#47612=CARTESIAN_POINT('Ctrl Pts',(-2.19951163212073,7.6015789348564,5.94708267688677));
#47613=CARTESIAN_POINT('Ctrl Pts',(-2.38594670398052,7.54513187565361,5.95489921852901));
#47614=CARTESIAN_POINT('Ctrl Pts',(-2.5699111494959,7.48194344296298,5.96271576017126));
#47615=CARTESIAN_POINT('Ctrl Pts',(-2.75409028479262,7.41868126824703,5.97054142385669));
#47616=CARTESIAN_POINT('Ctrl Pts',(-2.93579270219555,7.3486621210581,5.97836708754212));
#47617=CARTESIAN_POINT('Ctrl Pts',(-3.11449674320316,7.27212699535541,5.98619275122755));
#47618=CARTESIAN_POINT('Ctrl Pts',(-3.29331726924069,7.19554198160118,5.99402351593175));
#47619=CARTESIAN_POINT('Ctrl Pts',(-3.46913520710748,7.11243267504027,6.00185428063595));
#47620=CARTESIAN_POINT('Ctrl Pts',(-3.6414540154819,7.02308576432972,6.00968504534016));
#47621=CARTESIAN_POINT('Ctrl Pts',(-3.81402180621436,6.93360975683211,6.01752712466683));
#47622=CARTESIAN_POINT('Ctrl Pts',(-3.98308006430326,6.83787831662013,6.02536920399351));
#47623=CARTESIAN_POINT('Ctrl Pts',(-4.14816070635285,6.73622177145841,6.03321128332018));
#47624=CARTESIAN_POINT('Ctrl Pts',(-4.24068817453482,6.67924342056785,6.03760675777661));
#47625=CARTESIAN_POINT('Ctrl Pts',(-4.3319666145367,6.6204043905575,6.04200223223303));
#47626=CARTESIAN_POINT('Ctrl Pts',(-4.42191828936477,6.55976826131696,6.04639770668946));
#47627=CARTESIAN_POINT('Ctrl Pts',(-4.58340604536027,6.45090989417677,6.05428878051171));
#47628=CARTESIAN_POINT('Ctrl Pts',(-4.7411067374536,6.33592622752953,6.06217985433396));
#47629=CARTESIAN_POINT('Ctrl Pts',(-4.89452224960557,6.21510844218474,6.07007092815622));
#47630=CARTESIAN_POINT('Ctrl Pts',(-5.04776084545647,6.09442998196677,6.07795290211906));
#47631=CARTESIAN_POINT('Ctrl Pts',(-5.19672383319295,5.96793101483532,6.0858348760819));
#47632=CARTESIAN_POINT('Ctrl Pts',(-5.34094036450682,5.83594696881164,6.09371685004475));
#47633=CARTESIAN_POINT('Ctrl Pts',(-5.48501781815481,5.70409020384851,6.10159122289188));
#47634=CARTESIAN_POINT('Ctrl Pts',(-5.62435767852726,5.56675912887002,6.10946559573902));
#47635=CARTESIAN_POINT('Ctrl Pts',(-5.75852041490217,5.42433070812934,6.11733996858615));
#47636=CARTESIAN_POINT('Ctrl Pts',(-5.89257909164205,5.28201275807434,6.12520823389265));
#47637=CARTESIAN_POINT('Ctrl Pts',(-6.0214684068441,5.13460558984344,6.13307649919915));
#47638=CARTESIAN_POINT('Ctrl Pts',(-6.14478392051677,4.98252461811867,6.14094476450564));
#47639=CARTESIAN_POINT('Ctrl Pts',(-6.26802705681479,4.83053290703224,6.14880841170393));
#47640=CARTESIAN_POINT('Ctrl Pts',(-6.38570269162808,4.67387312693333,6.15667205890222));
#47641=CARTESIAN_POINT('Ctrl Pts',(-6.49744493742192,4.51299571074139,6.16453570610051));
#47642=CARTESIAN_POINT('Ctrl Pts',(-6.61176264344172,4.34841035594743,6.17258059639487));
#47643=CARTESIAN_POINT('Ctrl Pts',(-6.71986989774841,4.17941087149798,6.18062548668924));
#47644=CARTESIAN_POINT('Ctrl Pts',(-6.82141967250549,4.00651402737531,6.1886703769836));
#47645=CARTESIAN_POINT('Ctrl Pts',(-6.92063477014604,3.8375921630737,6.19653031146373));
#47646=CARTESIAN_POINT('Ctrl Pts',(-7.01359042491432,3.66495049636911,6.20439024594387));
#47647=CARTESIAN_POINT('Ctrl Pts',(-7.10000779725799,3.48909877746042,6.212250180424));
#47648=CARTESIAN_POINT('Ctrl Pts',(-7.18642677923157,3.31324378309705,6.22011026130508));
#47649=CARTESIAN_POINT('Ctrl Pts',(-7.26630708264474,3.13417892894322,6.22797034218617));
#47650=CARTESIAN_POINT('Ctrl Pts',(-7.33941668836165,2.95243690442293,6.23583042306725));
#47651=CARTESIAN_POINT('Ctrl Pts',(-7.41254015222441,2.77066043015481,6.24369199385033));
#47652=CARTESIAN_POINT('Ctrl Pts',(-7.47889023200438,2.58620609670518,6.25155356463341));
#47653=CARTESIAN_POINT('Ctrl Pts',(-7.5382836731742,2.39962502544777,6.25941513541648));
#47654=CARTESIAN_POINT('Ctrl Pts',(-7.60010670235002,2.20541154354125,6.26759829689555));
#47655=CARTESIAN_POINT('Ctrl Pts',(-7.65439183267923,2.00889405926646,6.27578145837461));
#47656=CARTESIAN_POINT('Ctrl Pts',(-7.70099040580724,1.81070918970022,6.28396461985367));
#47657=CARTESIAN_POINT('Ctrl Pts',(-7.74581800068916,1.62005633386632,6.29183678037303));
#47658=CARTESIAN_POINT('Ctrl Pts',(-7.78353249133439,1.42786084217599,6.29970894089239));
#47659=CARTESIAN_POINT('Ctrl Pts',(-7.81405419343074,1.23469755897039,6.30758110141175));
#47660=CARTESIAN_POINT('Ctrl Pts',(-7.84459391678191,1.04142022430274,6.31545790997499));
#47661=CARTESIAN_POINT('Ctrl Pts',(-7.86793234444799,0.847174302690902,
6.32333471853823));
#47662=CARTESIAN_POINT('Ctrl Pts',(-7.88404177619998,0.652538329244746,
6.33121152710147));
#47663=CARTESIAN_POINT('Ctrl Pts',(-7.90016949112144,0.457681456480474,
6.33909727533608));
#47664=CARTESIAN_POINT('Ctrl Pts',(-7.90905181413018,0.262433993324727,
6.3469830235707));
#47665=CARTESIAN_POINT('Ctrl Pts',(-7.91071310043852,0.067373901106895,
6.35486877180531));
#47666=CARTESIAN_POINT('Ctrl Pts',(-7.9109058139321,0.0447464276609003,
6.35578353892529));
#47667=CARTESIAN_POINT('Ctrl Pts',(-7.91100141416754,0.0221214693622712,
6.35669830604527));
#47668=CARTESIAN_POINT('Ctrl Pts',(-7.91099998419434,-0.000500077126143346,
6.35761307316525));
#47669=CARTESIAN_POINT('',(-7.911,-8.41493541514637E-12,8.35766849176337));
#47670=CARTESIAN_POINT('Ctrl Pts',(-7.9109999835323,-0.000497167457162866,
6.35768849598628));
#47671=CARTESIAN_POINT('Ctrl Pts',(-7.9108541427804,-2.20200474133999,6.44626926364471));
#47672=CARTESIAN_POINT('Ctrl Pts',(-6.9420229263903,-4.38621542289884,6.53485003130312));
#47673=CARTESIAN_POINT('Ctrl Pts',(-3.67820201487512,-7.34180684108019,
6.71201823469427));
#47674=CARTESIAN_POINT('Ctrl Pts',(-1.40868175870894,-8.08992666571484,
6.800605670427));
#47675=CARTESIAN_POINT('Ctrl Pts',(2.97309270522073,-7.65454228024946,6.97778054189245));
#47676=CARTESIAN_POINT('Ctrl Pts',(5.05102072676276,-6.47444880833699,7.06636797762517));
#47677=CARTESIAN_POINT('Ctrl Pts',(7.66951518848174,-2.93425195366914,7.24354284909062));
#47678=CARTESIAN_POINT('Ctrl Pts',(8.18956872247132,-0.601881960090737,
7.33213028482335));
#47679=CARTESIAN_POINT('Ctrl Pts',(7.32306689760962,3.71537198233198,7.5093051562888));
#47680=CARTESIAN_POINT('Ctrl Pts',(5.94329958849624,5.66643518937116,7.59789259202152));
#47681=CARTESIAN_POINT('Ctrl Pts',(2.16154501637046,7.92205913233216,7.77506746348697));
#47682=CARTESIAN_POINT('Ctrl Pts',(-0.210816529308643,8.2089496371298,7.8636548992197));
#47683=CARTESIAN_POINT('Ctrl Pts',(-4.4212390857713,6.91982244717388,8.04082977068514));
#47684=CARTESIAN_POINT('Ctrl Pts',(-6.22631625634721,5.35390358802899,8.12941720641787));
#47685=CARTESIAN_POINT('Ctrl Pts',(-7.65317280859726,2.31334857513741,8.26455925868819));
#47686=CARTESIAN_POINT('Ctrl Pts',(-7.91100000000123,1.15702837835696,8.31111387522578));
#47687=CARTESIAN_POINT('Ctrl Pts',(-7.911,-8.41493541514637E-12,8.35766849176337));
#47688=CARTESIAN_POINT('',(-7.90360519151496,-0.00207662742780917,10.3576684917634));
#47689=CARTESIAN_POINT('Ctrl Pts',(-7.911,-8.41493541514637E-12,8.35766849176337));
#47690=CARTESIAN_POINT('Ctrl Pts',(-7.91099999999766,-2.20167589667516,
8.4462559274961));
#47691=CARTESIAN_POINT('Ctrl Pts',(-6.94214576671907,-4.38610418339416,
8.53484336322882));
#47692=CARTESIAN_POINT('Ctrl Pts',(-3.67820201487515,-7.34180684108018,
8.71201823469427));
#47693=CARTESIAN_POINT('Ctrl Pts',(-1.40868175870897,-8.08992666571483,
8.800605670427));
#47694=CARTESIAN_POINT('Ctrl Pts',(2.9730927052207,-7.65454228024947,8.97778054189244));
#47695=CARTESIAN_POINT('Ctrl Pts',(5.05102072676273,-6.47444880833701,9.06636797762517));
#47696=CARTESIAN_POINT('Ctrl Pts',(7.66951518848173,-2.93425195366917,9.24354284909062));
#47697=CARTESIAN_POINT('Ctrl Pts',(8.18956872247132,-0.601881960090768,
9.33213028482334));
#47698=CARTESIAN_POINT('Ctrl Pts',(7.32306689760963,3.71537198233196,9.50930515628879));
#47699=CARTESIAN_POINT('Ctrl Pts',(5.94329958849626,5.66643518937113,9.59789259202152));
#47700=CARTESIAN_POINT('Ctrl Pts',(2.16154501637049,7.92205913233215,9.77506746348697));
#47701=CARTESIAN_POINT('Ctrl Pts',(-0.210816529308611,8.2089496371298,9.86365489921969));
#47702=CARTESIAN_POINT('Ctrl Pts',(-4.42123908577128,6.91982244717389,10.0408297706851));
#47703=CARTESIAN_POINT('Ctrl Pts',(-6.22631625634721,5.353903588029,10.1294172064179));
#47704=CARTESIAN_POINT('Ctrl Pts',(-7.65317280859726,2.31334857513742,10.2645592586882));
#47705=CARTESIAN_POINT('Ctrl Pts',(-7.91100000000123,1.15702837835698,10.3111138752258));
#47706=CARTESIAN_POINT('Ctrl Pts',(-7.911,-8.38551450499381E-12,10.3576684917634));
#47707=CARTESIAN_POINT('',(-7.91571978525191,-0.0020331227406836,12.3575752383775));
#47708=CARTESIAN_POINT('Ctrl Pts',(-7.89834820152432,-0.00355290765606358,
10.3576684917634));
#47709=CARTESIAN_POINT('Ctrl Pts',(-7.90111396095795,-1.2014871786324,10.4056583685572));
#47710=CARTESIAN_POINT('Ctrl Pts',(-7.08241423273656,-5.0426308771058,10.5597253981002));
#47711=CARTESIAN_POINT('Ctrl Pts',(-2.32675483040277,-8.41269614686096,
10.7668310040172));
#47712=CARTESIAN_POINT('Ctrl Pts',(3.05913169433092,-7.63406331823264,10.9789853095152));
#47713=CARTESIAN_POINT('Ctrl Pts',(7.4923240719073,-4.47798219086958,11.191139615013));
#47714=CARTESIAN_POINT('Ctrl Pts',(8.91679478215701,2.84829431800013,11.4563324968853));
#47715=CARTESIAN_POINT('Ctrl Pts',(2.41200260105483,9.04380386318945,11.7745639551321));
#47716=CARTESIAN_POINT('Ctrl Pts',(-5.80949993071132,7.0346858171147,12.0749618174482));
#47717=CARTESIAN_POINT('Ctrl Pts',(-7.89632373226713,2.18652121168757,12.2692825270153));
#47718=CARTESIAN_POINT('Ctrl Pts',(-7.91703408569381,-0.00202294616919351,
12.3575260838335));
#47719=CARTESIAN_POINT('',(-7.91661424246722,0.00191610784238723,14.357737223299));
#47720=CARTESIAN_POINT('Ctrl Pts',(-7.91099971462202,-0.00206967004347107,
12.3577517679683));
#47721=CARTESIAN_POINT('Ctrl Pts',(-7.9103927569587,-2.20304480169943,12.4463114449661));
#47722=CARTESIAN_POINT('Ctrl Pts',(-6.94163439087416,-4.38656726580578,
12.5348711219638));
#47723=CARTESIAN_POINT('Ctrl Pts',(-3.67820201487507,-7.34180684108022,
12.7120182346943));
#47724=CARTESIAN_POINT('Ctrl Pts',(-1.40868175870889,-8.08992666571485,
12.800605670427));
#47725=CARTESIAN_POINT('Ctrl Pts',(2.97309270522078,-7.65454228024944,12.9777805418925));
#47726=CARTESIAN_POINT('Ctrl Pts',(5.0510207267628,-6.47444880833696,13.0663679776252));
#47727=CARTESIAN_POINT('Ctrl Pts',(7.66951518848176,-2.93425195366909,13.2435428490906));
#47728=CARTESIAN_POINT('Ctrl Pts',(8.18956872247133,-0.601881960090685,
13.3321302848233));
#47729=CARTESIAN_POINT('Ctrl Pts',(7.3230668976096,3.71537198233203,13.5093051562888));
#47730=CARTESIAN_POINT('Ctrl Pts',(5.9432995884962,5.6664351893712,13.5978925920215));
#47731=CARTESIAN_POINT('Ctrl Pts',(2.16154501637041,7.92205913233217,13.775067463487));
#47732=CARTESIAN_POINT('Ctrl Pts',(-0.210816529308695,8.2089496371298,13.8636548992197));
#47733=CARTESIAN_POINT('Ctrl Pts',(-4.42123908577134,6.91982244717385,14.0408297706851));
#47734=CARTESIAN_POINT('Ctrl Pts',(-6.22631625634725,5.35390358802895,14.1294172064179));
#47735=CARTESIAN_POINT('Ctrl Pts',(-7.65289632442553,2.31393774812261,14.2645330720065));
#47736=CARTESIAN_POINT('Ctrl Pts',(-7.91070987367968,1.15832918971538,14.3110615018624));
#47737=CARTESIAN_POINT('Ctrl Pts',(-7.91099975527532,0.00195246306002456,
14.3575899317182));
#47738=CARTESIAN_POINT('',(-7.90441257296093,0.00229462530749312,16.3576684917634));
#47739=CARTESIAN_POINT('Ctrl Pts',(-7.91882171999131,0.00190181386983465,
14.3577951347062));
#47740=CARTESIAN_POINT('Ctrl Pts',(-7.90092880425392,-2.31733288374248,
14.4514124495886));
#47741=CARTESIAN_POINT('Ctrl Pts',(-5.60174024730873,-7.29337738801806,
14.65110691722));
#47742=CARTESIAN_POINT('Ctrl Pts',(2.87741498209291,-8.90744030178522,14.9568785376003));
#47743=CARTESIAN_POINT('Ctrl Pts',(8.00355842970691,-3.48285758573526,15.2220714194727));
#47744=CARTESIAN_POINT('Ctrl Pts',(7.9874613863806,1.95899721059107,15.4342257249706));
#47745=CARTESIAN_POINT('Ctrl Pts',(5.483858582018,6.79076870116109,15.6463800304684));
#47746=CARTESIAN_POINT('Ctrl Pts',(-1.57046161563201,9.22798244595634,15.9115729123407));
#47747=CARTESIAN_POINT('Ctrl Pts',(-7.21150187483662,4.76683328138724,16.166348591564));
#47748=CARTESIAN_POINT('Ctrl Pts',(-7.90585355722926,1.066076564084,16.3150471180381));
#47749=CARTESIAN_POINT('Ctrl Pts',(-7.90052382745844,0.00364920788198668,
16.3576684917634));
#47750=CARTESIAN_POINT('',(-7.911,-8.60200799479571E-12,18.3576684917634));
#47751=CARTESIAN_POINT('Ctrl Pts',(-7.911,-8.60422844084496E-12,16.3576684917634));
#47752=CARTESIAN_POINT('Ctrl Pts',(-7.9109999999976,-2.20167589667533,16.4462559274961));
#47753=CARTESIAN_POINT('Ctrl Pts',(-6.94214576671898,-4.38610418339429,
16.5348433632288));
#47754=CARTESIAN_POINT('Ctrl Pts',(-3.67820201487504,-7.34180684108023,
16.7120182346943));
#47755=CARTESIAN_POINT('Ctrl Pts',(-1.40868175870887,-8.08992666571484,
16.800605670427));
#47756=CARTESIAN_POINT('Ctrl Pts',(2.97309270522075,-7.65454228024944,16.9777805418924));
#47757=CARTESIAN_POINT('Ctrl Pts',(5.05102072676276,-6.47444880833699,17.0663679776252));
#47758=CARTESIAN_POINT('Ctrl Pts',(7.66951518848173,-2.93425195366916,17.2435428490906));
#47759=CARTESIAN_POINT('Ctrl Pts',(8.18956872247132,-0.601881960090787,
17.3321302848233));
#47760=CARTESIAN_POINT('Ctrl Pts',(7.32306689760966,3.7153719823319,17.5093051562888));
#47761=CARTESIAN_POINT('Ctrl Pts',(5.94329958849631,5.66643518937107,17.5978925920215));
#47762=CARTESIAN_POINT('Ctrl Pts',(2.1615450163706,7.92205913233211,17.775067463487));
#47763=CARTESIAN_POINT('Ctrl Pts',(-0.210816529308475,8.2089496371298,17.8636548992197));
#47764=CARTESIAN_POINT('Ctrl Pts',(-4.42123908577112,6.91982244717398,18.0408297706851));
#47765=CARTESIAN_POINT('Ctrl Pts',(-6.22631625634706,5.35390358802916,18.1294172064179));
#47766=CARTESIAN_POINT('Ctrl Pts',(-7.65317280859725,2.31334857513751,18.2645592586882));
#47767=CARTESIAN_POINT('Ctrl Pts',(-7.91100000000126,1.15702837835691,18.3111138752258));
#47768=CARTESIAN_POINT('Ctrl Pts',(-7.911,-8.60200799479571E-12,18.3576684917634));
#47769=CARTESIAN_POINT('',(-7.911,-8.71303029725823E-12,20.3576684917634));
#47770=CARTESIAN_POINT('Ctrl Pts',(-7.911,-8.60200799479571E-12,18.3576684917634));
#47771=CARTESIAN_POINT('Ctrl Pts',(-7.91099999999761,-2.20167589667534,
18.4462559274961));
#47772=CARTESIAN_POINT('Ctrl Pts',(-6.94214576671897,-4.38610418339433,
18.5348433632288));
#47773=CARTESIAN_POINT('Ctrl Pts',(-3.67820201487497,-7.34180684108027,
18.7120182346943));
#47774=CARTESIAN_POINT('Ctrl Pts',(-1.40868175870878,-8.08992666571486,
18.800605670427));
#47775=CARTESIAN_POINT('Ctrl Pts',(2.97309270522088,-7.6545422802494,18.9777805418925));
#47776=CARTESIAN_POINT('Ctrl Pts',(5.05102072676288,-6.47444880833689,19.0663679776252));
#47777=CARTESIAN_POINT('Ctrl Pts',(7.6695151884818,-2.93425195366899,19.2435428490906));
#47778=CARTESIAN_POINT('Ctrl Pts',(8.18956872247134,-0.601881960090575,
19.3321302848234));
#47779=CARTESIAN_POINT('Ctrl Pts',(7.32306689760955,3.71537198233213,19.5093051562888));
#47780=CARTESIAN_POINT('Ctrl Pts',(5.94329958849612,5.66643518937128,19.5978925920215));
#47781=CARTESIAN_POINT('Ctrl Pts',(2.1615450163703,7.9220591323322,19.775067463487));
#47782=CARTESIAN_POINT('Ctrl Pts',(-0.210816529308805,8.2089496371298,19.8636548992197));
#47783=CARTESIAN_POINT('Ctrl Pts',(-4.42123908577143,6.91982244717379,20.0408297706851));
#47784=CARTESIAN_POINT('Ctrl Pts',(-6.22631625634732,5.35390358802887,20.1294172064179));
#47785=CARTESIAN_POINT('Ctrl Pts',(-7.65317280859733,2.31334857513722,20.2645592586882));
#47786=CARTESIAN_POINT('Ctrl Pts',(-7.91100000000127,1.15702837835671,20.3111138752258));
#47787=CARTESIAN_POINT('Ctrl Pts',(-7.911,-8.71303029725823E-12,20.3576684917634));
#47788=CARTESIAN_POINT('',(-7.911,-8.76687611395255E-12,22.3576684917634));
#47789=CARTESIAN_POINT('Ctrl Pts',(-7.911,-8.71303029725823E-12,20.3576684917634));
#47790=CARTESIAN_POINT('Ctrl Pts',(-7.91099999999757,-2.20167589667551,
20.4462559274961));
#47791=CARTESIAN_POINT('Ctrl Pts',(-6.94214576671885,-4.38610418339453,
20.5348433632288));
#47792=CARTESIAN_POINT('Ctrl Pts',(-3.67820201487467,-7.34180684108043,
20.7120182346943));
#47793=CARTESIAN_POINT('Ctrl Pts',(-1.40868175870837,-8.08992666571495,
20.800605670427));
#47794=CARTESIAN_POINT('Ctrl Pts',(2.97309270522137,-7.65454228024923,20.9777805418925));
#47795=CARTESIAN_POINT('Ctrl Pts',(5.05102072676335,-6.47444880833655,21.0663679776252));
#47796=CARTESIAN_POINT('Ctrl Pts',(7.66951518848206,-2.93425195366835,21.2435428490907));
#47797=CARTESIAN_POINT('Ctrl Pts',(8.18956872247141,-0.601881960089817,
21.3321302848234));
#47798=CARTESIAN_POINT('Ctrl Pts',(7.32306689760917,3.71537198233291,21.5093051562888));
#47799=CARTESIAN_POINT('Ctrl Pts',(5.94329958849549,5.66643518937196,21.5978925920216));
#47800=CARTESIAN_POINT('Ctrl Pts',(2.1615450163693,7.92205913233249,21.775067463487));
#47801=CARTESIAN_POINT('Ctrl Pts',(-0.210816529309916,8.20894963712979,
21.8636548992197));
#47802=CARTESIAN_POINT('Ctrl Pts',(-4.42123908577247,6.91982244717315,22.0408297706852));
#47803=CARTESIAN_POINT('Ctrl Pts',(-6.22631625634817,5.3539035880279,22.1294172064179));
#47804=CARTESIAN_POINT('Ctrl Pts',(-7.65317280859753,2.31334857513634,22.2645592586882));
#47805=CARTESIAN_POINT('Ctrl Pts',(-7.91100000000128,1.15702837835624,22.3111138752258));
#47806=CARTESIAN_POINT('Ctrl Pts',(-7.911,-8.76687611395255E-12,22.3576684917634));
#47807=CARTESIAN_POINT('',(-7.90652056602762,-0.000845387666311545,24.3576684917634));
#47808=CARTESIAN_POINT('Ctrl Pts',(-7.911,-8.76687611395255E-12,22.3576684917634));
#47809=CARTESIAN_POINT('Ctrl Pts',(-7.91099999999756,-2.20167589667553,
22.4462559274961));
#47810=CARTESIAN_POINT('Ctrl Pts',(-6.94214576671886,-4.38610418339451,
22.5348433632288));
#47811=CARTESIAN_POINT('Ctrl Pts',(-3.67820201487475,-7.34180684108038,
22.7120182346943));
#47812=CARTESIAN_POINT('Ctrl Pts',(-1.40868175870851,-8.08992666571492,
22.800605670427));
#47813=CARTESIAN_POINT('Ctrl Pts',(2.97309270522117,-7.65454228024929,22.9777805418925));
#47814=CARTESIAN_POINT('Ctrl Pts',(5.05102072676315,-6.4744488083367,23.0663679776252));
#47815=CARTESIAN_POINT('Ctrl Pts',(7.66951518848194,-2.93425195366865,23.2435428490906));
#47816=CARTESIAN_POINT('Ctrl Pts',(8.18956872247137,-0.60188196009019,23.3321302848234));
#47817=CARTESIAN_POINT('Ctrl Pts',(7.32306689760936,3.71537198233251,23.5093051562888));
#47818=CARTESIAN_POINT('Ctrl Pts',(5.94329958849582,5.6664351893716,23.5978925920215));
#47819=CARTESIAN_POINT('Ctrl Pts',(2.16154501636984,7.92205913233233,23.775067463487));
#47820=CARTESIAN_POINT('Ctrl Pts',(-0.210816529309308,8.20894963712979,
23.8636548992197));
#47821=CARTESIAN_POINT('Ctrl Pts',(-4.42123908577189,6.91982244717351,24.0408297706852));
#47822=CARTESIAN_POINT('Ctrl Pts',(-6.22631625634769,5.35390358802845,24.1294172064179));
#47823=CARTESIAN_POINT('Ctrl Pts',(-7.65317280859741,2.31334857513685,24.2645592586882));
#47824=CARTESIAN_POINT('Ctrl Pts',(-7.91100000000127,1.15702837835653,24.3111138752258));
#47825=CARTESIAN_POINT('Ctrl Pts',(-7.911,-8.70858940515973E-12,24.3576684917634));
#47826=CARTESIAN_POINT('',(-7.91126158341924,-0.001405488932413,26.3574794111892));
#47827=CARTESIAN_POINT('Ctrl Pts',(-7.90426632794342,-0.00127082201034442,
24.3576684917634));
#47828=CARTESIAN_POINT('Ctrl Pts',(-7.9058497364464,-1.21571962861209,24.4063864228439));
#47829=CARTESIAN_POINT('Ctrl Pts',(-7.05373471379606,-5.07204213544585,
24.5611815066734));
#47830=CARTESIAN_POINT('Ctrl Pts',(-1.05237152432548,-9.30131839492834,
24.8220537432516));
#47831=CARTESIAN_POINT('Ctrl Pts',(7.26337396731614,-5.90351958362561,25.1402852014985));
#47832=CARTESIAN_POINT('Ctrl Pts',(8.88769428104811,2.91399200048715,25.4585166597452));
#47833=CARTESIAN_POINT('Ctrl Pts',(2.35795283017753,9.05804632986584,25.7767481179922));
#47834=CARTESIAN_POINT('Ctrl Pts',(-5.84663248951178,7.00016475381016,26.0764023684734));
#47835=CARTESIAN_POINT('Ctrl Pts',(-7.88980521203094,2.17032634514267,26.2699794662058));
#47836=CARTESIAN_POINT('Ctrl Pts',(-7.91126158341924,-0.001405488932413,
26.3574794111892));
#47837=CARTESIAN_POINT('',(-7.91099988262543,0.00136275470605475,28.3577729727994));
#47838=CARTESIAN_POINT('Ctrl Pts',(-7.91099986978392,-0.00139804521138159,
26.3577247441145));
#47839=CARTESIAN_POINT('Ctrl Pts',(-7.91058982688626,-2.20260059530338,
26.4462934290635));
#47840=CARTESIAN_POINT('Ctrl Pts',(-6.94180033678989,-4.38641699152991,
26.5348621140125));
#47841=CARTESIAN_POINT('Ctrl Pts',(-3.67820201487476,-7.34180684108038,
26.7120182346943));
#47842=CARTESIAN_POINT('Ctrl Pts',(-1.40868175870852,-8.08992666571491,
26.800605670427));
#47843=CARTESIAN_POINT('Ctrl Pts',(2.97309270522116,-7.6545422802493,26.9777805418925));
#47844=CARTESIAN_POINT('Ctrl Pts',(5.05102072676314,-6.4744488083367,27.0663679776252));
#47845=CARTESIAN_POINT('Ctrl Pts',(7.66951518848193,-2.93425195366865,27.2435428490906));
#47846=CARTESIAN_POINT('Ctrl Pts',(8.18956872247137,-0.601881960090193,
27.3321302848234));
#47847=CARTESIAN_POINT('Ctrl Pts',(7.32306689760936,3.7153719823325,27.5093051562888));
#47848=CARTESIAN_POINT('Ctrl Pts',(5.94329958849583,5.6664351893716,27.5978925920215));
#47849=CARTESIAN_POINT('Ctrl Pts',(2.16154501636984,7.92205913233233,27.775067463487));
#47850=CARTESIAN_POINT('Ctrl Pts',(-0.210816529309305,8.20894963712979,
27.8636548992197));
#47851=CARTESIAN_POINT('Ctrl Pts',(-4.42123908577189,6.91982244717351,28.0408297706852));
#47852=CARTESIAN_POINT('Ctrl Pts',(-6.22631625634769,5.35390358802845,28.1294172064179));
#47853=CARTESIAN_POINT('Ctrl Pts',(-7.65298073882793,2.31375786554483,28.2645410671589));
#47854=CARTESIAN_POINT('Ctrl Pts',(-7.91079846890045,1.1579320415085,28.3110774921671));
#47855=CARTESIAN_POINT('Ctrl Pts',(-7.91099988189791,0.00135634950828223,
28.3576139171754));
#47856=CARTESIAN_POINT('',(-7.91116372059493,0.00341841640445254,30.3575613031839));
#47857=CARTESIAN_POINT('Ctrl Pts',(-7.91099988262543,0.00136275470605475,
28.3577729727994));
#47858=CARTESIAN_POINT('Ctrl Pts',(-7.91103304674915,-0.191160065200167,
28.3655621021175));
#47859=CARTESIAN_POINT('Ctrl Pts',(-7.9040340849586,-0.383975128877379,
28.3733512314357));
#47860=CARTESIAN_POINT('Ctrl Pts',(-7.88996501489689,-0.576518051498078,
28.3811403607538));
#47861=CARTESIAN_POINT('Ctrl Pts',(-7.87591085565761,-0.768856911354393,
28.3889212349191));
#47862=CARTESIAN_POINT('Ctrl Pts',(-7.85480153216924,-0.960923852310489,
28.3967021090843));
#47863=CARTESIAN_POINT('Ctrl Pts',(-7.8266510171243,-1.15215227125028,28.4044829832496));
#47864=CARTESIAN_POINT('Ctrl Pts',(-7.7985247063564,-1.34321626884203,28.4122571672909));
#47865=CARTESIAN_POINT('Ctrl Pts',(-7.76336931069869,-1.53344282962111,
28.4200313513323));
#47866=CARTESIAN_POINT('Ctrl Pts',(-7.7212507718984,-1.72226813169681,28.4278055353736));
#47867=CARTESIAN_POINT('Ctrl Pts',(-7.67916003024605,-1.91096881394933,
28.4355745886543));
#47868=CARTESIAN_POINT('Ctrl Pts',(-7.63011537485797,-2.09826973266808,
28.4433436419349));
#47869=CARTESIAN_POINT('Ctrl Pts',(-7.57423424038156,-2.28361482562879,
28.4511126952156));
#47870=CARTESIAN_POINT('Ctrl Pts',(-7.51737570576517,-2.47220173394455,
28.4590176346738));
#47871=CARTESIAN_POINT('Ctrl Pts',(-7.45343937646802,-2.65876339351354,
28.4669225741321));
#47872=CARTESIAN_POINT('Ctrl Pts',(-7.38260290411685,-2.84272674735462,
28.4748275135903));
#47873=CARTESIAN_POINT('Ctrl Pts',(-7.31302578234416,-3.02341954934032,
28.4825919168283));
#47874=CARTESIAN_POINT('Ctrl Pts',(-7.23679194854965,-3.20160531616111,
28.4903563200663));
#47875=CARTESIAN_POINT('Ctrl Pts',(-7.15411941173772,-3.37675827423248,
28.4981207233043));
#47876=CARTESIAN_POINT('Ctrl Pts',(-7.07144832537299,-3.55190815933518,
28.5058849903198));
#47877=CARTESIAN_POINT('Ctrl Pts',(-6.98233891285306,-3.72402501899075,
28.5136492573354));
#47878=CARTESIAN_POINT('Ctrl Pts',(-6.88705639282087,-3.89260519987646,
28.5214135243509));
#47879=CARTESIAN_POINT('Ctrl Pts',(-6.79175831210266,-4.06121291176431,
28.5291790593569));
#47880=CARTESIAN_POINT('Ctrl Pts',(-6.69028529202385,-4.22628248442844,
28.5369445943628));
#47881=CARTESIAN_POINT('Ctrl Pts',(-6.58294740138362,-4.3873368357828,28.5447101293687));
#47882=CARTESIAN_POINT('Ctrl Pts',(-6.47222914983099,-4.55346322489422,
28.5527202221058));
#47883=CARTESIAN_POINT('Ctrl Pts',(-6.35527081706428,-4.71531701900264,
28.5607303148429));
#47884=CARTESIAN_POINT('Ctrl Pts',(-6.23245913855011,-4.87240947440824,
28.5687404075799));
#47885=CARTESIAN_POINT('Ctrl Pts',(-6.1132398452078,-5.02490679184133,28.5765161957401));
#47886=CARTESIAN_POINT('Ctrl Pts',(-5.98850508880372,-5.17291715927829,
28.5842919839002));
#47887=CARTESIAN_POINT('Ctrl Pts',(-5.8586475387481,-5.31602953497446,28.5920677720604));
#47888=CARTESIAN_POINT('Ctrl Pts',(-5.72292057371531,-5.46561042883512,
28.6001950170859));
#47889=CARTESIAN_POINT('Ctrl Pts',(-5.58159729495791,-5.60983996416175,
28.6083222621114));
#47890=CARTESIAN_POINT('Ctrl Pts',(-5.43516607510868,-5.74829459370235,
28.6164495071369));
#47891=CARTESIAN_POINT('Ctrl Pts',(-5.28873485525947,-5.88674922324294,
28.6245767521624));
#47892=CARTESIAN_POINT('Ctrl Pts',(-5.13719606725288,-6.01942870847893,
28.632703997188));
#47893=CARTESIAN_POINT('Ctrl Pts',(-4.98107366476083,-6.14596014844109,
28.6408312422135));
#47894=CARTESIAN_POINT('Ctrl Pts',(-4.82135188567672,-6.27540875016794,
28.6491458595509));
#47895=CARTESIAN_POINT('Ctrl Pts',(-4.65644385003665,-6.39873902158748,
28.6574604768884));
#47896=CARTESIAN_POINT('Ctrl Pts',(-4.48683443849475,-6.51553817589441,
28.6657750942259));
#47897=CARTESIAN_POINT('Ctrl Pts',(-4.31743465568261,-6.63219297230204,
28.6740794351131));
#47898=CARTESIAN_POINT('Ctrl Pts',(-4.14334532639385,-6.74233258546919,
28.6823837760004));
#47899=CARTESIAN_POINT('Ctrl Pts',(-3.96508381650821,-6.84558480541032,
28.6906881168877));
#47900=CARTESIAN_POINT('Ctrl Pts',(-3.78703084525463,-6.94871623608675,
28.6989827429695));
#47901=CARTESIAN_POINT('Ctrl Pts',(-3.60481568117551,-7.04497619738786,
28.7072773690513));
#47902=CARTESIAN_POINT('Ctrl Pts',(-3.41898474863096,-7.1340356242893,28.7155719951331));
#47903=CARTESIAN_POINT('Ctrl Pts',(-3.23343362076888,-7.22296095486823,
28.723854132039));
#47904=CARTESIAN_POINT('Ctrl Pts',(-3.04427785290794,-7.30470726108928,
28.7321362689448));
#47905=CARTESIAN_POINT('Ctrl Pts',(-2.85208860341916,-7.37899123175022,
28.7404184058506));
#47906=CARTESIAN_POINT('Ctrl Pts',(-2.66007658993801,-7.45320669808832,
28.7486929050094));
#47907=CARTESIAN_POINT('Ctrl Pts',(-2.46503694599074,-7.51997344672542,
28.7569674041682));
#47908=CARTESIAN_POINT('Ctrl Pts',(-2.26756262496539,-7.57905539904941,
28.7652419033269));
#47909=CARTESIAN_POINT('Ctrl Pts',(-2.07031543065522,-7.6380693977798,28.7735068855024));
#47910=CARTESIAN_POINT('Ctrl Pts',(-1.87063942731905,-7.68941615348493,
28.7817718676779));
#47911=CARTESIAN_POINT('Ctrl Pts',(-1.66914488557447,-7.73290866045633,
28.7900368498533));
#47912=CARTESIAN_POINT('Ctrl Pts',(-1.58861091931513,-7.75029188115623,
28.7933402236812));
#47913=CARTESIAN_POINT('Ctrl Pts',(-1.50778664199549,-7.76642096191549,
28.796643597509));
#47914=CARTESIAN_POINT('Ctrl Pts',(-1.42671173387857,-7.7812861808581,28.7999469713369));
#47915=CARTESIAN_POINT('Ctrl Pts',(-1.22383658821642,-7.81848367547545,
28.8082130608344));
#47916=CARTESIAN_POINT('Ctrl Pts',(-1.01962085420059,-7.84772174840313,
28.816479150332));
#47917=CARTESIAN_POINT('Ctrl Pts',(-0.814700864793647,-7.86893788899776,
28.8247452398296));
#47918=CARTESIAN_POINT('Ctrl Pts',(-0.609596590557578,-7.89017310929688,
28.8330187630328));
#47919=CARTESIAN_POINT('Ctrl Pts',(-0.40378708867809,-7.90337196488202,
28.8412922862361));
#47920=CARTESIAN_POINT('Ctrl Pts',(-0.19791119255603,-7.90852401904812,
28.8495658094393));
#47921=CARTESIAN_POINT('Ctrl Pts',(0.00816323896655843,-7.91368104157214,
28.8578473111737));
#47922=CARTESIAN_POINT('Ctrl Pts',(0.214303899246248,-7.9107757632299,28.866128812908));
#47923=CARTESIAN_POINT('Ctrl Pts',(0.419873743605476,-7.89984981119456,
28.8744103146424));
#47924=CARTESIAN_POINT('Ctrl Pts',(0.625785857325099,-7.88890566768456,
28.8827056048987));
#47925=CARTESIAN_POINT('Ctrl Pts',(0.831124961246783,-7.8699141674667,28.8910008951549));
#47926=CARTESIAN_POINT('Ctrl Pts',(1.03525887144275,-7.84296883004766,28.8992961854112));
#47927=CARTESIAN_POINT('Ctrl Pts',(1.23957791186844,-7.81599905574548,28.9075989987144));
#47928=CARTESIAN_POINT('Ctrl Pts',(1.44268928701813,-7.78106109062025,28.9159018120176));
#47929=CARTESIAN_POINT('Ctrl Pts',(1.6439714750191,-7.73829947658551,28.9242046253209));
#47930=CARTESIAN_POINT('Ctrl Pts',(1.84556233314544,-7.69547228678921,28.9325201711487));
#47931=CARTESIAN_POINT('Ctrl Pts',(2.04531811129274,-7.64479753368419,28.9408357169766));
#47932=CARTESIAN_POINT('Ctrl Pts',(2.24263107276241,-7.58646998751597,28.9491512628045));
#47933=CARTESIAN_POINT('Ctrl Pts',(2.32102460846675,-7.5632961294023,28.9524550753564));
#47934=CARTESIAN_POINT('Ctrl Pts',(2.39903274847824,-7.53891480491464,28.9557588879083));
#47935=CARTESIAN_POINT('Ctrl Pts',(2.47661825383057,-7.51334033734618,28.9590627004603));
#47936=CARTESIAN_POINT('Ctrl Pts',(2.66236678009493,-7.45211215252913,28.9669724035651));
#47937=CARTESIAN_POINT('Ctrl Pts',(2.84607876551478,-7.38391403888483,28.9748821066698));
#47938=CARTESIAN_POINT('Ctrl Pts',(3.0271940501256,-7.30889986132552,28.9827918097746));
#47939=CARTESIAN_POINT('Ctrl Pts',(3.2081255844522,-7.23396178930571,28.9906934881001));
#47940=CARTESIAN_POINT('Ctrl Pts',(3.38646534987413,-7.15222155880661,28.9985951664255));
#47941=CARTESIAN_POINT('Ctrl Pts',(3.56166825101636,-7.06388280407469,29.006496844751));
#47942=CARTESIAN_POINT('Ctrl Pts',(3.73672585699575,-6.97561730836798,29.0143919702418));
#47943=CARTESIAN_POINT('Ctrl Pts',(3.90865147509959,-6.88076434409402,29.0222870957326));
#47944=CARTESIAN_POINT('Ctrl Pts',(4.07691964949858,-6.77957573683873,29.0301822212234));
#47945=CARTESIAN_POINT('Ctrl Pts',(4.24507944322176,-6.67845230465102,29.0380722615041));
#47946=CARTESIAN_POINT('Ctrl Pts',(4.40958619258182,-6.57100153701387,29.0459623017847));
#47947=CARTESIAN_POINT('Ctrl Pts',(4.56993848670113,-6.45752144617173,29.0538523420653));
#47948=CARTESIAN_POINT('Ctrl Pts',(4.73021719035728,-6.34409343473693,29.0617387613705));
#47949=CARTESIAN_POINT('Ctrl Pts',(4.88634495736857,-6.22464181268815,29.0696251806757));
#47950=CARTESIAN_POINT('Ctrl Pts',(5.03784861781131,-6.09950836576332,29.0775115999808));
#47951=CARTESIAN_POINT('Ctrl Pts',(5.18931079779809,-5.9744091793469,29.0853958600493));
#47952=CARTESIAN_POINT('Ctrl Pts',(5.33615112921285,-5.84363148792599,29.0932801201177));
#47953=CARTESIAN_POINT('Ctrl Pts',(5.477928631778,-5.707558050966,29.1011643801862));
#47954=CARTESIAN_POINT('Ctrl Pts',(5.61972268679212,-5.5714687275037,29.1090495607379));
#47955=CARTESIAN_POINT('Ctrl Pts',(5.75645247847028,-5.43008265680269,29.1169347412895));
#47956=CARTESIAN_POINT('Ctrl Pts',(5.88771263608965,-5.28382067398491,29.1248199218412));
#47957=CARTESIAN_POINT('Ctrl Pts',(6.01898916572442,-5.13754044798137,29.1327060859076));
#47958=CARTESIAN_POINT('Ctrl Pts',(6.14479447103222,-4.98638335416747,29.140592249974));
#47959=CARTESIAN_POINT('Ctrl Pts',(6.26476238886679,-4.830804613213,29.1484784140404));
#47960=CARTESIAN_POINT('Ctrl Pts',(6.38476539877375,-4.67518036358808,29.1563668849055));
#47961=CARTESIAN_POINT('Ctrl Pts',(6.49892740802877,-4.51513216233616,29.1642553557706));
#47962=CARTESIAN_POINT('Ctrl Pts',(6.60692449258012,-4.3511457972981,29.1721438266358));
#47963=CARTESIAN_POINT('Ctrl Pts',(6.71497128802812,-4.18708394958124,29.1800359285522));
#47964=CARTESIAN_POINT('Ctrl Pts',(6.81684731459258,-4.01908061335109,29.1879280304687));
#47965=CARTESIAN_POINT('Ctrl Pts',(6.9122735380583,-3.8476480523898,29.1958201323852));
#47966=CARTESIAN_POINT('Ctrl Pts',(7.00781038930819,-3.6760167493672,29.2037213836289));
#47967=CARTESIAN_POINT('Ctrl Pts',(7.09688233433858,-3.50094858194217,29.2116226348727));
#47968=CARTESIAN_POINT('Ctrl Pts',(7.17925711742028,-3.32297882057204,29.2195238861164));
#47969=CARTESIAN_POINT('Ctrl Pts',(7.26168648444222,-3.14489113123344,29.2274303729603));
#47970=CARTESIAN_POINT('Ctrl Pts',(7.33740971002179,-2.96389833188598,29.2353368598041));
#47971=CARTESIAN_POINT('Ctrl Pts',(7.40624366716349,-2.78055313608653,29.243243346648));
#47972=CARTESIAN_POINT('Ctrl Pts',(7.4751724545044,-2.59695535185308,29.2511607259896));
#47973=CARTESIAN_POINT('Ctrl Pts',(7.53719290699625,-2.41099902363484,29.2590781053312));
#47974=CARTESIAN_POINT('Ctrl Pts',(7.59217215418576,-2.22325054395728,29.2669954846728));
#47975=CARTESIAN_POINT('Ctrl Pts',(7.6160105701153,-2.14184480310993,29.2704283760176));
#47976=CARTESIAN_POINT('Ctrl Pts',(7.63852589598784,-2.06010225280555,29.2738612673623));
#47977=CARTESIAN_POINT('Ctrl Pts',(7.65971031677736,-1.97806947882386,29.2772941587071));
#47978=CARTESIAN_POINT('Ctrl Pts',(7.70810110523076,-1.79068504894333,29.2851357853674));
#47979=CARTESIAN_POINT('Ctrl Pts',(7.74968780417034,-1.60122867415708,29.2929774120277));
#47980=CARTESIAN_POINT('Ctrl Pts',(7.78428804038756,-1.41024136383784,29.3008190386881));
#47981=CARTESIAN_POINT('Ctrl Pts',(7.81884753743351,-1.219478926687,29.3086514324238));
#47982=CARTESIAN_POINT('Ctrl Pts',(7.84643688910024,-1.02718948531261,29.3164838261596));
#47983=CARTESIAN_POINT('Ctrl Pts',(7.86692331808896,-0.833929557761398,
29.3243162198953));
#47984=CARTESIAN_POINT('Ctrl Pts',(7.88738961390277,-0.640859557694782,
29.3321409162938));
#47985=CARTESIAN_POINT('Ctrl Pts',(7.90076685114784,-0.446821317721075,
29.3399656126923));
#47986=CARTESIAN_POINT('Ctrl Pts',(7.90697314235659,-0.252382103271008,
29.3477903090908));
#47987=CARTESIAN_POINT('Ctrl Pts',(7.9131745417304,-0.0580961469445164,
29.355608838018));
#47988=CARTESIAN_POINT('Ctrl Pts',(7.91221624117949,0.136589804671775,29.3634273669451));
#47989=CARTESIAN_POINT('Ctrl Pts',(7.90406807064486,0.331102604357672,29.3712458958722));
#47990=CARTESIAN_POINT('Ctrl Pts',(7.89592473796643,0.525499914934816,29.379059782663));
#47991=CARTESIAN_POINT('Ctrl Pts',(7.88060005345888,0.71972392801215,29.3868736694538));
#47992=CARTESIAN_POINT('Ctrl Pts',(7.85811591774078,0.913200538408173,29.3946875562446));
#47993=CARTESIAN_POINT('Ctrl Pts',(7.83564076036415,1.10659988992728,29.4024983228023));
#47994=CARTESIAN_POINT('Ctrl Pts',(7.8060118882968,1.2992520845273,29.41030908936));
#47995=CARTESIAN_POINT('Ctrl Pts',(7.76930314839567,1.49058699455251,29.4181198559177));
#47996=CARTESIAN_POINT('Ctrl Pts',(7.73259586748839,1.68191429994578,29.4259303120354));
#47997=CARTESIAN_POINT('Ctrl Pts',(7.68880933669557,1.87192407799625,29.4337407681532));
#47998=CARTESIAN_POINT('Ctrl Pts',(7.63806881440613,2.06005480179451,29.4415512242709));
#47999=CARTESIAN_POINT('Ctrl Pts',(7.5873268927913,2.24819071387396,29.4493618957859));
#48000=CARTESIAN_POINT('Ctrl Pts',(7.52963068854188,2.43444712842404,29.4571725673009));
#48001=CARTESIAN_POINT('Ctrl Pts',(7.46515578756604,2.61827616331228,29.4649832388159));
#48002=CARTESIAN_POINT('Ctrl Pts',(7.40066775354943,2.80214264275912,29.4727955013046));
#48003=CARTESIAN_POINT('Ctrl Pts',(7.32939838869323,2.9835804254994,29.4806077637932));
#48004=CARTESIAN_POINT('Ctrl Pts',(7.25157207281655,3.16206000460887,29.4884200262818));
#48005=CARTESIAN_POINT('Ctrl Pts',(7.17371619699191,3.34060737373271,29.4962352560196));
#48006=CARTESIAN_POINT('Ctrl Pts',(7.08929854984644,3.51619397882489,29.5040504857575));
#48007=CARTESIAN_POINT('Ctrl Pts',(6.99859031562769,3.68831324510301,29.5118657154953));
#48008=CARTESIAN_POINT('Ctrl Pts',(6.90778343180112,3.86061969943813,29.5196894446748));
#48009=CARTESIAN_POINT('Ctrl Pts',(6.81067246089798,4.02945097199532,29.5275131738543));
#48010=CARTESIAN_POINT('Ctrl Pts',(6.70757348027875,4.19432700282908,29.5353369030338));
#48011=CARTESIAN_POINT('Ctrl Pts',(6.60441194707415,4.35930306784294,29.5431653790546));
#48012=CARTESIAN_POINT('Ctrl Pts',(6.49525536064069,4.52031881834257,29.5509938550753));
#48013=CARTESIAN_POINT('Ctrl Pts',(6.38046128827864,4.67692577969521,29.558822331096));
#48014=CARTESIAN_POINT('Ctrl Pts',(6.26550922710007,4.83374827611838,29.5666615812937));
#48015=CARTESIAN_POINT('Ctrl Pts',(6.14490440061826,4.98614958906298,29.5745008314915));
#48016=CARTESIAN_POINT('Ctrl Pts',(6.01904331686938,5.13371586179544,29.5823400816893));
#48017=CARTESIAN_POINT('Ctrl Pts',(5.94847764981573,5.21645082767864,29.5867352601108));
#48018=CARTESIAN_POINT('Ctrl Pts',(5.87626036670645,5.29766660895056,29.5911304385324));
#48019=CARTESIAN_POINT('Ctrl Pts',(5.80246602453022,5.37729569897104,29.5955256169539));
#48020=CARTESIAN_POINT('Ctrl Pts',(5.66966033730927,5.52060202451148,29.6034355010117));
#48021=CARTESIAN_POINT('Ctrl Pts',(5.53136325581621,5.65917893213775,29.6113453850695));
#48022=CARTESIAN_POINT('Ctrl Pts',(5.38794440026323,5.79257940296654,29.6192552691272));
#48023=CARTESIAN_POINT('Ctrl Pts',(5.24468146505712,5.92583484511269,29.6271565538146));
#48024=CARTESIAN_POINT('Ctrl Pts',(5.09630809708073,6.05392482701331,29.6350578385019));
#48025=CARTESIAN_POINT('Ctrl Pts',(4.94323315358624,6.1764364312511,29.6429591231892));
#48026=CARTESIAN_POINT('Ctrl Pts',(4.79029618321246,6.29883761043843,29.6508532861042));
#48027=CARTESIAN_POINT('Ctrl Pts',(4.63266634681972,6.41567021398392,29.6587474490191));
#48028=CARTESIAN_POINT('Ctrl Pts',(4.47078842503838,6.5265589600143,29.666641611934));
#48029=CARTESIAN_POINT('Ctrl Pts',(4.30902633946936,6.63736835654359,29.674530125963));
#48030=CARTESIAN_POINT('Ctrl Pts',(4.14302250828464,6.74224217535166,29.6824186399919));
#48031=CARTESIAN_POINT('Ctrl Pts',(3.97325400095765,6.84084597428374,29.6903071540208));
#48032=CARTESIAN_POINT('Ctrl Pts',(3.80357544603444,6.93939752766759,29.6981914882945));
#48033=CARTESIAN_POINT('Ctrl Pts',(3.63013648728671,7.0316855081978,29.7060758225682));
#48034=CARTESIAN_POINT('Ctrl Pts',(3.45344256066231,7.11741915867024,29.7139601568419));
#48035=CARTESIAN_POINT('Ctrl Pts',(3.27680944490404,7.20312330310565,29.7218417776483));
#48036=CARTESIAN_POINT('Ctrl Pts',(3.09692390389205,7.28227746279696,29.7297233984547));
#48037=CARTESIAN_POINT('Ctrl Pts',(2.91431556546067,7.35463702604783,29.7376050192611));
#48038=CARTESIAN_POINT('Ctrl Pts',(2.73170483534119,7.42699753701832,29.745486743296));
#48039=CARTESIAN_POINT('Ctrl Pts',(2.54637155407258,7.49256313870811,29.7533684673308));
#48040=CARTESIAN_POINT('Ctrl Pts',(2.35886543682323,7.5511373216861,29.7612501913657));
#48041=CARTESIAN_POINT('Ctrl Pts',(2.1713480241709,7.60971503318365,29.7691323901971));
#48042=CARTESIAN_POINT('Ctrl Pts',(1.98165784401353,7.66130038323983,29.7770145890284));
#48043=CARTESIAN_POINT('Ctrl Pts',(1.79035991680783,7.70574671062369,29.7848967878598));
#48044=CARTESIAN_POINT('Ctrl Pts',(1.59901827601724,7.75020319446003,29.7927807878563));
#48045=CARTESIAN_POINT('Ctrl Pts',(1.40606849224416,7.78751732682527,29.8006647878529));
#48046=CARTESIAN_POINT('Ctrl Pts',(1.21208616243327,7.81759350022996,29.8085487878495));
#48047=CARTESIAN_POINT('Ctrl Pts',(1.01802686373275,7.8476816073488,29.8164359160831));
#48048=CARTESIAN_POINT('Ctrl Pts',(0.822934543366754,7.87052598017935,29.8243230443168));
#48049=CARTESIAN_POINT('Ctrl Pts',(0.627390552475897,7.88608281053807,29.8322101725505));
#48050=CARTESIAN_POINT('Ctrl Pts',(0.431637938485425,7.90165623825759,29.840105715449));
#48051=CARTESIAN_POINT('Ctrl Pts',(0.235433035532845,7.90992656620909,29.8480012583475));
#48052=CARTESIAN_POINT('Ctrl Pts',(0.0393589541391628,7.91090208969426,
29.855896801246));
#48053=CARTESIAN_POINT('Ctrl Pts',(-0.156834529575379,7.91187820723944,
29.8637971522565));
#48054=CARTESIAN_POINT('Ctrl Pts',(-0.352896688958301,7.90555067515392,
29.871697503267));
#48055=CARTESIAN_POINT('Ctrl Pts',(-0.548248629333389,7.89197975418298,
29.8795978542775));
#48056=CARTESIAN_POINT('Ctrl Pts',(-0.743854926148637,7.87839116330233,
29.8875084918772));
#48057=CARTESIAN_POINT('Ctrl Pts',(-0.938748814827542,7.85754038185277,
29.8954191294769));
#48058=CARTESIAN_POINT('Ctrl Pts',(-1.13235955610086,7.82953912026162,29.9033297670766));
#48059=CARTESIAN_POINT('Ctrl Pts',(-1.21742808270823,7.81723594921315,29.9068055364513));
#48060=CARTESIAN_POINT('Ctrl Pts',(-1.30224905815058,7.80355300658742,29.910281305826));
#48061=CARTESIAN_POINT('Ctrl Pts',(-1.38677495964398,7.78850282219275,29.9137570752007));
#48062=CARTESIAN_POINT('Ctrl Pts',(-1.57913194171663,7.75425287041884,29.9216669406442));
#48063=CARTESIAN_POINT('Ctrl Pts',(-1.77047892991408,7.71282634107011,29.9295768060876));
#48064=CARTESIAN_POINT('Ctrl Pts',(-1.96024003766932,7.664292530607,29.9374866715311));
#48065=CARTESIAN_POINT('Ctrl Pts',(-2.1497949144898,7.61581146632153,29.9453879405926));
#48066=CARTESIAN_POINT('Ctrl Pts',(-2.33776701266895,7.56023859084218,29.9532892096542));
#48067=CARTESIAN_POINT('Ctrl Pts',(-2.52358792335832,7.49769464522796,29.9611904787158));
#48068=CARTESIAN_POINT('Ctrl Pts',(-2.70924141526446,7.43520704973728,29.969084628983));
#48069=CARTESIAN_POINT('Ctrl Pts',(-2.89274725574595,7.36576100509929,29.9769787792503));
#48070=CARTESIAN_POINT('Ctrl Pts',(-3.07354927817775,7.28952781972969,29.9848729295175));
#48071=CARTESIAN_POINT('Ctrl Pts',(-3.25422199054022,7.21334915652943,29.9927614338682));
#48072=CARTESIAN_POINT('Ctrl Pts',(-3.43219442100778,7.13039315718868,30.000649938219));
#48073=CARTESIAN_POINT('Ctrl Pts',(-3.60692730560232,7.04088037194926,30.0085384425697));
#48074=CARTESIAN_POINT('Ctrl Pts',(-3.78156767291515,6.95141498179285,30.0164227701281));
#48075=CARTESIAN_POINT('Ctrl Pts',(-3.95297160594728,6.85539988037804,30.0243070976864));
#48076=CARTESIAN_POINT('Ctrl Pts',(-4.1206212574183,6.75310309805147,30.0321914252448));
#48077=CARTESIAN_POINT('Ctrl Pts',(-4.28821327354627,6.65084148376785,30.040073042294));
#48078=CARTESIAN_POINT('Ctrl Pts',(-4.45205328631158,6.5423026720551,30.0479546593431));
#48079=CARTESIAN_POINT('Ctrl Pts',(-4.61164919190898,6.42779999150295,30.0558362763923));
#48080=CARTESIAN_POINT('Ctrl Pts',(-4.77124727740716,6.3132957469728,30.0637180010955));
#48081=CARTESIAN_POINT('Ctrl Pts',(-4.92660085465792,6.19282766497068,30.0715997257987));
#48082=CARTESIAN_POINT('Ctrl Pts',(-5.07724742815115,6.06675197723893,30.0794814505019));
#48083=CARTESIAN_POINT('Ctrl Pts',(-5.22790312932432,5.94066865057788,30.087363652759));
#48084=CARTESIAN_POINT('Ctrl Pts',(-5.37385099334685,5.80897726222848,30.0952458550161));
#48085=CARTESIAN_POINT('Ctrl Pts',(-5.51466218728181,5.6720738676576,30.1031280572732));
#48086=CARTESIAN_POINT('Ctrl Pts',(-5.65550560731773,5.53513914132613,30.111012063454));
#48087=CARTESIAN_POINT('Ctrl Pts',(-5.79120976731282,5.39299027245297,30.1188960696348));
#48088=CARTESIAN_POINT('Ctrl Pts',(-5.9213830674542,5.24605981365697,30.1267800758155));
#48089=CARTESIAN_POINT('Ctrl Pts',(-6.05160806369479,5.0990710039429,30.1346672129945));
#48090=CARTESIAN_POINT('Ctrl Pts',(-6.17629759474949,4.94729707861559,30.1425543501735));
#48091=CARTESIAN_POINT('Ctrl Pts',(-6.29510052804808,4.79120343356122,30.1504414873524));
#48092=CARTESIAN_POINT('Ctrl Pts',(-6.41403027258995,4.63494317284637,30.1583370433275));
#48093=CARTESIAN_POINT('Ctrl Pts',(-6.52706065970622,4.47435425713783,30.1662325993025));
#48094=CARTESIAN_POINT('Ctrl Pts',(-6.63388343936781,4.30993172949195,30.1741281552776));
#48095=CARTESIAN_POINT('Ctrl Pts',(-6.74077130244694,4.14540902489829,30.1820285217413));
#48096=CARTESIAN_POINT('Ctrl Pts',(-6.84144384140127,3.97704834722757,30.189928888205));
#48097=CARTESIAN_POINT('Ctrl Pts',(-6.93563880299297,3.80536928489447,30.1978292546686));
#48098=CARTESIAN_POINT('Ctrl Pts',(-7.02995645221743,3.63346661296065,30.2057399112502));
#48099=CARTESIAN_POINT('Ctrl Pts',(-7.11777951762511,3.4582372306317,30.2136505678318));
#48100=CARTESIAN_POINT('Ctrl Pts',(-7.19889343844244,3.28022167878185,30.2215612244134));
#48101=CARTESIAN_POINT('Ctrl Pts',(-7.2345331231562,3.2020055343994,30.2250369940914));
#48102=CARTESIAN_POINT('Ctrl Pts',(-7.26887822907425,3.1232517273169,30.2285127637695));
#48103=CARTESIAN_POINT('Ctrl Pts',(-7.301913606672,3.04400701061911,30.2319885334476));
#48104=CARTESIAN_POINT('Ctrl Pts',(-7.38494034361703,2.84484384900301,30.2407240720043));
#48105=CARTESIAN_POINT('Ctrl Pts',(-7.45989208854214,2.642096526646,30.2494596105611));
#48106=CARTESIAN_POINT('Ctrl Pts',(-7.52647707587245,2.43640387176807,30.2581951491179));
#48107=CARTESIAN_POINT('Ctrl Pts',(-7.59279172313769,2.23154634456583,30.2668952207299));
#48108=CARTESIAN_POINT('Ctrl Pts',(-7.65080730516922,2.02376754660903,30.275595292342));
#48109=CARTESIAN_POINT('Ctrl Pts',(-7.70028122495755,1.81372270663579,30.2842953639541));
#48110=CARTESIAN_POINT('Ctrl Pts',(-7.74963017704213,1.60420842541853,30.2929734597863));
#48111=CARTESIAN_POINT('Ctrl Pts',(-7.79048045122216,1.39243973004719,30.3016515556185));
#48112=CARTESIAN_POINT('Ctrl Pts',(-7.82263844849393,1.17908808158871,30.3103296514507));
#48113=CARTESIAN_POINT('Ctrl Pts',(-7.85465833584681,0.966652720877075,
30.3189704772035));
#48114=CARTESIAN_POINT('Ctrl Pts',(-7.87806035896862,0.752648180903682,
30.3276113029563));
#48115=CARTESIAN_POINT('Ctrl Pts',(-7.89270170464743,0.537755336054983,
30.3362521287091));
#48116=CARTESIAN_POINT('Ctrl Pts',(-7.90479793956879,0.360217397177362,
30.3433909163939));
#48117=CARTESIAN_POINT('Ctrl Pts',(-7.91091536010079,0.182073519787902,
30.3505297040786));
#48118=CARTESIAN_POINT('Ctrl Pts',(-7.910999127499,0.00371546903165411,
30.3576684917634));
#48119=CARTESIAN_POINT('',(-7.91099855363492,-0.00392369634145859,32.3576684917634));
#48120=CARTESIAN_POINT('Ctrl Pts',(-7.911,-8.98392471526677E-12,30.3576684917634));
#48121=CARTESIAN_POINT('Ctrl Pts',(-7.9109999999975,-2.20167589667574,30.4462559274961));
#48122=CARTESIAN_POINT('Ctrl Pts',(-6.94214576671874,-4.3861041833947,30.5348433632288));
#48123=CARTESIAN_POINT('Ctrl Pts',(-3.67820201487455,-7.34180684108048,
30.7120182346943));
#48124=CARTESIAN_POINT('Ctrl Pts',(-1.40868175870829,-8.08992666571496,
30.800605670427));
#48125=CARTESIAN_POINT('Ctrl Pts',(2.97309270522138,-7.65454228024921,30.9777805418925));
#48126=CARTESIAN_POINT('Ctrl Pts',(5.05102072676332,-6.47444880833656,31.0663679776252));
#48127=CARTESIAN_POINT('Ctrl Pts',(7.66951518848202,-2.93425195366844,31.2435428490907));
#48128=CARTESIAN_POINT('Ctrl Pts',(8.18956872247139,-0.601881960089965,
31.3321302848234));
#48129=CARTESIAN_POINT('Ctrl Pts',(7.32306689760926,3.71537198233271,31.5093051562888));
#48130=CARTESIAN_POINT('Ctrl Pts',(5.94329958849567,5.66643518937176,31.5978925920216));
#48131=CARTESIAN_POINT('Ctrl Pts',(2.16154501636962,7.92205913233239,31.775067463487));
#48132=CARTESIAN_POINT('Ctrl Pts',(-0.210816529309534,8.20894963712979,
31.8636548992197));
#48133=CARTESIAN_POINT('Ctrl Pts',(-4.42123908577208,6.91982244717338,32.0408297706852));
#48134=CARTESIAN_POINT('Ctrl Pts',(-6.22631625634784,5.35390358802828,32.1294172064179));
#48135=CARTESIAN_POINT('Ctrl Pts',(-7.65317280859749,2.31334857513661,32.2645592586882));
#48136=CARTESIAN_POINT('Ctrl Pts',(-7.91100000000132,1.15702837835623,32.3111138752258));
#48137=CARTESIAN_POINT('Ctrl Pts',(-7.911,-9.0383256434734E-12,32.3576684917634));
#48138=CARTESIAN_POINT('',(-7.91722079586035,-0.00170382440757721,34.3576684917634));
#48139=CARTESIAN_POINT('Ctrl Pts',(-7.91099785005971,-0.00583235378789637,
32.3576684917634));
#48140=CARTESIAN_POINT('Ctrl Pts',(-7.91082541404672,-0.239724359934149,
32.3670578153675));
#48141=CARTESIAN_POINT('Ctrl Pts',(-7.90027652667228,-0.473177135982916,
32.3764471389717));
#48142=CARTESIAN_POINT('Ctrl Pts',(-7.87949087824595,-0.705368343235573,
32.3858364625758));
#48143=CARTESIAN_POINT('Ctrl Pts',(-7.85856304809976,-0.939147826422932,
32.395290012715));
#48144=CARTESIAN_POINT('Ctrl Pts',(-7.82725802231293,-1.17164840009605,
32.4047435628543));
#48145=CARTESIAN_POINT('Ctrl Pts',(-7.78576728881217,-1.40205161262427,
32.4141971129935));
#48146=CARTESIAN_POINT('Ctrl Pts',(-7.74394622875813,-1.63428916965886,
32.4237259271344));
#48147=CARTESIAN_POINT('Ctrl Pts',(-7.69177667750553,-1.86439581611647,
32.4332547412752));
#48148=CARTESIAN_POINT('Ctrl Pts',(-7.62950321232089,-2.0915548601902,32.4427835554161));
#48149=CARTESIAN_POINT('Ctrl Pts',(-7.5928507809301,-2.22525436210524,32.4483919506691));
#48150=CARTESIAN_POINT('Ctrl Pts',(-7.55269908749128,-2.35793316962834,
32.4540003459222));
#48151=CARTESIAN_POINT('Ctrl Pts',(-7.5091056755644,-2.48942823821185,32.4596087411753));
#48152=CARTESIAN_POINT('Ctrl Pts',(-7.44817536530196,-2.67321828750213,
32.4674475692857));
#48153=CARTESIAN_POINT('Ctrl Pts',(-7.38040138015807,-2.8550476425854,32.4752863973962));
#48154=CARTESIAN_POINT('Ctrl Pts',(-7.30592644173637,-3.03436316678432,
32.4831252255067));
#48155=CARTESIAN_POINT('Ctrl Pts',(-7.23153498856715,-3.2134776810579,32.4909552664122));
#48156=CARTESIAN_POINT('Ctrl Pts',(-7.15045767286685,-3.39008365418208,
32.4987853073178));
#48157=CARTESIAN_POINT('Ctrl Pts',(-7.06288723091396,-3.56364209249365,
32.5066153482233));
#48158=CARTESIAN_POINT('Ctrl Pts',(-6.97539791045116,-3.73703975373455,
32.5144381357158));
#48159=CARTESIAN_POINT('Ctrl Pts',(-6.88142759951014,-3.90739519048686,
32.5222609232083));
#48160=CARTESIAN_POINT('Ctrl Pts',(-6.78121752641135,-4.07418824546578,
32.5300837107009));
#48161=CARTESIAN_POINT('Ctrl Pts',(-6.6810807904657,-4.24085923559197,32.5379007732104));
#48162=CARTESIAN_POINT('Ctrl Pts',(-6.5747135677808,-4.40397273637294,32.5457178357199));
#48163=CARTESIAN_POINT('Ctrl Pts',(-6.46240360873286,-4.56303195231379,
32.5535348982294));
#48164=CARTESIAN_POINT('Ctrl Pts',(-6.35015400311001,-4.72200569258928,
32.561347759985));
#48165=CARTESIAN_POINT('Ctrl Pts',(-6.23196822504431,-4.87692920145537,
32.5691606217407));
#48166=CARTESIAN_POINT('Ctrl Pts',(-6.10817814816965,-5.02733335976667,
32.5769734834963));
#48167=CARTESIAN_POINT('Ctrl Pts',(-5.98443052870422,-5.17768593259502,
32.5847836656036));
#48168=CARTESIAN_POINT('Ctrl Pts',(-5.85508266347596,-5.32352197197867,
32.592593847711));
#48169=CARTESIAN_POINT('Ctrl Pts',(-5.72050774440121,-5.46440409800061,
32.6004040298183));
#48170=CARTESIAN_POINT('Ctrl Pts',(-5.58592675591156,-5.6052925778965,32.6082145641698));
#48171=CARTESIAN_POINT('Ctrl Pts',(-5.44611847888516,-5.74122643729883,
32.6160250985214));
#48172=CARTESIAN_POINT('Ctrl Pts',(-5.30149448147925,-5.87180357836032,
32.6238356328729));
#48173=CARTESIAN_POINT('Ctrl Pts',(-5.15685889232388,-6.00239118530252,
32.6316467932461));
#48174=CARTESIAN_POINT('Ctrl Pts',(-5.00740707463034,-6.12762098210182,
32.6394579536193));
#48175=CARTESIAN_POINT('Ctrl Pts',(-4.85358526859605,-6.24712982420466,
32.6472691139925));
#48176=CARTESIAN_POINT('Ctrl Pts',(-4.69972404254289,-6.36666929291978,
32.6550822761371));
#48177=CARTESIAN_POINT('Ctrl Pts',(-4.54149087503321,-6.48048467031655,
32.6628954382817));
#48178=CARTESIAN_POINT('Ctrl Pts',(-4.37936280483853,-6.58825488453481,
32.6707086004263));
#48179=CARTESIAN_POINT('Ctrl Pts',(-4.21716462949364,-6.69607169924025,
32.6785251410291));
#48180=CARTESIAN_POINT('Ctrl Pts',(-4.05106848925646,-6.7978379490441,32.6863416816319));
#48181=CARTESIAN_POINT('Ctrl Pts',(-3.88157806155302,-6.89327735928784,
32.6941582222347));
#48182=CARTESIAN_POINT('Ctrl Pts',(-3.71188983543504,-6.98882814906071,
32.7019838848826));
#48183=CARTESIAN_POINT('Ctrl Pts',(-3.53879971682521,-7.07803717952283,
32.7098095475306));
#48184=CARTESIAN_POINT('Ctrl Pts',(-3.36283450243718,-7.16067490598603,
32.7176352101785));
#48185=CARTESIAN_POINT('Ctrl Pts',(-3.18675458827304,-7.24336649837244,
32.7254659738446));
#48186=CARTESIAN_POINT('Ctrl Pts',(-3.00779616625427,-7.31947811357063,
32.7332967375108));
#48187=CARTESIAN_POINT('Ctrl Pts',(-2.82650347640145,-7.38882934556554,
32.7411275011769));
#48188=CARTESIAN_POINT('Ctrl Pts',(-2.64494883766978,-7.4582807828003,32.7489695794733));
#48189=CARTESIAN_POINT('Ctrl Pts',(-2.46105352628233,-7.52095221383441,
32.7568116577697));
#48190=CARTESIAN_POINT('Ctrl Pts',(-2.2753754692137,-7.5767135008591,32.7646537360662));
#48191=CARTESIAN_POINT('Ctrl Pts',(-2.1713028495594,-7.60796772285804,32.7690492238515));
#48192=CARTESIAN_POINT('Ctrl Pts',(-2.06667033537943,-7.63705197311932,
32.7734447116368));
#48193=CARTESIAN_POINT('Ctrl Pts',(-1.9615771006619,-7.66395043552337,32.7778401994221));
#48194=CARTESIAN_POINT('Ctrl Pts',(-1.7722981957133,-7.7123960992459,32.7857567234205));
#48195=CARTESIAN_POINT('Ctrl Pts',(-1.58095632328446,-7.75389396916855,
32.793673247419));
#48196=CARTESIAN_POINT('Ctrl Pts',(-1.38810369409898,-7.78826611861901,
32.8015897714174));
#48197=CARTESIAN_POINT('Ctrl Pts',(-1.1954732428881,-7.82259866925984,32.8094971750981));
#48198=CARTESIAN_POINT('Ctrl Pts',(-1.00133583748493,-7.8498217908875,32.8174045787787));
#48199=CARTESIAN_POINT('Ctrl Pts',(-0.806258457722267,-7.86980738642003,
32.8253119824594));
#48200=CARTESIAN_POINT('Ctrl Pts',(-0.611369670154704,-7.88977366076148,
32.8332117416114));
#48201=CARTESIAN_POINT('Ctrl Pts',(-0.415543058806255,-7.90251631235472,
32.8411115007634));
#48202=CARTESIAN_POINT('Ctrl Pts',(-0.219355684610209,-7.90795827528378,
32.8490112599154));
#48203=CARTESIAN_POINT('Ctrl Pts',(-0.0233216339860801,-7.91339598523174,
32.8569048452792));
#48204=CARTESIAN_POINT('Ctrl Pts',(0.173072274956343,-7.91154436430064,
32.8647984306431));
#48205=CARTESIAN_POINT('Ctrl Pts',(0.369243681633338,-7.9023781296249,32.8726920160069));
#48206=CARTESIAN_POINT('Ctrl Pts',(0.565298106723887,-7.89321736098874,
32.8805808942416));
#48207=CARTESIAN_POINT('Ctrl Pts',(0.761129950722925,-7.87675068606911,
32.8884697724763));
#48208=CARTESIAN_POINT('Ctrl Pts',(0.956156384946896,-7.85300490051581,
32.8963586507111));
#48209=CARTESIAN_POINT('Ctrl Pts',(1.15110263112005,-7.82926887839927,32.9042442853149));
#48210=CARTESIAN_POINT('Ctrl Pts',(1.34524378597666,-7.79825975198306,32.9121299199187));
#48211=CARTESIAN_POINT('Ctrl Pts',(1.53800139065524,-7.76005623190596,32.9200155545225));
#48212=CARTESIAN_POINT('Ctrl Pts',(1.73074184827965,-7.72185611028274,32.9279004876474));
#48213=CARTESIAN_POINT('Ctrl Pts',(1.92209866181779,-7.67646293069589,32.9357854207723));
#48214=CARTESIAN_POINT('Ctrl Pts',(2.11150230940953,-7.62400675480802,32.9436703538971));
#48215=CARTESIAN_POINT('Ctrl Pts',(2.30090530032556,-7.57155076078938,32.9515552596844));
#48216=CARTESIAN_POINT('Ctrl Pts',(2.48835480642252,-7.51203191072139,32.9594401654716));
#48217=CARTESIAN_POINT('Ctrl Pts',(2.6732951422396,-7.44563053625938,32.9673250712589));
#48218=CARTESIAN_POINT('Ctrl Pts',(2.85826586544687,-7.37921825144368,32.9752112726084));
#48219=CARTESIAN_POINT('Ctrl Pts',(3.04072627246391,-7.30592130542255,32.9830974739578));
#48220=CARTESIAN_POINT('Ctrl Pts',(3.2201391468173,-7.22596878453919,32.9909836753073));
#48221=CARTESIAN_POINT('Ctrl Pts',(3.39961160169132,-7.14598971253548,32.9988724955545));
#48222=CARTESIAN_POINT('Ctrl Pts',(3.57603419278762,-7.0593508020727,33.0067613158018));
#48223=CARTESIAN_POINT('Ctrl Pts',(3.7488926380972,-6.9663279414639,33.014650136049));
#48224=CARTESIAN_POINT('Ctrl Pts',(3.92191839442842,-6.87321504331127,33.0225465919462));
#48225=CARTESIAN_POINT('Ctrl Pts',(4.09137281065589,-6.77370601614417,33.0304430478434));
#48226=CARTESIAN_POINT('Ctrl Pts',(4.25676811904696,-6.6681216381126,33.0383395037406));
#48227=CARTESIAN_POINT('Ctrl Pts',(4.42225484159113,-6.56247890348921,33.0462403240168));
#48228=CARTESIAN_POINT('Ctrl Pts',(4.58367770042664,-6.45075431881464,33.0541411442931));
#48229=CARTESIAN_POINT('Ctrl Pts',(4.74058034280286,-6.33331027294819,33.0620419645694));
#48230=CARTESIAN_POINT('Ctrl Pts',(4.89767364313631,-6.21572351666251,33.0699523854122));
#48231=CARTESIAN_POINT('Ctrl Pts',(5.0502354880613,-6.09240363288114,33.077862806255));
#48232=CARTESIAN_POINT('Ctrl Pts',(5.1978440257412,-5.96375204750051,33.0857732270978));
#48233=CARTESIAN_POINT('Ctrl Pts',(5.26190030067285,-5.90792234108201,33.0892060372882));
#48234=CARTESIAN_POINT('Ctrl Pts',(5.32502424256473,-5.85108901776739,33.0926388474785));
#48235=CARTESIAN_POINT('Ctrl Pts',(5.38718366354049,-5.79328690600444,33.0960716576689));
#48236=CARTESIAN_POINT('Ctrl Pts',(5.53774013787773,-5.65328428018089,33.1043862750063));
#48237=CARTESIAN_POINT('Ctrl Pts',(5.68296554276837,-5.5072890821744,33.1127008923437));
#48238=CARTESIAN_POINT('Ctrl Pts',(5.82238320800562,-5.35572355327776,33.1210155096811));
#48239=CARTESIAN_POINT('Ctrl Pts',(5.9616285599979,-5.20434535177658,33.1293198505683));
#48240=CARTESIAN_POINT('Ctrl Pts',(6.09508029100375,-5.04741076523861,33.1376241914556));
#48241=CARTESIAN_POINT('Ctrl Pts',(6.22229735421852,-4.88537988652727,33.1459285323428));
#48242=CARTESIAN_POINT('Ctrl Pts',(6.34936559297583,-4.72353855909943,33.1542231584245));
#48243=CARTESIAN_POINT('Ctrl Pts',(6.47021353080071,-4.55661306047075,33.1625177845062));
#48244=CARTESIAN_POINT('Ctrl Pts',(6.58443876735422,-4.3850983020866,33.1708124105879));
#48245=CARTESIAN_POINT('Ctrl Pts',(6.69849201555532,-4.21384179259385,33.1790945474937));
#48246=CARTESIAN_POINT('Ctrl Pts',(6.8059423005254,-4.03801005667824,33.1873766843994));
#48247=CARTESIAN_POINT('Ctrl Pts',(6.90642905759138,-3.85812890822189,33.1956588213052));
#48248=CARTESIAN_POINT('Ctrl Pts',(7.00682314625146,-3.67841364529878,33.203933320464));
#48249=CARTESIAN_POINT('Ctrl Pts',(7.10026637039486,-3.49465667183419,33.2122078196228));
#48250=CARTESIAN_POINT('Ctrl Pts',(7.18644187709675,-3.30741200141593,33.2204823187816));
#48251=CARTESIAN_POINT('Ctrl Pts',(7.27251826832934,-3.12038269199865,33.228747300957));
#48252=CARTESIAN_POINT('Ctrl Pts',(7.35134349972627,-2.92987395591469,33.2370122831324));
#48253=CARTESIAN_POINT('Ctrl Pts',(7.4226468798375,-2.73646383079307,33.2452772653078));
#48254=CARTESIAN_POINT('Ctrl Pts',(7.45114563696957,-2.65916106935138,33.248580639136));
#48255=CARTESIAN_POINT('Ctrl Pts',(7.47844332087114,-2.58139509025245,33.2518840129641));
#48256=CARTESIAN_POINT('Ctrl Pts',(7.50452474429773,-2.50320381955268,33.2551873867923));
#48257=CARTESIAN_POINT('Ctrl Pts',(7.56978874149768,-2.30754444971906,33.2634534762899));
#48258=CARTESIAN_POINT('Ctrl Pts',(7.62735976619017,-2.10944218308649,33.2717195657876));
#48259=CARTESIAN_POINT('Ctrl Pts',(7.67708674047127,-1.90951831079991,33.2799856552852));
#48260=CARTESIAN_POINT('Ctrl Pts',(7.72685843428924,-1.70941464669802,33.2882591784886));
#48261=CARTESIAN_POINT('Ctrl Pts',(7.76877192402986,-1.50748639153828,33.296532701692));
#48262=CARTESIAN_POINT('Ctrl Pts',(7.80272734130214,-1.30436461056564,33.3048062248954));
#48263=CARTESIAN_POINT('Ctrl Pts',(7.83671550331287,-1.10104695010966,33.3130877266299));
#48264=CARTESIAN_POINT('Ctrl Pts',(7.8627302231974,-0.896533755392057,33.3213692283644));
#48265=CARTESIAN_POINT('Ctrl Pts',(7.88072343325758,-0.691461617521098,
33.3296507300989));
#48266=CARTESIAN_POINT('Ctrl Pts',(7.89874660162455,-0.486048038962156,
33.3379460203553));
#48267=CARTESIAN_POINT('Ctrl Pts',(7.90872153303988,-0.280073949757042,
33.3462413106116));
#48268=CARTESIAN_POINT('Ctrl Pts',(7.91065222120185,-0.0741784011299107,
33.354536600868));
#48269=CARTESIAN_POINT('Ctrl Pts',(7.91258466031614,0.131903875366846,33.3628394141713));
#48270=CARTESIAN_POINT('Ctrl Pts',(7.9064582978321,0.33790717583952,33.3711422274745));
#48271=CARTESIAN_POINT('Ctrl Pts',(7.89232914057703,0.54319585491661,33.3794450407778));
#48272=CARTESIAN_POINT('Ctrl Pts',(7.87817831598618,0.748799348151595,33.3877605866058));
#48273=CARTESIAN_POINT('Ctrl Pts',(7.85600019236455,0.953685737009395,33.3960761324338));
#48274=CARTESIAN_POINT('Ctrl Pts',(7.82590244114712,1.15722598555663,33.4043916782618));
#48275=CARTESIAN_POINT('Ctrl Pts',(7.81394443739188,1.23809365699453,33.4076954908131));
#48276=CARTESIAN_POINT('Ctrl Pts',(7.80073687067036,1.31874896723893,33.4109993033644));
#48277=CARTESIAN_POINT('Ctrl Pts',(7.78628870373272,1.39915303742095,33.4143031159157));
#48278=CARTESIAN_POINT('Ctrl Pts',(7.75169814839391,1.59164952857453,33.4222128190205));
#48279=CARTESIAN_POINT('Ctrl Pts',(7.70992103064171,1.78310643945418,33.4301225221252));
#48280=CARTESIAN_POINT('Ctrl Pts',(7.66103118836468,1.97294757429174,33.43803222523));
#48281=CARTESIAN_POINT('Ctrl Pts',(7.61219094721578,2.1625961060442,33.4459339035554));
#48282=CARTESIAN_POINT('Ctrl Pts',(7.55625244095167,2.3506317960854,33.4538355818808));
#48283=CARTESIAN_POINT('Ctrl Pts',(7.49334089691572,2.53648638920267,33.4617372602062));
#48284=CARTESIAN_POINT('Ctrl Pts',(7.43048152520646,2.72218685374625,33.469632385697));
#48285=CARTESIAN_POINT('Ctrl Pts',(7.36066074571401,2.9057095001494,33.4775275111878));
#48286=CARTESIAN_POINT('Ctrl Pts',(7.28405425401273,3.08649876471692,33.4854226366786));
#48287=CARTESIAN_POINT('Ctrl Pts',(7.20749710416343,3.26717158383793,33.4933126769592));
#48288=CARTESIAN_POINT('Ctrl Pts',(7.12416308422304,3.44511421271346,33.5012027172398));
#48289=CARTESIAN_POINT('Ctrl Pts',(7.03427699053538,3.6197884220524,33.5090927575204));
#48290=CARTESIAN_POINT('Ctrl Pts',(6.94443214826451,3.79438246817234,33.5169791768256));
#48291=CARTESIAN_POINT('Ctrl Pts',(6.8480413815963,3.96571077798305,33.5248655961307));
#48292=CARTESIAN_POINT('Ctrl Pts',(6.74537678638158,4.13325694939771,33.5327520154358));
#48293=CARTESIAN_POINT('Ctrl Pts',(6.64274029988734,4.30075724805079,33.5406362755043));
#48294=CARTESIAN_POINT('Ctrl Pts',(6.53383358841617,4.46447717872594,33.5485205355728));
#48295=CARTESIAN_POINT('Ctrl Pts',(6.41897382861698,4.62392646865522,33.5564047956413));
#48296=CARTESIAN_POINT('Ctrl Pts',(6.30410065900207,4.78339437420407,33.5642899761929));
#48297=CARTESIAN_POINT('Ctrl Pts',(6.18327324819839,4.9385903590711,33.5721751567445));
#48298=CARTESIAN_POINT('Ctrl Pts',(6.05685146349842,5.08905407213531,33.5800603372962));
#48299=CARTESIAN_POINT('Ctrl Pts',(5.93041391027072,5.2395365524653,33.5879465013626));
#48300=CARTESIAN_POINT('Ctrl Pts',(5.79838081400447,5.38528532036431,33.595832665429));
#48301=CARTESIAN_POINT('Ctrl Pts',(5.66115158322437,5.52587402604839,33.6037188294953));
#48302=CARTESIAN_POINT('Ctrl Pts',(5.52388221122846,5.66650385563546,33.6116073003605));
#48303=CARTESIAN_POINT('Ctrl Pts',(5.38141391657862,5.80197036847344,33.6194957712256));
#48304=CARTESIAN_POINT('Ctrl Pts',(5.23418229322077,5.93188475287022,33.6273842420907));
#48305=CARTESIAN_POINT('Ctrl Pts',(5.08688289936547,6.06185893666509,33.6352763440072));
#48306=CARTESIAN_POINT('Ctrl Pts',(4.9348160658088,6.186275671494,33.6431684459237));
#48307=CARTESIAN_POINT('Ctrl Pts',(4.77844989257998,6.30478688173537,33.6510605478402));
#48308=CARTESIAN_POINT('Ctrl Pts',(4.62190244378021,6.42343548222463,33.6589617990839));
#48309=CARTESIAN_POINT('Ctrl Pts',(4.46104597428791,6.53616467480275,33.6668630503276));
#48310=CARTESIAN_POINT('Ctrl Pts',(4.29637791989264,6.64266947615633,33.6747643015714));
#48311=CARTESIAN_POINT('Ctrl Pts',(4.13160075162838,6.7492448507063,33.6826707884152));
#48312=CARTESIAN_POINT('Ctrl Pts',(3.96300725859472,6.84958743595584,33.6905772752591));
#48313=CARTESIAN_POINT('Ctrl Pts',(3.79111903307485,6.94343844770425,33.698483762103));
#48314=CARTESIAN_POINT('Ctrl Pts',(3.61899400299996,7.03741875479565,33.7064011414445));
#48315=CARTESIAN_POINT('Ctrl Pts',(3.44356548136039,7.12488947176204,33.7143185207861));
#48316=CARTESIAN_POINT('Ctrl Pts',(3.26537564802098,7.20563965774806,33.7222359001277));
#48317=CARTESIAN_POINT('Ctrl Pts',(3.18811443439959,7.24065207822409,33.7256687914726));
#48318=CARTESIAN_POINT('Ctrl Pts',(3.11033430007697,7.27440167281522,33.7291016828176));
#48319=CARTESIAN_POINT('Ctrl Pts',(3.0320802757189,7.30687417447409,33.7325345741626));
#48320=CARTESIAN_POINT('Ctrl Pts',(2.8533275037777,7.38104990832296,33.7403762008229));
#48321=CARTESIAN_POINT('Ctrl Pts',(2.67156962090182,7.44877910061264,33.7482178274832));
#48322=CARTESIAN_POINT('Ctrl Pts',(2.48731673635885,7.50980535387098,33.7560594541435));
#48323=CARTESIAN_POINT('Ctrl Pts',(2.30328079570511,7.57075975331405,33.7638918478793));
#48324=CARTESIAN_POINT('Ctrl Pts',(2.11675603282264,7.62502681902685,33.771724241615));
#48325=CARTESIAN_POINT('Ctrl Pts',(1.92827486361654,7.67239708633127,33.7795566353508));
#48326=CARTESIAN_POINT('Ctrl Pts',(1.7399789255388,7.719720800189,33.7873813317492));
#48327=CARTESIAN_POINT('Ctrl Pts',(1.54973074833863,7.76016112808362,33.7952060281477));
#48328=CARTESIAN_POINT('Ctrl Pts',(1.35808052161118,7.79355748659239,33.8030307245462));
#48329=CARTESIAN_POINT('Ctrl Pts',(1.16658135471028,7.82692752189659,33.8108492534733));
#48330=CARTESIAN_POINT('Ctrl Pts',(0.973682683985094,7.8532645856887,33.8186677824005));
#48331=CARTESIAN_POINT('Ctrl Pts',(0.779947771138422,7.87245847714018,33.8264863113276));
#48332=CARTESIAN_POINT('Ctrl Pts',(0.586327885542514,7.89164097250133,33.8343001981183));
#48333=CARTESIAN_POINT('Ctrl Pts',(0.391873095806411,7.90368870919852,33.8421140849091));
#48334=CARTESIAN_POINT('Ctrl Pts',(0.197154910023527,7.90854290887099,33.8499279716999));
#48335=CARTESIAN_POINT('Ctrl Pts',(0.00251447890120057,7.91339517016957,
33.8577387382576));
#48336=CARTESIAN_POINT('Ctrl Pts',(-0.192388787611445,7.91105960878699,
33.8655495048153));
#48337=CARTESIAN_POINT('Ctrl Pts',(-0.386980039243796,7.90152943734483,
33.873360271373));
#48338=CARTESIAN_POINT('Ctrl Pts',(-0.581563556820466,7.89199964468062,
33.8811707274908));
#48339=CARTESIAN_POINT('Ctrl Pts',(-0.775834732537457,7.87527581978102,
33.8889811836085));
#48340=CARTESIAN_POINT('Ctrl Pts',(-0.969220026476353,7.85140328478147,
33.8967916397262));
#48341=CARTESIAN_POINT('Ctrl Pts',(-1.16261065360724,7.82753009142361,33.9046023112412));
#48342=CARTESIAN_POINT('Ctrl Pts',(-1.35511500086208,7.79650783757462,33.9124129827562));
#48343=CARTESIAN_POINT('Ctrl Pts',(-1.54616598484776,7.75843358850869,33.9202236542712));
#48344=CARTESIAN_POINT('Ctrl Pts',(-1.73725588444708,7.72035158401153,33.9280359167599));
#48345=CARTESIAN_POINT('Ctrl Pts',(-1.92689148591203,7.67521479159519,33.9358481792485));
#48346=CARTESIAN_POINT('Ctrl Pts',(-2.11451706105623,7.62317116418765,33.9436604417371));
#48347=CARTESIAN_POINT('Ctrl Pts',(-2.30221390004129,7.5711077695987,33.9514756714749));
#48348=CARTESIAN_POINT('Ctrl Pts',(-2.48789885315812,7.51213240844658,33.9592909012126));
#48349=CARTESIAN_POINT('Ctrl Pts',(-2.67103233821561,7.44644259013701,33.9671061309504));
#48350=CARTESIAN_POINT('Ctrl Pts',(-2.85436498982844,7.38068133096108,33.9749298601299));
#48351=CARTESIAN_POINT('Ctrl Pts',(-3.0351402999016,7.30819114865378,33.9827535893095));
#48352=CARTESIAN_POINT('Ctrl Pts',(-3.21283864744986,7.22921771877515,33.990577318489));
#48353=CARTESIAN_POINT('Ctrl Pts',(-3.39064480878037,7.15019637385234,33.9984057945097));
#48354=CARTESIAN_POINT('Ctrl Pts',(-3.5653699720372,7.0646840963973,34.0062342705304));
#48355=CARTESIAN_POINT('Ctrl Pts',(-3.73651997483667,6.97297206918589,34.0140627465511));
#48356=CARTESIAN_POINT('Ctrl Pts',(-3.90790552800753,6.88113382052127,34.0219019967488));
#48357=CARTESIAN_POINT('Ctrl Pts',(-4.07570579018091,6.78307895642799,34.0297412469466));
#48358=CARTESIAN_POINT('Ctrl Pts',(-4.23945541750854,6.67914206788248,34.0375804971443));
#48359=CARTESIAN_POINT('Ctrl Pts',(-4.33126379336439,6.62086848836599,34.041975675566));
#48360=CARTESIAN_POINT('Ctrl Pts',(-4.42179945894131,6.5607466756324,34.0463708539876));
#48361=CARTESIAN_POINT('Ctrl Pts',(-4.51098512448502,6.49884098948996,34.0507660324093));
#48362=CARTESIAN_POINT('Ctrl Pts',(-4.6706035382721,6.38804641991181,34.0586322226059));
#48363=CARTESIAN_POINT('Ctrl Pts',(-4.8263653571498,6.27120966955334,34.0664984128024));
#48364=CARTESIAN_POINT('Ctrl Pts',(-4.9777792821485,6.14862866159708,34.074364602999));
#48365=CARTESIAN_POINT('Ctrl Pts',(-5.12902791675357,6.02618146869817,34.0822222061011));
#48366=CARTESIAN_POINT('Ctrl Pts',(-5.27593784087924,5.89800272393123,34.0900798092033));
#48367=CARTESIAN_POINT('Ctrl Pts',(-5.41804577754358,5.76443413983039,34.0979374123054));
#48368=CARTESIAN_POINT('Ctrl Pts',(-5.56002581550766,5.63098576891893,34.1057879434786));
#48369=CARTESIAN_POINT('Ctrl Pts',(-5.69721222110953,5.49215745811834,34.1136384746519));
#48370=CARTESIAN_POINT('Ctrl Pts',(-5.82917376449969,5.34833191035004,34.1214890058251));
#48371=CARTESIAN_POINT('Ctrl Pts',(-5.96104181941303,5.20460825614136,34.1293339752704));
#48372=CARTESIAN_POINT('Ctrl Pts',(-6.0876921504874,5.05589467364254,34.1371789447157));
#48373=CARTESIAN_POINT('Ctrl Pts',(-6.20872931340659,4.9026116828529,34.145023914161));
#48374=CARTESIAN_POINT('Ctrl Pts',(-6.32970390662075,4.74940793112742,34.1528648281789));
#48375=CARTESIAN_POINT('Ctrl Pts',(-6.44507089687165,4.59163975082454,34.1607057421968));
#48376=CARTESIAN_POINT('Ctrl Pts',(-6.55447404215888,4.4297619609484,34.1685466562148));
#48377=CARTESIAN_POINT('Ctrl Pts',(-6.66442361566216,4.26707565142955,34.176426732696));
#48378=CARTESIAN_POINT('Ctrl Pts',(-6.76834937075488,4.10023883530814,34.1843068091772));
#48379=CARTESIAN_POINT('Ctrl Pts',(-6.86593240988546,3.92974466637266,34.1921868856584));
#48380=CARTESIAN_POINT('Ctrl Pts',(-6.96300230492519,3.76014704745341,34.2000255244602));
#48381=CARTESIAN_POINT('Ctrl Pts',(-7.05379587419109,3.58693076493575,34.2078641632621));
#48382=CARTESIAN_POINT('Ctrl Pts',(-7.13804420136761,3.41060786067854,34.215702802064));
#48383=CARTESIAN_POINT('Ctrl Pts',(-7.22229999029257,3.23426933976521,34.2235421351224));
#48384=CARTESIAN_POINT('Ctrl Pts',(-7.30000923125475,3.05482396421545,34.2313814681808));
#48385=CARTESIAN_POINT('Ctrl Pts',(-7.37095025389119,2.87280583309443,34.2392208012392));
#48386=CARTESIAN_POINT('Ctrl Pts',(-7.44190986601797,2.69074000567355,34.247062188528));
#48387=CARTESIAN_POINT('Ctrl Pts',(-7.50609759982208,2.50610040520851,34.2549035758168));
#48388=CARTESIAN_POINT('Ctrl Pts',(-7.56334089624944,2.31943861464809,34.2627449631057));
#48389=CARTESIAN_POINT('Ctrl Pts',(-7.62108722234317,2.13113651991079,34.2706552571605));
#48390=CARTESIAN_POINT('Ctrl Pts',(-7.67176637387579,1.94077687265887,34.2785655512153));
#48391=CARTESIAN_POINT('Ctrl Pts',(-7.71525345212281,1.74893829779871,34.2864758452701));
#48392=CARTESIAN_POINT('Ctrl Pts',(-7.75842621094329,1.55848630932855,34.2943289646608));
#48393=CARTESIAN_POINT('Ctrl Pts',(-7.79451051461208,1.36657705616842,34.3021820840515));
#48394=CARTESIAN_POINT('Ctrl Pts',(-7.823436143118,1.17378358931916,34.3100352034423));
#48395=CARTESIAN_POINT('Ctrl Pts',(-7.85267766133815,0.978884672172183,
34.3179740848291));
#48396=CARTESIAN_POINT('Ctrl Pts',(-7.87460319983354,0.783082483421094,
34.325912966216));
#48397=CARTESIAN_POINT('Ctrl Pts',(-7.88919428051167,0.586970701434065,
34.3338518476028));
#48398=CARTESIAN_POINT('Ctrl Pts',(-7.9037853611898,0.390858919447036,34.3417907289897));
#48399=CARTESIAN_POINT('Ctrl Pts',(-7.91104202717494,0.194437909010654,
34.3497296103765));
#48400=CARTESIAN_POINT('Ctrl Pts',(-7.91099981680841,-0.00170248562263939,
34.3576684917634));
#48401=CARTESIAN_POINT('',(-7.91065253198049,0.0049220711787074,36.3576684917634));
#48402=CARTESIAN_POINT('Ctrl Pts',(-7.92256293040024,-0.00170497406090317,
34.3576684917634));
#48403=CARTESIAN_POINT('Ctrl Pts',(-7.92283402357086,-0.0951406271396644,
34.3614448247277));
#48404=CARTESIAN_POINT('Ctrl Pts',(-7.92132116720036,-0.188567197001396,
34.3652211576919));
#48405=CARTESIAN_POINT('Ctrl Pts',(-7.824618403598,-2.90446889716205,34.4750746434051));
#48406=CARTESIAN_POINT('Ctrl Pts',(-4.77929028327528,-8.04776548189143,
34.6872289489031));
#48407=CARTESIAN_POINT('Ctrl Pts',(4.19818763349781,-8.36643474264993,35.0054604071498));
#48408=CARTESIAN_POINT('Ctrl Pts',(8.44002877177934,-2.22556932755547,35.2706532890221));
#48409=CARTESIAN_POINT('Ctrl Pts',(7.59677957168971,3.15057924978888,35.48280759452));
#48410=CARTESIAN_POINT('Ctrl Pts',(4.38769321310667,7.54555450367134,35.694961900018));
#48411=CARTESIAN_POINT('Ctrl Pts',(-2.95515982338205,8.8819502434627,35.9601547818902));
#48412=CARTESIAN_POINT('Ctrl Pts',(-7.54111000579349,3.94981135115549,36.1987365045968));
#48413=CARTESIAN_POINT('Ctrl Pts',(-7.91666636458249,0.66324315570486,36.3312410745546));
#48414=CARTESIAN_POINT('Ctrl Pts',(-7.91054183245,0.0064901895060634,36.3576684917634));
#48415=CARTESIAN_POINT('',(-7.911,-9.20097331658098E-12,38.3576684917634));
#48416=CARTESIAN_POINT('Ctrl Pts',(-7.911,-9.14712749988666E-12,36.3576684917634));
#48417=CARTESIAN_POINT('Ctrl Pts',(-7.91099999999745,-2.20167589667591,
36.4462559274961));
#48418=CARTESIAN_POINT('Ctrl Pts',(-6.94214576671865,-4.38610418339484,
36.5348433632289));
#48419=CARTESIAN_POINT('Ctrl Pts',(-3.6782020148744,-7.34180684108056,36.7120182346943));
#48420=CARTESIAN_POINT('Ctrl Pts',(-1.40868175870812,-8.08992666571498,
36.800605670427));
#48421=CARTESIAN_POINT('Ctrl Pts',(2.97309270522153,-7.65454228024915,36.9777805418925));
#48422=CARTESIAN_POINT('Ctrl Pts',(5.05102072676346,-6.47444880833645,37.0663679776252));
#48423=CARTESIAN_POINT('Ctrl Pts',(7.66951518848208,-2.93425195366828,37.2435428490907));
#48424=CARTESIAN_POINT('Ctrl Pts',(8.1895687224714,-0.601881960089796,37.3321302848234));
#48425=CARTESIAN_POINT('Ctrl Pts',(7.32306689760918,3.71537198233286,37.5093051562888));
#48426=CARTESIAN_POINT('Ctrl Pts',(5.94329958849555,5.66643518937189,37.5978925920216));
#48427=CARTESIAN_POINT('Ctrl Pts',(2.16154501636946,7.92205913233244,37.775067463487));
#48428=CARTESIAN_POINT('Ctrl Pts',(-0.210816529309703,8.20894963712978,
37.8636548992197));
#48429=CARTESIAN_POINT('Ctrl Pts',(-4.42123908577222,6.91982244717329,38.0408297706852));
#48430=CARTESIAN_POINT('Ctrl Pts',(-6.22631625634795,5.35390358802815,38.1294172064179));
#48431=CARTESIAN_POINT('Ctrl Pts',(-7.65317280859754,2.31334857513645,38.2645592586882));
#48432=CARTESIAN_POINT('Ctrl Pts',(-7.91100000000134,1.15702837835607,38.3111138752258));
#48433=CARTESIAN_POINT('Ctrl Pts',(-7.911,-9.20097331658098E-12,38.3576684917634));
#48434=CARTESIAN_POINT('',(-7.911,-9.14324171930048E-12,40.3576684917634));
#48435=CARTESIAN_POINT('Ctrl Pts',(-7.911,-9.20097331658098E-12,38.3576684917634));
#48436=CARTESIAN_POINT('Ctrl Pts',(-7.91099999999744,-2.20167589667592,
38.4462559274961));
#48437=CARTESIAN_POINT('Ctrl Pts',(-6.94214576671865,-4.38610418339481,
38.5348433632289));
#48438=CARTESIAN_POINT('Ctrl Pts',(-3.67820201487448,-7.3418068410805,38.7120182346943));
#48439=CARTESIAN_POINT('Ctrl Pts',(-1.40868175870826,-8.08992666571495,
38.800605670427));
#48440=CARTESIAN_POINT('Ctrl Pts',(2.97309270522133,-7.65454228024922,38.9777805418925));
#48441=CARTESIAN_POINT('Ctrl Pts',(5.05102072676325,-6.4744488083366,39.0663679776252));
#48442=CARTESIAN_POINT('Ctrl Pts',(7.66951518848195,-2.93425195366858,39.2435428490906));
#48443=CARTESIAN_POINT('Ctrl Pts',(8.18956872247136,-0.601881960090168,
39.3321302848234));
#48444=CARTESIAN_POINT('Ctrl Pts',(7.32306689760937,3.71537198233245,39.5093051562888));
#48445=CARTESIAN_POINT('Ctrl Pts',(5.94329958849588,5.66643518937152,39.5978925920215));
#48446=CARTESIAN_POINT('Ctrl Pts',(2.16154501637,7.92205913233228,39.775067463487));
#48447=CARTESIAN_POINT('Ctrl Pts',(-0.210816529309095,8.20894963712979,
39.8636548992197));
#48448=CARTESIAN_POINT('Ctrl Pts',(-4.42123908577165,6.91982244717365,40.0408297706852));
#48449=CARTESIAN_POINT('Ctrl Pts',(-6.22631625634747,5.35390358802869,40.1294172064179));
#48450=CARTESIAN_POINT('Ctrl Pts',(-7.65317280859742,2.31334857513695,40.2645592586882));
#48451=CARTESIAN_POINT('Ctrl Pts',(-7.91100000000134,1.15702837835635,40.3111138752258));
#48452=CARTESIAN_POINT('Ctrl Pts',(-7.911,-9.14324171930048E-12,40.3576684917634));
#48453=CARTESIAN_POINT('',(-7.91099967169525,0.00226142970142933,42.3575775000139));
#48454=CARTESIAN_POINT('Ctrl Pts',(-7.911,-9.14324171930048E-12,40.3576684917634));
#48455=CARTESIAN_POINT('Ctrl Pts',(-7.91099999999746,-2.2016758966759,40.4462559274961));
#48456=CARTESIAN_POINT('Ctrl Pts',(-6.94214576671865,-4.38610418339484,
40.5348433632289));
#48457=CARTESIAN_POINT('Ctrl Pts',(-3.6782020148744,-7.34180684108056,40.7120182346943));
#48458=CARTESIAN_POINT('Ctrl Pts',(-1.40868175870813,-8.08992666571498,
40.800605670427));
#48459=CARTESIAN_POINT('Ctrl Pts',(2.97309270522157,-7.65454228024915,40.9777805418925));
#48460=CARTESIAN_POINT('Ctrl Pts',(5.05102072676352,-6.47444880833642,41.0663679776252));
#48461=CARTESIAN_POINT('Ctrl Pts',(7.66951518848214,-2.93425195366815,41.2435428490907));
#48462=CARTESIAN_POINT('Ctrl Pts',(8.18956872247142,-0.601881960089605,
41.3321302848234));
#48463=CARTESIAN_POINT('Ctrl Pts',(7.32306689760907,3.7153719823331,41.5093051562888));
#48464=CARTESIAN_POINT('Ctrl Pts',(5.94329958849534,5.66643518937212,41.5978925920216));
#48465=CARTESIAN_POINT('Ctrl Pts',(2.16154501636909,7.92205913233254,41.775067463487));
#48466=CARTESIAN_POINT('Ctrl Pts',(-0.210816529310129,8.20894963712978,
41.8636548992198));
#48467=CARTESIAN_POINT('Ctrl Pts',(-4.42123908577265,6.91982244717303,42.0408297706852));
#48468=CARTESIAN_POINT('Ctrl Pts',(-6.22631625634831,5.35390358802774,42.1294172064179));
#48469=CARTESIAN_POINT('Ctrl Pts',(-7.65285257229365,2.31403098157547,42.2645289281051));
#48470=CARTESIAN_POINT('Ctrl Pts',(-7.91066394919783,1.15853502979653,42.3110532140595));
#48471=CARTESIAN_POINT('Ctrl Pts',(-7.91099967169525,0.00226142970142933,
42.3575775000139));
#48472=CARTESIAN_POINT('',(-7.91099966078395,0.00163815081257414,44.3576684917634));
#48473=CARTESIAN_POINT('Ctrl Pts',(-7.91099967460919,0.00226899390551966,
42.3577662811419));
#48474=CARTESIAN_POINT('Ctrl Pts',(-7.91105523449881,-0.19144429357958,
42.3655880831917));
#48475=CARTESIAN_POINT('Ctrl Pts',(-7.9039914899811,-0.38540394722232,42.3734098852415));
#48476=CARTESIAN_POINT('Ctrl Pts',(-7.88978036946687,-0.579039481879457,
42.3812316872913));
#48477=CARTESIAN_POINT('Ctrl Pts',(-7.87558204539206,-0.772500656929422,
42.3890464461796));
#48478=CARTESIAN_POINT('Ctrl Pts',(-7.8542491874259,-0.965637944728926,
42.3968612050679));
#48479=CARTESIAN_POINT('Ctrl Pts',(-7.82580574136786,-1.15787974262179,
42.4046759639563));
#48480=CARTESIAN_POINT('Ctrl Pts',(-7.79738233777216,-1.34998607876402,
42.412485216233));
#48481=CARTESIAN_POINT('Ctrl Pts',(-7.76185837669972,-1.54119783421374,
42.4202944685097));
#48482=CARTESIAN_POINT('Ctrl Pts',(-7.71930972670178,-1.73094723872432,
42.4281037207864));
#48483=CARTESIAN_POINT('Ctrl Pts',(-7.67678273016845,-1.92060007772652,
42.4359089988509));
#48484=CARTESIAN_POINT('Ctrl Pts',(-7.62723824307516,-2.10879170477572,
42.4437142769153));
#48485=CARTESIAN_POINT('Ctrl Pts',(-7.57080348232179,-2.29496310037094,
42.4515195549797));
#48486=CARTESIAN_POINT('Ctrl Pts',(-7.51311269925965,-2.48527796043738,
42.4594985487336));
#48487=CARTESIAN_POINT('Ctrl Pts',(-7.44822142064704,-2.67348124129677,
42.4674775424875));
#48488=CARTESIAN_POINT('Ctrl Pts',(-7.37632005783899,-2.85898992728588,
42.4754565362414));
#48489=CARTESIAN_POINT('Ctrl Pts',(-7.30600106045762,-3.04041604071181,
42.4832599327137));
#48490=CARTESIAN_POINT('Ctrl Pts',(-7.22897744319996,-3.21926458296378,
42.4910633291859));
#48491=CARTESIAN_POINT('Ctrl Pts',(-7.1454767238172,-3.39500859930968,42.4988667256582));
#48492=CARTESIAN_POINT('Ctrl Pts',(-7.06196661380801,-3.57077238011288,
42.5066709997131));
#48493=CARTESIAN_POINT('Ctrl Pts',(-6.97197810182106,-3.74343062041715,
42.514475273768));
#48494=CARTESIAN_POINT('Ctrl Pts',(-6.87578554007716,-3.91247929155744,
42.5222795478228));
#48495=CARTESIAN_POINT('Ctrl Pts',(-6.77956510754424,-4.08157694278271,
42.5300860830845));
#48496=CARTESIAN_POINT('Ctrl Pts',(-6.67713721925833,-4.24706263493058,
42.5378926183462));
#48497=CARTESIAN_POINT('Ctrl Pts',(-6.56882064692729,-4.40845962990495,
42.5456991536079));
#48498=CARTESIAN_POINT('Ctrl Pts',(-6.45629780081742,-4.57612417871097,
42.5538088412301));
#48499=CARTESIAN_POINT('Ctrl Pts',(-6.3374200012213,-4.73937577021939,42.5619185288522));
#48500=CARTESIAN_POINT('Ctrl Pts',(-6.21259151317871,-4.89771657922137,
42.5700282164743));
#48501=CARTESIAN_POINT('Ctrl Pts',(-6.09223400357626,-5.05038609992736,
42.5778474396433));
#48502=CARTESIAN_POINT('Ctrl Pts',(-5.96634494839708,-5.19849028389335,
42.5856666628123));
#48503=CARTESIAN_POINT('Ctrl Pts',(-5.83532506711406,-5.34161982558758,
42.5934858859812));
#48504=CARTESIAN_POINT('Ctrl Pts',(-5.70421447027605,-5.48484846732435,
42.6013105230245));
#48505=CARTESIAN_POINT('Ctrl Pts',(-5.56796621521892,-5.62309535359634,
42.6091351600679));
#48506=CARTESIAN_POINT('Ctrl Pts',(-5.42701555307506,-5.75599020036356,
42.6169597971111));
#48507=CARTESIAN_POINT('Ctrl Pts',(-5.28588402170887,-5.88905557905466,
42.6247944748027));
#48508=CARTESIAN_POINT('Ctrl Pts',(-5.14003830250138,-6.01675497905471,
42.6326291524942));
#48509=CARTESIAN_POINT('Ctrl Pts',(-4.9899448138045,-6.13875978966319,42.6404638301857));
#48510=CARTESIAN_POINT('Ctrl Pts',(-4.97365081118194,-6.1520045128106,42.6413143551483));
#48511=CARTESIAN_POINT('Ctrl Pts',(-4.95730677432316,-6.16518216827127,
42.6421648801108));
#48512=CARTESIAN_POINT('Ctrl Pts',(-4.94091331848041,-6.17829236757722,
42.6430154050734));
#48513=CARTESIAN_POINT('Ctrl Pts',(-4.78976977061013,-6.29916511432414,
42.6508570317337));
#48514=CARTESIAN_POINT('Ctrl Pts',(-4.6339499961255,-6.41467861723858,42.6586986583941));
#48515=CARTESIAN_POINT('Ctrl Pts',(-4.47387290355124,-6.52444497584814,
42.6665402850544));
#48516=CARTESIAN_POINT('Ctrl Pts',(-4.31398428969263,-6.63408209284067,
42.6743726787902));
#48517=CARTESIAN_POINT('Ctrl Pts',(-4.14984862551579,-6.73798534271742,
42.682205072526));
#48518=CARTESIAN_POINT('Ctrl Pts',(-3.98191927558171,-6.83580572301107,
42.6900374662618));
#48519=CARTESIAN_POINT('Ctrl Pts',(-3.81415495933828,-6.9335299696724,42.6978621626603));
#48520=CARTESIAN_POINT('Ctrl Pts',(-3.64260468331891,-7.02518307570911,
42.7056868590588));
#48521=CARTESIAN_POINT('Ctrl Pts',(-3.46775245403099,-7.11045806664817,
42.7135115554573));
#48522=CARTESIAN_POINT('Ctrl Pts',(-3.29303804429053,-7.19566584334176,
42.7213300843844));
#48523=CARTESIAN_POINT('Ctrl Pts',(-3.11502717932611,-7.27450536421443,
42.7291486133116));
#48524=CARTESIAN_POINT('Ctrl Pts',(-2.9342304073972,-7.34671443002283,42.7369671422387));
#48525=CARTESIAN_POINT('Ctrl Pts',(-2.75354098088784,-7.41888062276231,
42.7447810290295));
#48526=CARTESIAN_POINT('Ctrl Pts',(-2.5700692679648,-7.48442407223109,42.7525949158203));
#48527=CARTESIAN_POINT('Ctrl Pts',(-2.38434801111233,-7.5431296927671,42.7604088026111));
#48528=CARTESIAN_POINT('Ctrl Pts',(-2.19870091627492,-7.60181187103706,
42.7682195691689));
#48529=CARTESIAN_POINT('Ctrl Pts',(-2.01080640209859,-7.65366155461945,
42.7760303357267));
#48530=CARTESIAN_POINT('Ctrl Pts',(-1.82121485153133,-7.69851267872968,
42.7838411022845));
#48531=CARTESIAN_POINT('Ctrl Pts',(-1.63163083630754,-7.74336202022554,
42.7916515584023));
#48532=CARTESIAN_POINT('Ctrl Pts',(-1.44035025919597,-7.78121326662324,
42.7994620145201));
#48533=CARTESIAN_POINT('Ctrl Pts',(-1.24793670675543,-7.81195077915449,
42.8072724706378));
#48534=CARTESIAN_POINT('Ctrl Pts',(-1.0555178479215,-7.84268913936685,42.8150831421529));
#48535=CARTESIAN_POINT('Ctrl Pts',(-0.86196629896923,-7.86631331859884,
42.8228938136679));
#48536=CARTESIAN_POINT('Ctrl Pts',(-0.667853804383722,-7.88275918038666,
42.8307044851829));
#48537=CARTESIAN_POINT('Ctrl Pts',(-0.473701770577963,-7.89920839206988,
42.8385167476716));
#48538=CARTESIAN_POINT('Ctrl Pts',(-0.27898891418997,-7.908476343858,42.8463290101603));
#48539=CARTESIAN_POINT('Ctrl Pts',(-0.0842901939676469,-7.91055093929626,
42.854141272649));
#48540=CARTESIAN_POINT('Ctrl Pts',(0.110482476612491,-7.91262632270618,
42.8619565023867));
#48541=CARTESIAN_POINT('Ctrl Pts',(0.305240648751071,-7.907502903694,42.8697717321245));
#48542=CARTESIAN_POINT('Ctrl Pts',(0.499411121469912,-7.89522067657087,
42.8775869618623));
#48543=CARTESIAN_POINT('Ctrl Pts',(0.693792764004116,-7.88292509192949,
42.8854106910419));
#48544=CARTESIAN_POINT('Ctrl Pts',(0.887585079272827,-7.86345517138622,
42.8932344202214));
#48545=CARTESIAN_POINT('Ctrl Pts',(1.0802206752646,-7.83690272318924,42.9010581494009));
#48546=CARTESIAN_POINT('Ctrl Pts',(1.27297314782017,-7.8103341649951,42.9088866254217));
#48547=CARTESIAN_POINT('Ctrl Pts',(1.464567156976,-7.77667457607048,42.9167151014424));
#48548=CARTESIAN_POINT('Ctrl Pts',(1.65444713907479,-7.73606654986934,42.9245435774631));
#48549=CARTESIAN_POINT('Ctrl Pts',(1.84458844924595,-7.69540263564307,42.9323828276609));
#48550=CARTESIAN_POINT('Ctrl Pts',(2.03301068071,-7.64777126942025,42.9402220778587));
#48551=CARTESIAN_POINT('Ctrl Pts',(2.21917390866053,-7.59336474582384,42.9480613280565));
#48552=CARTESIAN_POINT('Ctrl Pts',(2.32354876361187,-7.56286101492435,42.9524565064778));
#48553=CARTESIAN_POINT('Ctrl Pts',(2.42721386694964,-7.53022843219252,42.956851684899));
#48554=CARTESIAN_POINT('Ctrl Pts',(2.5300771028892,-7.49550737798555,42.9612468633203));
#48555=CARTESIAN_POINT('Ctrl Pts',(2.71519729417709,-7.43302083322734,42.9691567473781));
#48556=CARTESIAN_POINT('Ctrl Pts',(2.89825112111964,-7.36358785461777,42.9770666314358));
#48557=CARTESIAN_POINT('Ctrl Pts',(3.07867941314536,-7.28736262793851,42.9849765154936));
#48558=CARTESIAN_POINT('Ctrl Pts',(3.25891154936043,-7.21122027086337,42.992877800181));
#48559=CARTESIAN_POINT('Ctrl Pts',(3.43652352126279,-7.12830050708488,43.0007790848683));
#48560=CARTESIAN_POINT('Ctrl Pts',(3.61097120465141,-7.0388072824292,43.0086803695556));
#48561=CARTESIAN_POINT('Ctrl Pts',(3.78526165073689,-6.94939472191891,43.0165745324706));
#48562=CARTESIAN_POINT('Ctrl Pts',(3.95639318493084,-6.85342065991789,43.0244686953856));
#48563=CARTESIAN_POINT('Ctrl Pts',(4.12384131043278,-6.75113722615442,43.0323628583005));
#48564=CARTESIAN_POINT('Ctrl Pts',(4.29116961380941,-6.64892698412351,43.0402513723294));
#48565=CARTESIAN_POINT('Ctrl Pts',(4.45481946661778,-6.54041654446315,43.0481398863583));
#48566=CARTESIAN_POINT('Ctrl Pts',(4.61429041088716,-6.42590421683943,43.0560284003873));
#48567=CARTESIAN_POINT('Ctrl Pts',(4.77367685895037,-6.31145256395047,43.063912734661));
#48568=CARTESIAN_POINT('Ctrl Pts',(4.92888853101546,-6.19100556059785,43.0717970689347));
#48569=CARTESIAN_POINT('Ctrl Pts',(5.07945320974837,-6.0649052828529,43.0796814032084));
#48570=CARTESIAN_POINT('Ctrl Pts',(5.22996607024078,-5.93884840369633,43.0875630240149));
#48571=CARTESIAN_POINT('Ctrl Pts',(5.37583486070327,-5.80714234904797,43.0954446448213));
#48572=CARTESIAN_POINT('Ctrl Pts',(5.51661955856436,-5.67017016023903,43.1033262656277));
#48573=CARTESIAN_POINT('Ctrl Pts',(5.65740610033338,-5.53319617745597,43.1112079896626));
#48574=CARTESIAN_POINT('Ctrl Pts',(5.79310816325151,-5.3909561571011,43.1190897136975));
#48575=CARTESIAN_POINT('Ctrl Pts',(5.9233213853265,-5.24387116223633,43.1269714377324));
#48576=CARTESIAN_POINT('Ctrl Pts',(6.05354245146998,-5.09677730694437,43.1348536365637));
#48577=CARTESIAN_POINT('Ctrl Pts',(6.17827378864938,-4.94483815361627,43.1427358353951));
#48578=CARTESIAN_POINT('Ctrl Pts',(6.29715024632641,-4.78850913909447,43.1506180342265));
#48579=CARTESIAN_POINT('Ctrl Pts',(6.41605386852112,-4.63214440175283,43.158502034223));
#48580=CARTESIAN_POINT('Ctrl Pts',(6.52909973635385,-4.471388079023,43.1663860342195));
#48581=CARTESIAN_POINT('Ctrl Pts',(6.63596494679445,-4.30672616089244,43.174270034216));
#48582=CARTESIAN_POINT('Ctrl Pts',(6.74287255953469,-4.14199890771071,43.1821571624497));
#48583=CARTESIAN_POINT('Ctrl Pts',(6.84359444060331,-3.97336326049963,43.1900442906835));
#48584=CARTESIAN_POINT('Ctrl Pts',(6.93785258916042,-3.8013316681237,43.1979314189172));
#48585=CARTESIAN_POINT('Ctrl Pts',(7.03221130039376,-3.629116537692,43.2058269618157));
#48586=CARTESIAN_POINT('Ctrl Pts',(7.12009233889316,-3.45349852796777,43.2137225047142));
#48587=CARTESIAN_POINT('Ctrl Pts',(7.20126451919202,-3.27501302663458,43.2216180476127));
#48588=CARTESIAN_POINT('Ctrl Pts',(7.28248613053575,-3.09641883381627,43.2295183986233));
#48589=CARTESIAN_POINT('Ctrl Pts',(7.35699060808092,-2.91495398644879,43.2374187496338));
#48590=CARTESIAN_POINT('Ctrl Pts',(7.42459590233919,-2.73117130311668,43.2453191006443));
#48591=CARTESIAN_POINT('Ctrl Pts',(7.49228922153324,-2.54714932700325,43.2532297382441));
#48592=CARTESIAN_POINT('Ctrl Pts',(7.55306530770237,-2.36080381382491,43.2611403758438));
#48593=CARTESIAN_POINT('Ctrl Pts',(7.6067923898368,-2.17270120769538,43.2690510134435));
#48594=CARTESIAN_POINT('Ctrl Pts',(7.63039895053558,-2.0900528409353,43.272526782818));
#48595=CARTESIAN_POINT('Ctrl Pts',(7.65264534020375,-2.00706537838969,43.2760025521925));
#48596=CARTESIAN_POINT('Ctrl Pts',(7.67352353208574,-1.92378730698753,43.279478321567));
#48597=CARTESIAN_POINT('Ctrl Pts',(7.72103637620601,-1.73427003233409,43.2873881870105));
#48598=CARTESIAN_POINT('Ctrl Pts',(7.76158824895091,-1.54273577210148,43.2952980524539));
#48599=CARTESIAN_POINT('Ctrl Pts',(7.79500657608151,-1.34973830013301,43.3032079178973));
#48600=CARTESIAN_POINT('Ctrl Pts',(7.82838858442728,-1.15695057635546,43.3111091869589));
#48601=CARTESIAN_POINT('Ctrl Pts',(7.8546524309102,-0.962703145096539,43.3190104560205));
#48602=CARTESIAN_POINT('Ctrl Pts',(7.87367553765369,-0.767564021925151,
43.326911725082));
#48603=CARTESIAN_POINT('Ctrl Pts',(7.89268150517765,-0.572600712952502,
43.3348058753493));
#48604=CARTESIAN_POINT('Ctrl Pts',(7.90445969534575,-0.376747653637676,
43.3427000256165));
#48605=CARTESIAN_POINT('Ctrl Pts',(7.9089386771246,-0.180582395273219,43.3505941758837));
#48606=CARTESIAN_POINT('Ctrl Pts',(7.91341445552419,0.0154425651954087,
43.3584826802344));
#48607=CARTESIAN_POINT('Ctrl Pts',(7.91060141846242,0.211778936393597,43.3663711845851));
#48608=CARTESIAN_POINT('Ctrl Pts',(7.90047998062532,0.407844425901003,43.3742596889358));
#48609=CARTESIAN_POINT('Ctrl Pts',(7.89036390187049,0.603806102975317,43.3821440164942));
#48610=CARTESIAN_POINT('Ctrl Pts',(7.87294715080648,0.799496840469732,43.3900283440526));
#48611=CARTESIAN_POINT('Ctrl Pts',(7.84826222883147,0.994334444488994,43.3979126716109));
#48612=CARTESIAN_POINT('Ctrl Pts',(7.82358579314876,1.18910506637002,43.4057942886601));
#48613=CARTESIAN_POINT('Ctrl Pts',(7.79164620979011,1.38302279749853,43.4136759057093));
#48614=CARTESIAN_POINT('Ctrl Pts',(7.75252784787185,1.5755103833271,43.4215575227585));
#48615=CARTESIAN_POINT('Ctrl Pts',(7.7134089516409,1.76800059831891,43.4294392474617));
#48616=CARTESIAN_POINT('Ctrl Pts',(7.66711114124667,1.95906028924922,43.4373209721648));
#48617=CARTESIAN_POINT('Ctrl Pts',(7.61377005084622,2.14812164758823,43.445202696868));
#48618=CARTESIAN_POINT('Ctrl Pts',(7.56042572850756,2.33719446116041,43.4530848991251));
#48619=CARTESIAN_POINT('Ctrl Pts',(7.50003736894496,2.52426836850037,43.4609671013822));
#48620=CARTESIAN_POINT('Ctrl Pts',(7.43279072190796,2.70878996681524,43.4688493036393));
#48621=CARTESIAN_POINT('Ctrl Pts',(7.36552868477923,2.8933537948092,43.4767333098201));
#48622=CARTESIAN_POINT('Ctrl Pts',(7.29140535068825,3.07536382558975,43.4846173160008));
#48623=CARTESIAN_POINT('Ctrl Pts',(7.21065501198952,3.25428568169274,43.4925013221815));
#48624=CARTESIAN_POINT('Ctrl Pts',(7.12987260467482,3.43327859355085,43.5003884593605));
#48625=CARTESIAN_POINT('Ctrl Pts',(7.04245809050236,3.60918057272071,43.5082755965394));
#48626=CARTESIAN_POINT('Ctrl Pts',(6.94869229507463,3.78148071373773,43.5161627337184));
#48627=CARTESIAN_POINT('Ctrl Pts',(6.85482641325402,3.95396476936381,43.5240582896934));
#48628=CARTESIAN_POINT('Ctrl Pts',(6.7545958738127,4.12283900429356,43.5319538456684));
#48629=CARTESIAN_POINT('Ctrl Pts',(6.6483261086347,4.28761949725559,43.5398494016435));
#48630=CARTESIAN_POINT('Ctrl Pts',(6.54199159697163,4.45250038526138,43.5477497681071));
#48631=CARTESIAN_POINT('Ctrl Pts',(6.42961072118199,4.61328227678453,43.5556501345708));
#48632=CARTESIAN_POINT('Ctrl Pts',(6.31155014000222,4.76951316490875,43.5635505010344));
#48633=CARTESIAN_POINT('Ctrl Pts',(6.193335786551,4.92594754160046,43.571461157616));
#48634=CARTESIAN_POINT('Ctrl Pts',(6.06942716860398,5.0778188082938,43.5793718141975));
#48635=CARTESIAN_POINT('Ctrl Pts',(5.94022958811885,5.22470989055253,43.587282470779));
#48636=CARTESIAN_POINT('Ctrl Pts',(5.8834629938259,5.28925062297586,43.5907582404573));
#48637=CARTESIAN_POINT('Ctrl Pts',(5.82567580896491,5.35283041298148,43.5942340101355));
#48638=CARTESIAN_POINT('Ctrl Pts',(5.76690448498989,5.41541629618661,43.5977097798138));
#48639=CARTESIAN_POINT('Ctrl Pts',(5.63435879033588,5.55656488369309,43.6055486079242));
#48640=CARTESIAN_POINT('Ctrl Pts',(5.49642770460188,5.69305753192045,43.6133874360346));
#48641=CARTESIAN_POINT('Ctrl Pts',(5.35347325052906,5.82445234814998,43.6212262641451));
#48642=CARTESIAN_POINT('Ctrl Pts',(5.21067904618544,5.95569987282532,43.6290563050506));
#48643=CARTESIAN_POINT('Ctrl Pts',(5.06287294244189,6.08186070890334,43.636886345956));
#48644=CARTESIAN_POINT('Ctrl Pts',(4.91045639755445,6.2025268212009,43.6447163868615));
#48645=CARTESIAN_POINT('Ctrl Pts',(4.75818104479671,6.3230811536035,43.652539174354));
#48646=CARTESIAN_POINT('Ctrl Pts',(4.60130402998158,6.43815068211475,43.6603619618465));
#48647=CARTESIAN_POINT('Ctrl Pts',(4.4402628923503,6.54736484754111,43.668184749339));
#48648=CARTESIAN_POINT('Ctrl Pts',(4.2793396101219,6.65649908631235,43.6760018118485));
#48649=CARTESIAN_POINT('Ctrl Pts',(4.11425856448946,6.75978630029101,43.683818874358));
#48650=CARTESIAN_POINT('Ctrl Pts',(3.94548968584606,6.85689668427944,43.6916359368675));
#48651=CARTESIAN_POINT('Ctrl Pts',(3.77681150067302,6.95395488283058,43.6994487986231));
#48652=CARTESIAN_POINT('Ctrl Pts',(3.6044497343129,7.04484268857589,43.7072616603787));
#48653=CARTESIAN_POINT('Ctrl Pts',(3.4289027180311,7.12927395674194,43.7150745221343));
#48654=CARTESIAN_POINT('Ctrl Pts',(3.25341591070757,7.21367626674733,43.7228847042415));
#48655=CARTESIAN_POINT('Ctrl Pts',(3.07474634675879,7.29162629907549,43.7306948863488));
#48656=CARTESIAN_POINT('Ctrl Pts',(2.8934165052976,7.36288407669654,43.7385050684561));
#48657=CARTESIAN_POINT('Ctrl Pts',(2.71207848574386,7.43414506808922,43.7463156028076));
#48658=CARTESIAN_POINT('Ctrl Pts',(2.52808027299092,7.49871306450029,43.7541261371591));
#48659=CARTESIAN_POINT('Ctrl Pts',(2.34196433521704,7.55639623448714,43.7619366715106));
#48660=CARTESIAN_POINT('Ctrl Pts',(2.15583348007587,7.61408402783426,43.7697478318838));
#48661=CARTESIAN_POINT('Ctrl Pts',(1.96758489780044,7.66488579049288,43.777558992257));
#48662=CARTESIAN_POINT('Ctrl Pts',(1.7777761413379,7.70865961054772,43.7853701526301));
#48663=CARTESIAN_POINT('Ctrl Pts',(1.58791874245647,7.75244464854915,43.7931833147747));
#48664=CARTESIAN_POINT('Ctrl Pts',(1.39650071577984,7.78919807689108,43.8009964769192));
#48665=CARTESIAN_POINT('Ctrl Pts',(1.20408987311681,7.81882910527258,43.8088096390638));
#48666=CARTESIAN_POINT('Ctrl Pts',(1.01159583085082,7.84847294628855,43.8166261796665));
#48667=CARTESIAN_POINT('Ctrl Pts',(0.818108464844139,7.87098819881346,43.8244427202693));
#48668=CARTESIAN_POINT('Ctrl Pts',(0.624200925947996,7.88633591752505,43.832259260872));
#48669=CARTESIAN_POINT('Ctrl Pts',(0.430067093424239,7.90170154730375,43.8400849235199));
#48670=CARTESIAN_POINT('Ctrl Pts',(0.235512459454907,7.90988290886475,43.8479105861679));
#48671=CARTESIAN_POINT('Ctrl Pts',(0.0411115081473399,7.91089317611468,
43.8557362488158));
#48672=CARTESIAN_POINT('Ctrl Pts',(-0.153416159942628,7.91190410188925,
43.8635670124819));
#48673=CARTESIAN_POINT('Ctrl Pts',(-0.34778959534068,7.90573462937797,43.871397776148));
#48674=CARTESIAN_POINT('Ctrl Pts',(-0.541439143345873,7.89244985122192,
43.8792285398141));
#48675=CARTESIAN_POINT('Ctrl Pts',(-0.735368494589738,7.87914587795805,
43.8870706181105));
#48676=CARTESIAN_POINT('Ctrl Pts',(-0.928571520869114,7.85870610168352,
43.8949126964069));
#48677=CARTESIAN_POINT('Ctrl Pts',(-1.12048728004616,7.83124697958472,43.9027547747032));
#48678=CARTESIAN_POINT('Ctrl Pts',(-1.22805613405249,7.8158561314915,43.9071502624891));
#48679=CARTESIAN_POINT('Ctrl Pts',(-1.33522080975073,7.79826099232864,43.9115457502749));
#48680=CARTESIAN_POINT('Ctrl Pts',(-1.4418846728385,7.77848890146624,43.9159412380607));
#48681=CARTESIAN_POINT('Ctrl Pts',(-1.63399236896911,7.74287823902345,43.9238577620592));
#48682=CARTESIAN_POINT('Ctrl Pts',(-1.82505123055244,7.70009627128783,43.9317742860576));
#48683=CARTESIAN_POINT('Ctrl Pts',(-2.01448541291256,7.65021369120906,43.9396908100561));
#48684=CARTESIAN_POINT('Ctrl Pts',(-2.2037013555568,7.60038857890071,43.9475982137368));
#48685=CARTESIAN_POINT('Ctrl Pts',(-2.39129601721905,7.54347923481972,43.9555056174174));
#48686=CARTESIAN_POINT('Ctrl Pts',(-2.57670109950925,7.47960777339212,43.9634130210981));
#48687=CARTESIAN_POINT('Ctrl Pts',(-2.76192694035415,7.41579806007261,43.9713127802501));
#48688=CARTESIAN_POINT('Ctrl Pts',(-2.94496709509954,7.34503974866953,43.9792125394021));
#48689=CARTESIAN_POINT('Ctrl Pts',(-3.12526557042166,7.26750549462035,43.9871122985541));
#48690=CARTESIAN_POINT('Ctrl Pts',(-3.30542313960086,7.19003183483112,43.9950058839179));
#48691=CARTESIAN_POINT('Ctrl Pts',(-3.48284298314604,7.10579291813421,44.0028994692818));
#48692=CARTESIAN_POINT('Ctrl Pts',(-3.65698606732593,7.01501061320538,44.0107930546456));
#48693=CARTESIAN_POINT('Ctrl Pts',(-3.83102530592119,6.92428244388333,44.0186819328803));
#48694=CARTESIAN_POINT('Ctrl Pts',(-4.00179137401646,6.82701882018973,44.026570811115));
#48695=CARTESIAN_POINT('Ctrl Pts',(-4.16876670559107,6.72348906107204,44.0344596893497));
#48696=CARTESIAN_POINT('Ctrl Pts',(-4.33567338274859,6.62000186977078,44.0423453239536));
#48697=CARTESIAN_POINT('Ctrl Pts',(-4.49879213724428,6.51025385902708,44.0502309585574));
#48698=CARTESIAN_POINT('Ctrl Pts',(-4.65763119171931,6.39455961594881,44.0581165931612));
#48699=CARTESIAN_POINT('Ctrl Pts',(-4.81645611641754,6.27887566463308,44.0660015262861));
#48700=CARTESIAN_POINT('Ctrl Pts',(-4.97100181737944,6.15724673240566,44.073886459411));
#48701=CARTESIAN_POINT('Ctrl Pts',(-5.12080621286675,6.03003024289806,44.0817713925359));
#48702=CARTESIAN_POINT('Ctrl Pts',(-5.27061008897105,5.90281419445952,44.0896562983231));
#48703=CARTESIAN_POINT('Ctrl Pts',(-5.41567242922947,5.77001085004406,44.0975412041103));
#48704=CARTESIAN_POINT('Ctrl Pts',(-5.55556483856092,5.63201742935385,44.1054261098976));
#48705=CARTESIAN_POINT('Ctrl Pts',(-5.6954802334969,5.49400133508035,44.113312311247));
#48706=CARTESIAN_POINT('Ctrl Pts',(-5.83022375950345,5.35079370740464,44.1211985125965));
#48707=CARTESIAN_POINT('Ctrl Pts',(-5.95940427454596,5.20282823976762,44.129084713946));
#48708=CARTESIAN_POINT('Ctrl Pts',(-6.08862768864053,5.05481363485707,44.1369735341933));
#48709=CARTESIAN_POINT('Ctrl Pts',(-6.21228418432807,4.90203830134548,44.1448623544405));
#48710=CARTESIAN_POINT('Ctrl Pts',(-6.33002310350414,4.74496875744233,44.1527511746878));
#48711=CARTESIAN_POINT('Ctrl Pts',(-6.44787598308759,4.58774718471699,44.1606476305849));
#48712=CARTESIAN_POINT('Ctrl Pts',(-6.55979963871181,4.42622337539335,44.1685440864821));
#48713=CARTESIAN_POINT('Ctrl Pts',(-6.66548634053808,4.26089343261484,44.1764405423793));
#48714=CARTESIAN_POINT('Ctrl Pts',(-6.77123145551075,4.09547211181068,44.1843413626556));
#48715=CARTESIAN_POINT('Ctrl Pts',(-6.87073256935227,3.92624075975176,44.1922421829319));
#48716=CARTESIAN_POINT('Ctrl Pts',(-6.96372794869085,3.75372002906743,44.2001430032082));
#48717=CARTESIAN_POINT('Ctrl Pts',(-7.05683633000814,3.58098966233368,44.208053424051));
#48718=CARTESIAN_POINT('Ctrl Pts',(-7.14342303419475,3.40496224139899,44.2159638448938));
#48719=CARTESIAN_POINT('Ctrl Pts',(-7.22327404246507,3.22617933590962,44.2238742657366));
#48720=CARTESIAN_POINT('Ctrl Pts',(-7.25792622600135,3.14859461671368,44.2273070759269));
#48721=CARTESIAN_POINT('Ctrl Pts',(-7.29131056197855,3.07049119303736,44.2307398861171));
#48722=CARTESIAN_POINT('Ctrl Pts',(-7.32341248565942,2.99191419744746,44.2341726963074));
#48723=CARTESIAN_POINT('Ctrl Pts',(-7.40518696717657,2.79175195366992,44.2429172275151));
#48724=CARTESIAN_POINT('Ctrl Pts',(-7.4788016471458,2.58811213538503,44.2516617587229));
#48725=CARTESIAN_POINT('Ctrl Pts',(-7.54398366782736,2.38164468793185,44.2604062899307));
#48726=CARTESIAN_POINT('Ctrl Pts',(-7.60897890274335,2.17576889412544,44.2691257627874));
#48727=CARTESIAN_POINT('Ctrl Pts',(-7.66558964318761,1.96708185281294,44.2778452356441));
#48728=CARTESIAN_POINT('Ctrl Pts',(-7.71359248493486,1.75624940608001,44.2865647085008));
#48729=CARTESIAN_POINT('Ctrl Pts',(-7.76150465931262,1.54581517792442,44.2952677120894));
#48730=CARTESIAN_POINT('Ctrl Pts',(-7.80084132689146,1.33324384238952,44.3039707156781));
#48731=CARTESIAN_POINT('Ctrl Pts',(-7.83142878147297,1.11921590442453,44.3126737192668));
#48732=CARTESIAN_POINT('Ctrl Pts',(-7.86191715276629,0.905881276581177,
44.3213485308328));
#48733=CARTESIAN_POINT('Ctrl Pts',(-7.88371282848472,0.691099677687127,
44.3300233423988));
#48734=CARTESIAN_POINT('Ctrl Pts',(-7.89669319590675,0.475560269282509,
44.3386981539648));
#48735=CARTESIAN_POINT('Ctrl Pts',(-7.90615514801457,0.318444257588431,
44.3450215998977));
#48736=CARTESIAN_POINT('Ctrl Pts',(-7.91093403175593,0.160925906523633,
44.3513450458305));
#48737=CARTESIAN_POINT('Ctrl Pts',(-7.91099932156789,0.00327630163417495,
44.3576684917634));
#48738=CARTESIAN_POINT('',(-7.90417282333004,-0.00298459611092975,46.3576684917634));
#48739=CARTESIAN_POINT('Ctrl Pts',(-7.911,-9.02666830171484E-12,44.3576684917634));
#48740=CARTESIAN_POINT('Ctrl Pts',(-7.91099999999749,-2.20167589667567,
44.4462559274961));
#48741=CARTESIAN_POINT('Ctrl Pts',(-6.94214576671882,-4.38610418339452,
44.5348433632288));
#48742=CARTESIAN_POINT('Ctrl Pts',(-3.67820201487491,-7.34180684108027,
44.7120182346943));
#48743=CARTESIAN_POINT('Ctrl Pts',(-1.40868175870882,-8.08992666571483,
44.800605670427));
#48744=CARTESIAN_POINT('Ctrl Pts',(2.97309270522065,-7.65454228024946,44.9777805418924));
#48745=CARTESIAN_POINT('Ctrl Pts',(5.0510207267626,-6.47444880833709,45.0663679776252));
#48746=CARTESIAN_POINT('Ctrl Pts',(7.66951518848159,-2.93425195366947,45.2435428490906));
#48747=CARTESIAN_POINT('Ctrl Pts',(8.18956872247127,-0.601881960091208,
45.3321302848233));
#48748=CARTESIAN_POINT('Ctrl Pts',(7.32306689760989,3.71537198233139,45.5093051562888));
#48749=CARTESIAN_POINT('Ctrl Pts',(5.94329958849675,5.66643518937059,45.5978925920215));
#48750=CARTESIAN_POINT('Ctrl Pts',(2.16154501637136,7.92205913233188,45.7750674634869));
#48751=CARTESIAN_POINT('Ctrl Pts',(-0.210816529307585,8.20894963712981,
45.8636548992197));
#48752=CARTESIAN_POINT('Ctrl Pts',(-4.42123908577024,6.91982244717452,46.0408297706851));
#48753=CARTESIAN_POINT('Ctrl Pts',(-6.22631625634631,5.35390358803,46.1294172064178));
#48754=CARTESIAN_POINT('Ctrl Pts',(-7.65317280859711,2.3133485751382,46.2645592586882));
#48755=CARTESIAN_POINT('Ctrl Pts',(-7.91100000000129,1.15702837835713,46.3111138752258));
#48756=CARTESIAN_POINT('Ctrl Pts',(-7.911,-8.85624906743487E-12,46.3576684917634));
#48757=CARTESIAN_POINT('',(-7.91868218107619,-0.00107497954501803,48.3576177169414));
#48758=CARTESIAN_POINT('Ctrl Pts',(-7.90000441911832,-0.00480687251647904,
46.3576684917634));
#48759=CARTESIAN_POINT('Ctrl Pts',(-7.90593017288142,-0.869079961314315,
46.3923766291873));
#48760=CARTESIAN_POINT('Ctrl Pts',(-7.5759867787326,-3.05033090647266,46.4801233429855));
#48761=CARTESIAN_POINT('Ctrl Pts',(-5.56852494667735,-6.05216815598226,
46.6209086331589));
#48762=CARTESIAN_POINT('Ctrl Pts',(-0.809224834445862,-8.69093778987658,
46.8330629386561));
#48763=CARTESIAN_POINT('Ctrl Pts',(6.41510616868783,-6.81677508456639,47.0982558205292));
#48764=CARTESIAN_POINT('Ctrl Pts',(9.19981120649332,1.72383834166179,47.4164872787754));
#48765=CARTESIAN_POINT('Ctrl Pts',(3.5235845388455,8.66411051463959,47.7347187370226));
#48766=CARTESIAN_POINT('Ctrl Pts',(-5.25815706812825,7.6698522869705,48.0484059832181));
#48767=CARTESIAN_POINT('Ctrl Pts',(-7.9149434973087,2.51016233332767,48.2560160766646));
#48768=CARTESIAN_POINT('Ctrl Pts',(-7.92423877845688,-0.00105786062598127,
48.3575490173622));
#48769=CARTESIAN_POINT('',(-7.911,-8.51485548736264E-12,50.3576684917634));
#48770=CARTESIAN_POINT('Ctrl Pts',(-7.91099991958436,-0.00109864726889428,
48.3577126973937));
#48771=CARTESIAN_POINT('Ctrl Pts',(-7.91067767249818,-2.20240257181979,
48.4462853979163));
#48772=CARTESIAN_POINT('Ctrl Pts',(-6.94187431232755,-4.38635000211155,
48.5348580984389));
#48773=CARTESIAN_POINT('Ctrl Pts',(-3.67820201487496,-7.34180684108027,
48.7120182346943));
#48774=CARTESIAN_POINT('Ctrl Pts',(-1.40868175870879,-8.08992666571486,
48.800605670427));
#48775=CARTESIAN_POINT('Ctrl Pts',(2.97309270522083,-7.65454228024941,48.9777805418925));
#48776=CARTESIAN_POINT('Ctrl Pts',(5.05102072676283,-6.47444880833693,49.0663679776252));
#48777=CARTESIAN_POINT('Ctrl Pts',(7.66951518848176,-2.93425195366908,49.2435428490906));
#48778=CARTESIAN_POINT('Ctrl Pts',(8.18956872247132,-0.601881960090703,
49.3321302848234));
#48779=CARTESIAN_POINT('Ctrl Pts',(7.32306689760962,3.71537198233198,49.5093051562888));
#48780=CARTESIAN_POINT('Ctrl Pts',(5.94329958849625,5.66643518937114,49.5978925920215));
#48781=CARTESIAN_POINT('Ctrl Pts',(2.16154501637051,7.92205913233214,49.775067463487));
#48782=CARTESIAN_POINT('Ctrl Pts',(-0.21081652930856,8.2089496371298,49.8636548992197));
#48783=CARTESIAN_POINT('Ctrl Pts',(-4.42123908577119,6.91982244717394,50.0408297706851));
#48784=CARTESIAN_POINT('Ctrl Pts',(-6.22631625634712,5.3539035880291,50.1294172064179));
#48785=CARTESIAN_POINT('Ctrl Pts',(-7.65317280859725,2.31334857513749,50.2645592586882));
#48786=CARTESIAN_POINT('Ctrl Pts',(-7.91100000000124,1.15702837835694,50.3111138752258));
#48787=CARTESIAN_POINT('Ctrl Pts',(-7.911,-8.51485548736264E-12,50.3576684917634));
#48788=CARTESIAN_POINT('',(-7.90335554000322,-0.000571285354785519,52.3576684917634));
#48789=CARTESIAN_POINT('Ctrl Pts',(-7.911,-8.51485548736264E-12,50.3576684917634));
#48790=CARTESIAN_POINT('Ctrl Pts',(-7.91099999999763,-2.20167589667524,
50.4462559274961));
#48791=CARTESIAN_POINT('Ctrl Pts',(-6.94214576671903,-4.38610418339421,
50.5348433632288));
#48792=CARTESIAN_POINT('Ctrl Pts',(-3.67820201487512,-7.34180684108019,
50.7120182346943));
#48793=CARTESIAN_POINT('Ctrl Pts',(-1.40868175870896,-8.08992666571483,
50.800605670427));
#48794=CARTESIAN_POINT('Ctrl Pts',(2.97309270522067,-7.65454228024948,50.9777805418925));
#48795=CARTESIAN_POINT('Ctrl Pts',(5.05102072676269,-6.47444880833704,51.0663679776252));
#48796=CARTESIAN_POINT('Ctrl Pts',(7.66951518848169,-2.93425195366925,51.2435428490906));
#48797=CARTESIAN_POINT('Ctrl Pts',(8.18956872247131,-0.601881960090878,
51.3321302848233));
#48798=CARTESIAN_POINT('Ctrl Pts',(7.3230668976097,3.71537198233182,51.5093051562888));
#48799=CARTESIAN_POINT('Ctrl Pts',(5.94329958849637,5.66643518937101,51.5978925920215));
#48800=CARTESIAN_POINT('Ctrl Pts',(2.16154501637069,7.92205913233209,51.775067463487));
#48801=CARTESIAN_POINT('Ctrl Pts',(-0.210816529308383,8.20894963712981,
51.8636548992197));
#48802=CARTESIAN_POINT('Ctrl Pts',(-4.42123908577105,6.91982244717403,52.0408297706851));
#48803=CARTESIAN_POINT('Ctrl Pts',(-6.226316256347,5.35390358802923,52.1294172064179));
#48804=CARTESIAN_POINT('Ctrl Pts',(-7.65317280859717,2.31334857513772,52.2645592586882));
#48805=CARTESIAN_POINT('Ctrl Pts',(-7.91100000000119,1.15702837835726,52.3111138752258));
#48806=CARTESIAN_POINT('Ctrl Pts',(-7.911,-8.11961609059608E-12,52.3576684917634));
#48807=CARTESIAN_POINT('',(-7.91378807792777,-0.00677265886045676,54.3576684917634));
#48808=CARTESIAN_POINT('Ctrl Pts',(-7.89842547330135,-0.000939718817194635,
52.3576684917634));
#48809=CARTESIAN_POINT('Ctrl Pts',(-7.90062068210384,-1.25239052911004,
52.4078425314172));
#48810=CARTESIAN_POINT('Ctrl Pts',(-7.03041977659177,-5.14763933039878,
52.5640937238196));
#48811=CARTESIAN_POINT('Ctrl Pts',(-0.910171092806715,-9.31630818999036,
52.8264220689717));
#48812=CARTESIAN_POINT('Ctrl Pts',(5.95294509739285,-6.38354832108906,53.091614950844));
#48813=CARTESIAN_POINT('Ctrl Pts',(8.10656207347067,-1.3859512325431,53.3037692563418));
#48814=CARTESIAN_POINT('Ctrl Pts',(7.73558219899898,4.04326755765096,53.5159235618395));
#48815=CARTESIAN_POINT('Ctrl Pts',(2.23661238370502,9.08953105248759,53.781116443712));
#48816=CARTESIAN_POINT('Ctrl Pts',(-5.90135440155818,6.93085732631015,54.0793776124781));
#48817=CARTESIAN_POINT('Ctrl Pts',(-7.89488553833502,2.12997361947987,54.2715616284952));
#48818=CARTESIAN_POINT('Ctrl Pts',(-7.91378807792777,-0.00677265886045676,
54.3576684917634));
#48819=CARTESIAN_POINT('',(-7.91688330362235,0.00331809628778629,56.3576684917634));
#48820=CARTESIAN_POINT('Ctrl Pts',(-7.91378807792777,-0.00677265886045676,
54.3576684917634));
#48821=CARTESIAN_POINT('Ctrl Pts',(-7.91817203959193,-0.502336428179145,
54.3776387812441));
#48822=CARTESIAN_POINT('Ctrl Pts',(-7.64902003038262,-3.6253689198465,54.5036862234736));
#48823=CARTESIAN_POINT('Ctrl Pts',(-3.50021070610332,-8.68082195856808,
54.7358108184526));
#48824=CARTESIAN_POINT('Ctrl Pts',(5.42135646210964,-7.63091762632114,55.0540422766991));
#48825=CARTESIAN_POINT('Ctrl Pts',(8.68027656630637,-0.916538724054716,
55.3192351585718));
#48826=CARTESIAN_POINT('Ctrl Pts',(7.02947994193568,4.26891335306067,55.5313894640693));
#48827=CARTESIAN_POINT('Ctrl Pts',(3.18951819903458,8.12491342466588,55.7435437695676));
#48828=CARTESIAN_POINT('Ctrl Pts',(-4.27115340882762,8.32942124443492,56.0087366514396));
#48829=CARTESIAN_POINT('Ctrl Pts',(-7.79718755544591,3.13560819023932,56.2311244176299));
#48830=CARTESIAN_POINT('Ctrl Pts',(-7.92357763626265,0.256741869022418,
56.3474350310711));
#48831=CARTESIAN_POINT('Ctrl Pts',(-7.92188845760677,0.00332019403032202,
56.3576684917634));
#48832=CARTESIAN_POINT('',(-7.91099861016705,0.00331586588032432,58.3576684917633));
#48833=CARTESIAN_POINT('Ctrl Pts',(-7.9109993051824,0.0033156302070531,
56.3576684917634));
#48834=CARTESIAN_POINT('Ctrl Pts',(-7.91108018991349,-0.189673036065407,
56.3654723476325));
#48835=CARTESIAN_POINT('Ctrl Pts',(-7.90409495673348,-0.382940414989945,
56.3732762035016));
#48836=CARTESIAN_POINT('Ctrl Pts',(-7.89000870977794,-0.575919751031557,
56.3810800593707));
#48837=CARTESIAN_POINT('Ctrl Pts',(-7.87593671431612,-0.768703843882773,
56.3888760198363));
#48838=CARTESIAN_POINT('Ctrl Pts',(-7.85477803540268,-0.961200123166922,
56.3966719803019));
#48839=CARTESIAN_POINT('Ctrl Pts',(-7.82654975269139,-1.15283995795008,
56.4044679407676));
#48840=CARTESIAN_POINT('Ctrl Pts',(-7.79834443083918,-1.34432391306864,
56.4122575600062));
#48841=CARTESIAN_POINT('Ctrl Pts',(-7.76308100786333,-1.53495246175189,
56.4200471792447));
#48842=CARTESIAN_POINT('Ctrl Pts',(-7.72082851955789,-1.72416007713366,
56.4278367984833));
#48843=CARTESIAN_POINT('Ctrl Pts',(-7.67860202482051,-1.91325129271923,
56.4356216255782));
#48844=CARTESIAN_POINT('Ctrl Pts',(-7.62939510544607,-2.1009229707498,56.443406452673));
#48845=CARTESIAN_POINT('Ctrl Pts',(-7.57332824800153,-2.28661764359985,
56.4511912797678));
#48846=CARTESIAN_POINT('Ctrl Pts',(-7.51510904103691,-2.47944094570087,
56.4592749584414));
#48847=CARTESIAN_POINT('Ctrl Pts',(-7.44949282727851,-2.67013205625295,
56.467358637115));
#48848=CARTESIAN_POINT('Ctrl Pts',(-7.37667233441845,-2.85808087195332,
56.4754423157885));
#48849=CARTESIAN_POINT('Ctrl Pts',(-7.30657826779504,-3.03899281434856,
56.4832233385371));
#48850=CARTESIAN_POINT('Ctrl Pts',(-7.22980973278331,-3.21736372312977,
56.4910043612857));
#48851=CARTESIAN_POINT('Ctrl Pts',(-7.14658865764285,-3.39266732210079,
56.4987853840343));
#48852=CARTESIAN_POINT('Ctrl Pts',(-7.06336557376309,-3.56797515244263,
56.5065665945964));
#48853=CARTESIAN_POINT('Ctrl Pts',(-6.97368979141322,-3.740215204408,56.5143478051585));
#48854=CARTESIAN_POINT('Ctrl Pts',(-6.87783030434885,-3.90888363917125,
56.5221290157207));
#48855=CARTESIAN_POINT('Ctrl Pts',(-6.78195130289631,-4.07758641024703,
56.529911810326));
#48856=CARTESIAN_POINT('Ctrl Pts',(-6.6798862651892,-4.2427158073662,56.5376946049312));
#48857=CARTESIAN_POINT('Ctrl Pts',(-6.57194887027541,-4.4037948460942,56.5454773995365));
#48858=CARTESIAN_POINT('Ctrl Pts',(-6.46397013174474,-4.56493558345842,
56.5532631752113));
#48859=CARTESIAN_POINT('Ctrl Pts',(-6.35011475401019,-4.72202257807922,
56.5610489508861));
#48860=CARTESIAN_POINT('Ctrl Pts',(-6.23073829652345,-4.87460985928475,
56.5688347265609));
#48861=CARTESIAN_POINT('Ctrl Pts',(-6.11123756686666,-5.0273559854833,56.5766286073115));
#48862=CARTESIAN_POINT('Ctrl Pts',(-5.9862044999284,-5.1755927654553,56.5844224880622));
#48863=CARTESIAN_POINT('Ctrl Pts',(-5.85603390862543,-5.31890852158873,
56.5922163688128));
#48864=CARTESIAN_POINT('Ctrl Pts',(-5.72578300336415,-5.46231270211623,
56.6000150583102));
#48865=CARTESIAN_POINT('Ctrl Pts',(-5.59038850528388,-5.60078955638088,
56.6078137478076));
#48866=CARTESIAN_POINT('Ctrl Pts',(-5.45028024240838,-5.7339660165729,56.615612437305));
#48867=CARTESIAN_POINT('Ctrl Pts',(-5.30999619300789,-5.86730956631885,
56.6234209114111));
#48868=CARTESIAN_POINT('Ctrl Pts',(-5.16498683685651,-5.9953392122672,56.6312293855172));
#48869=CARTESIAN_POINT('Ctrl Pts',(-5.01571372673485,-6.11772317218127,
56.6390378596233));
#48870=CARTESIAN_POINT('Ctrl Pts',(-4.97644965923604,-6.14991444935719,
56.6410917623933));
#48871=CARTESIAN_POINT('Ctrl Pts',(-4.93689074131798,-6.18171535351921,
56.6431456651633));
#48872=CARTESIAN_POINT('Ctrl Pts',(-4.89704567766127,-6.21312036185515,
56.6451995679333));
#48873=CARTESIAN_POINT('Ctrl Pts',(-4.74359679161102,-6.33406542012052,
56.6531094333768));
#48874=CARTESIAN_POINT('Ctrl Pts',(-4.58545758517985,-6.449485602999,56.6610192988203));
#48875=CARTESIAN_POINT('Ctrl Pts',(-4.42306262451535,-6.55899672355577,
56.6689291642637));
#48876=CARTESIAN_POINT('Ctrl Pts',(-4.26084415346442,-6.66838882825596,
56.6768304333253));
#48877=CARTESIAN_POINT('Ctrl Pts',(-4.09437942407764,-6.77188447093364,
56.6847317023869));
#48878=CARTESIAN_POINT('Ctrl Pts',(-3.92413646662417,-6.86913924675504,
56.6926329714486));
#48879=CARTESIAN_POINT('Ctrl Pts',(-3.75404689270852,-6.96630639908934,
56.7005271217158));
#48880=CARTESIAN_POINT('Ctrl Pts',(-3.58018616951,-7.05724371560999,56.7084212719831));
#48881=CARTESIAN_POINT('Ctrl Pts',(-3.40305196903901,-7.14164955007033,
56.7163154222503));
#48882=CARTESIAN_POINT('Ctrl Pts',(-3.22604445540244,-7.22599501726141,
56.7242039266011));
#48883=CARTESIAN_POINT('Ctrl Pts',(-3.04576843906962,-7.30381816143088,
56.7320924309518));
#48884=CARTESIAN_POINT('Ctrl Pts',(-2.862747145676,-7.37486269566586,56.7399809353026));
#48885=CARTESIAN_POINT('Ctrl Pts',(-2.67982275809595,-7.44586961335764,
56.747865262861));
#48886=CARTESIAN_POINT('Ctrl Pts',(-2.49415631067576,-7.5101049483499,56.7557495904194));
#48887=CARTESIAN_POINT('Ctrl Pts',(-2.30629226597316,-7.56735997451637,
56.7636339179779));
#48888=CARTESIAN_POINT('Ctrl Pts',(-2.11849280600797,-7.62459531729512,
56.7715155350271));
#48889=CARTESIAN_POINT('Ctrl Pts',(-1.92849758407093,-7.67485503349543,
56.7793971520763));
#48890=CARTESIAN_POINT('Ctrl Pts',(-1.73686779353118,-7.71797974004818,
56.7872787691255));
#48891=CARTESIAN_POINT('Ctrl Pts',(-1.54523538554448,-7.76110503563581,
56.7951604938287));
#48892=CARTESIAN_POINT('Ctrl Pts',(-1.35196869898921,-7.79709504277689,
56.8030422185319));
#48893=CARTESIAN_POINT('Ctrl Pts',(-1.15764129969557,-7.82584101686452,
56.8109239432351));
#48894=CARTESIAN_POINT('Ctrl Pts',(-0.96330212609917,-7.85458873267156,
56.8188061454923));
#48895=CARTESIAN_POINT('Ctrl Pts',(-0.767902453074723,-7.87609148971396,
56.8266883477494));
#48896=CARTESIAN_POINT('Ctrl Pts',(-0.572023223356488,-7.89029216391515,
56.8345705500066));
#48897=CARTESIAN_POINT('Ctrl Pts',(-0.376099164647193,-7.90449608808776,
56.8424545561874));
#48898=CARTESIAN_POINT('Ctrl Pts',(-0.179695674738636,-7.91139457442694,
56.8503385623682));
#48899=CARTESIAN_POINT('Ctrl Pts',(0.0166037853955017,-7.910982575781,56.8582225685489));
#48900=CARTESIAN_POINT('Ctrl Pts',(0.212981202500519,-7.91057041351684,
56.8661097057279));
#48901=CARTESIAN_POINT('Ctrl Pts',(0.409254162712939,-7.9028419820523,56.8739968429068));
#48902=CARTESIAN_POINT('Ctrl Pts',(0.60484156639343,-7.88784429863843,56.8818839800857));
#48903=CARTESIAN_POINT('Ctrl Pts',(0.800637741703501,-7.87283060657191,
56.8897795360607));
#48904=CARTESIAN_POINT('Ctrl Pts',(0.995746554669449,-7.85053219041334,
56.8976750920358));
#48905=CARTESIAN_POINT('Ctrl Pts',(1.18959326027058,-7.82104781184202,56.9055706480108));
#48906=CARTESIAN_POINT('Ctrl Pts',(1.38355806995182,-7.79154546946059,56.9134710144745));
#48907=CARTESIAN_POINT('Ctrl Pts',(1.57625890119976,-7.75484850062344,56.9213713809383));
#48908=CARTESIAN_POINT('Ctrl Pts',(1.76713324526486,-7.71110634691804,56.929271747402));
#48909=CARTESIAN_POINT('Ctrl Pts',(1.95825620051916,-7.66730721966335,56.9371824039836));
#48910=CARTESIAN_POINT('Ctrl Pts',(2.14754758453539,-7.6164446677572,56.9450930605651));
#48911=CARTESIAN_POINT('Ctrl Pts',(2.33446093623429,-7.55871769132808,56.9530037171467));
#48912=CARTESIAN_POINT('Ctrl Pts',(2.41658657947439,-7.5333537190465,56.9564794868245));
#48913=CARTESIAN_POINT('Ctrl Pts',(2.49825340183972,-7.50666517179851,56.9599552565024));
#48914=CARTESIAN_POINT('Ctrl Pts',(2.57941640384201,-7.47867180825518,56.9634310261802));
#48915=CARTESIAN_POINT('Ctrl Pts',(2.76246156522894,-7.41553898146043,56.9712698542906));
#48916=CARTESIAN_POINT('Ctrl Pts',(2.94346399646625,-7.34558651675808,56.979108682401));
#48917=CARTESIAN_POINT('Ctrl Pts',(3.12187231452425,-7.26896376740227,56.9869475105114));
#48918=CARTESIAN_POINT('Ctrl Pts',(3.30008063962085,-7.19242691096178,56.9947775514169));
#48919=CARTESIAN_POINT('Ctrl Pts',(3.47570032209801,-7.10923479600866,57.0026075923224));
#48920=CARTESIAN_POINT('Ctrl Pts',(3.64819472148541,-7.01958661703992,57.0104376332279));
#48921=CARTESIAN_POINT('Ctrl Pts',(3.82052932948186,-6.93002148428756,57.0182604207203));
#48922=CARTESIAN_POINT('Ctrl Pts',(3.98974411005337,-6.83401235865384,57.0260832082128));
#48923=CARTESIAN_POINT('Ctrl Pts',(4.1553218400315,-6.73180669699875,57.0339059957052));
#48924=CARTESIAN_POINT('Ctrl Pts',(4.32077839457395,-6.62967583293619,57.0417230582147));
#48925=CARTESIAN_POINT('Ctrl Pts',(4.48260290197556,-6.52135764885481,57.0495401207242));
#48926=CARTESIAN_POINT('Ctrl Pts',(4.64030205779981,-6.40714583979317,57.0573571832337));
#48927=CARTESIAN_POINT('Ctrl Pts',(4.79791646883156,-6.29299540617776,57.0651700449893));
#48928=CARTESIAN_POINT('Ctrl Pts',(4.95140966024248,-6.17295786235636,57.0729829067449));
#48929=CARTESIAN_POINT('Ctrl Pts',(5.10031653177235,-6.04737069111277,57.0807957685006));
#48930=CARTESIAN_POINT('Ctrl Pts',(5.24917233135645,-5.92182659364496,57.0886059506078));
#48931=CARTESIAN_POINT('Ctrl Pts',(5.39344467663459,-5.79073688768173,57.0964161327151));
#48932=CARTESIAN_POINT('Ctrl Pts',(5.53270070042722,-5.65447999019293,57.1042263148224));
#48933=CARTESIAN_POINT('Ctrl Pts',(5.67196300475582,-5.51821694743067,57.1120368491738));
#48934=CARTESIAN_POINT('Ctrl Pts',(5.80620827769993,-5.37678648696057,57.1198473835253));
#48935=CARTESIAN_POINT('Ctrl Pts',(5.93503939241925,-5.23060497556752,57.1276579178768));
#48936=CARTESIAN_POINT('Ctrl Pts',(6.06388083307358,-5.08441174758886,57.13546907825));
#48937=CARTESIAN_POINT('Ctrl Pts',(6.18730701767793,-4.93346697367534,57.1432802386232));
#48938=CARTESIAN_POINT('Ctrl Pts',(6.30496018621139,-4.77822122240999,57.1510913989963));
#48939=CARTESIAN_POINT('Ctrl Pts',(6.42264350580237,-4.62293568621037,57.1589045611409));
#48940=CARTESIAN_POINT('Ctrl Pts',(6.53455064947415,-4.4633472573478,57.1667177232854));
#48941=CARTESIAN_POINT('Ctrl Pts',(6.64036629668823,-4.29993679555956,57.17453088543));
#48942=CARTESIAN_POINT('Ctrl Pts',(6.74622769922347,-4.13645567410656,57.1823474260327));
#48943=CARTESIAN_POINT('Ctrl Pts',(6.84599216719703,-3.969149522604,57.1901639666355));
#48944=CARTESIAN_POINT('Ctrl Pts',(6.93938949391331,-3.79852529960846,57.1979805072383));
#48945=CARTESIAN_POINT('Ctrl Pts',(7.03289581700968,-3.62770195503938,57.2058061698862));
#48946=CARTESIAN_POINT('Ctrl Pts',(7.12001998885442,-3.45355311365304,57.2136318325341));
#48947=CARTESIAN_POINT('Ctrl Pts',(7.20053880696445,-3.27660829050392,57.221457495182));
#48948=CARTESIAN_POINT('Ctrl Pts',(7.28111010982523,-3.09954812903815,57.2292882588481));
#48949=CARTESIAN_POINT('Ctrl Pts',(7.35506734541584,-2.91968867812484,57.2371190225142));
#48950=CARTESIAN_POINT('Ctrl Pts',(7.42223665583889,-2.73757630482174,57.2449497861802));
#48951=CARTESIAN_POINT('Ctrl Pts',(7.48950301885456,-2.55520079828319,57.2527918644766));
#48952=CARTESIAN_POINT('Ctrl Pts',(7.54996175821235,-2.3705662006234,57.260633942773));
#48953=CARTESIAN_POINT('Ctrl Pts',(7.60348944494689,-2.18423196125806,57.2684760210694));
#48954=CARTESIAN_POINT('Ctrl Pts',(7.63349173316116,-2.07979155116989,57.2728715088552));
#48955=CARTESIAN_POINT('Ctrl Pts',(7.66131748299645,-1.97481734345205,57.2772669966411));
#48956=CARTESIAN_POINT('Ctrl Pts',(7.68695207033227,-1.86940869485901,57.281662484427));
#48957=CARTESIAN_POINT('Ctrl Pts',(7.73312142302325,-1.67956171156966,57.2895790084254));
#48958=CARTESIAN_POINT('Ctrl Pts',(7.77231871117484,-1.48773533706874,57.2974955324239));
#48959=CARTESIAN_POINT('Ctrl Pts',(7.80437265176402,-1.29448387877096,57.3054120564223));
#48960=CARTESIAN_POINT('Ctrl Pts',(7.83638966426137,-1.10145505792322,57.313319460103));
#48961=CARTESIAN_POINT('Ctrl Pts',(7.86127966514113,-0.90700475994466,57.3212268637836));
#48962=CARTESIAN_POINT('Ctrl Pts',(7.87892137472227,-0.711701461951944,
57.3291342674642));
#48963=CARTESIAN_POINT('Ctrl Pts',(7.89654602907775,-0.516586974561875,
57.3370340266162));
#48964=CARTESIAN_POINT('Ctrl Pts',(7.9069363203028,-0.32062147063296,57.3449337857683));
#48965=CARTESIAN_POINT('Ctrl Pts',(7.9100221172548,-0.124382894884864,57.3528335449203));
#48966=CARTESIAN_POINT('Ctrl Pts',(7.9131055026071,0.0717023172764458,57.3607271302841));
#48967=CARTESIAN_POINT('Ctrl Pts',(7.908895761514,0.268059833174569,57.3686207156479));
#48968=CARTESIAN_POINT('Ctrl Pts',(7.89737460578694,0.464107030620674,57.3765143010118));
#48969=CARTESIAN_POINT('Ctrl Pts',(7.8858603203938,0.660037320549568,57.3844031792465));
#48970=CARTESIAN_POINT('Ctrl Pts',(7.8670433281466,0.855657317763265,57.3922920574812));
#48971=CARTESIAN_POINT('Ctrl Pts',(7.84095742123833,1.05038455735388,57.400180935716));
#48972=CARTESIAN_POINT('Ctrl Pts',(7.81488223994292,1.24503173191201,57.4080665703198));
#48973=CARTESIAN_POINT('Ctrl Pts',(7.78154414606342,1.43878653940533,57.4159522049237));
#48974=CARTESIAN_POINT('Ctrl Pts',(7.74102879056715,1.6310715078164,57.4238378395275));
#48975=CARTESIAN_POINT('Ctrl Pts',(7.70051703917778,1.82333937121696,57.4317227726523));
#48976=CARTESIAN_POINT('Ctrl Pts',(7.65282936290027,2.01413731767258,57.4396077057772));
#48977=CARTESIAN_POINT('Ctrl Pts',(7.59810265271002,2.20289742813436,57.4474926389021));
#48978=CARTESIAN_POINT('Ctrl Pts',(7.54337613226107,2.39165688415176,57.4553775446893));
#48979=CARTESIAN_POINT('Ctrl Pts',(7.4816107219699,2.57837818700974,57.4632624504765));
#48980=CARTESIAN_POINT('Ctrl Pts',(7.41299341303602,2.76250785669192,57.4711473562638));
#48981=CARTESIAN_POINT('Ctrl Pts',(7.34436482965015,2.94666778056437,57.4790335576132));
#48982=CARTESIAN_POINT('Ctrl Pts',(7.26888222472407,3.12823489977492,57.4869197589627));
#48983=CARTESIAN_POINT('Ctrl Pts',(7.18678111885874,3.30667478739828,57.4948059603121));
#48984=CARTESIAN_POINT('Ctrl Pts',(7.10465274835829,3.48517393242599,57.5026947805594));
#48985=CARTESIAN_POINT('Ctrl Pts',(7.01590164162071,3.66054346372422,57.5105836008065));
#48986=CARTESIAN_POINT('Ctrl Pts',(6.9208098424507,3.83227244916611,57.5184724210538));
#48987=CARTESIAN_POINT('Ctrl Pts',(6.82562600319492,4.00416765241737,57.5263688769509));
#48988=CARTESIAN_POINT('Ctrl Pts',(6.72408937990399,4.17241496977283,57.5342653328481));
#48989=CARTESIAN_POINT('Ctrl Pts',(6.61652658460578,4.33653052049735,57.5421617887453));
#48990=CARTESIAN_POINT('Ctrl Pts',(6.50890433924238,4.50073677805189,57.5500626090216));
#48991=CARTESIAN_POINT('Ctrl Pts',(6.39524948026097,4.66080643540534,57.5579634292978));
#48992=CARTESIAN_POINT('Ctrl Pts',(6.27592985017476,4.81628752419178,57.5658642495741));
#48993=CARTESIAN_POINT('Ctrl Pts',(6.15646523058092,4.9719575435548,57.5737746704169));
#48994=CARTESIAN_POINT('Ctrl Pts',(6.03132230951853,5.12302759211004,57.5816850912596));
#48995=CARTESIAN_POINT('Ctrl Pts',(5.90090754944437,5.26908066866607,57.5895955121024));
#48996=CARTESIAN_POINT('Ctrl Pts',(5.84431269485101,5.33246193491155,57.5930283222929));
#48997=CARTESIAN_POINT('Ctrl Pts',(5.78672549096251,5.39489888412984,57.5964611324833));
#48998=CARTESIAN_POINT('Ctrl Pts',(5.72818115022042,5.45635974897729,57.5998939426738));
#48999=CARTESIAN_POINT('Ctrl Pts',(5.58638076990835,5.60522424893074,57.6082085600112));
#49000=CARTESIAN_POINT('Ctrl Pts',(5.43865226372989,5.7486861063339,57.6165231773487));
#49001=CARTESIAN_POINT('Ctrl Pts',(5.285423566284,5.88627375552393,57.6248377946862));
#49002=CARTESIAN_POINT('Ctrl Pts',(5.13238425182783,6.0236913532759,57.6331421355734));
#49003=CARTESIAN_POINT('Ctrl Pts',(4.97385852141849,6.15524902792256,57.6414464764606));
#49004=CARTESIAN_POINT('Ctrl Pts',(4.81031173073891,6.28051128914801,57.6497508173479));
#49005=CARTESIAN_POINT('Ctrl Pts',(4.64695626472553,6.40562701273603,57.6580454434296));
#49006=CARTESIAN_POINT('Ctrl Pts',(4.47859168602644,6.52446183427147,57.6663400695114));
#49007=CARTESIAN_POINT('Ctrl Pts',(4.30571770233826,6.63661932521152,57.6746346955932));
#49008=CARTESIAN_POINT('Ctrl Pts',(4.13310401412025,6.74860794119297,57.6829168324991));
#49009=CARTESIAN_POINT('Ctrl Pts',(3.95599471622409,6.85393913170547,57.6911989694049));
#49010=CARTESIAN_POINT('Ctrl Pts',(3.77491991420195,6.95225867192537,57.6994811063108));
#49011=CARTESIAN_POINT('Ctrl Pts',(3.59401209849676,7.05048754233522,57.7077556054696));
#49012=CARTESIAN_POINT('Ctrl Pts',(3.40914632805054,7.14171751741097,57.7160301046284));
#49013=CARTESIAN_POINT('Ctrl Pts',(3.22088038120729,7.22563841954149,57.7243046037872));
#49014=CARTESIAN_POINT('Ctrl Pts',(3.03283096999261,7.30946279935558,57.7325695859627));
#49015=CARTESIAN_POINT('Ctrl Pts',(2.84138945325158,7.38599476194414,57.7408345681381));
#49016=CARTESIAN_POINT('Ctrl Pts',(2.64713707734078,7.45497057631804,57.7490995503136));
#49017=CARTESIAN_POINT('Ctrl Pts',(2.56949768248666,7.48253904472132,57.7524029241415));
#49018=CARTESIAN_POINT('Ctrl Pts',(2.49140952558729,7.50890096427389,57.7557062979693));
#49019=CARTESIAN_POINT('Ctrl Pts',(2.41291071232974,7.53404160423371,57.7590096717972));
#49020=CARTESIAN_POINT('Ctrl Pts',(2.21648177341447,7.59695146268921,57.7672757612948));
#49021=CARTESIAN_POINT('Ctrl Pts',(2.01770248929773,7.65213956951669,57.7755418507925));
#49022=CARTESIAN_POINT('Ctrl Pts',(1.81719592044119,7.69946231802792,57.7838079402902));
#49023=CARTESIAN_POINT('Ctrl Pts',(1.61650903574976,7.74682762395239,57.7920814634935));
#49024=CARTESIAN_POINT('Ctrl Pts',(1.41409205108396,7.78631338306703,57.8003549866969));
#49025=CARTESIAN_POINT('Ctrl Pts',(1.21057718538857,7.81782731186976,57.8086285099003));
#49026=CARTESIAN_POINT('Ctrl Pts',(1.00686606113847,7.84937163097394,57.8169100116349));
#49027=CARTESIAN_POINT('Ctrl Pts',(0.802055232110211,7.87292872709926,57.8251915133695));
#49028=CARTESIAN_POINT('Ctrl Pts',(0.596781820702515,7.88845818005515,57.8334730151041));
#49029=CARTESIAN_POINT('Ctrl Pts',(0.391166633492497,7.90401348921525,57.8417683053604));
#49030=CARTESIAN_POINT('Ctrl Pts',(0.185087617456562,7.91151441118359,57.8500635956168));
#49031=CARTESIAN_POINT('Ctrl Pts',(-0.0208162702095703,7.91097261295314,
57.8583588858731));
#49032=CARTESIAN_POINT('Ctrl Pts',(-0.226906893306216,7.91043032336272,
57.8666616991764));
#49033=CARTESIAN_POINT('Ctrl Pts',(-0.432821777805041,7.90183076150704,
57.8749645124796));
#49034=CARTESIAN_POINT('Ctrl Pts',(-0.637925996679285,7.88523756286142,
57.8832673257828));
#49035=CARTESIAN_POINT('Ctrl Pts',(-0.843344746839667,7.86861891822478,
57.8915828716108));
#49036=CARTESIAN_POINT('Ctrl Pts',(-1.04795005433127,7.84398216412009,57.8998984174388));
#49037=CARTESIAN_POINT('Ctrl Pts',(-1.25111422146588,7.81144251754091,57.9082139632668));
#49038=CARTESIAN_POINT('Ctrl Pts',(-1.33183247366865,7.79851433519354,57.9115177758181));
#49039=CARTESIAN_POINT('Ctrl Pts',(-1.4123233755187,7.7843392299535,57.9148215883693));
#49040=CARTESIAN_POINT('Ctrl Pts',(-1.49254815857286,7.76892663077344,57.9181254009206));
#49041=CARTESIAN_POINT('Ctrl Pts',(-1.68461541594747,7.7320271149277,57.9260351040254));
#49042=CARTESIAN_POINT('Ctrl Pts',(-1.87555687338099,7.68795403783527,57.9339448071301));
#49043=CARTESIAN_POINT('Ctrl Pts',(-2.06479726327526,7.63678815088981,57.9418545102349));
#49044=CARTESIAN_POINT('Ctrl Pts',(-2.25384565956987,7.58567417423063,57.9497561885603));
#49045=CARTESIAN_POINT('Ctrl Pts',(-2.44119609606983,7.52748181085078,57.9576578668857));
#49046=CARTESIAN_POINT('Ctrl Pts',(-2.62628186223298,7.46234310254534,57.9655595452111));
#49047=CARTESIAN_POINT('Ctrl Pts',(-2.81121413740715,7.39725841354656,57.9734546707019));
#49048=CARTESIAN_POINT('Ctrl Pts',(-2.99388516044192,7.32523896940155,57.9813497961927));
#49049=CARTESIAN_POINT('Ctrl Pts',(-3.17374151740871,7.24646712410098,57.9892449216835));
#49050=CARTESIAN_POINT('Ctrl Pts',(-3.35348202981113,7.16774601534515,57.9971349619641));
#49051=CARTESIAN_POINT('Ctrl Pts',(-3.53041117367976,7.08228130859005,58.0050250022447));
#49052=CARTESIAN_POINT('Ctrl Pts',(-3.70399345783124,6.99030424690824,58.0129150425254));
#49053=CARTESIAN_POINT('Ctrl Pts',(-3.87749607988108,6.89836939625086,58.0208014618305));
#49054=CARTESIAN_POINT('Ctrl Pts',(-4.04765459908768,6.79992830735376,58.0286878811357));
#49055=CARTESIAN_POINT('Ctrl Pts',(-4.21395591786019,6.69525925729028,58.0365743004408));
#49056=CARTESIAN_POINT('Ctrl Pts',(-4.38021170470164,6.59061886475041,58.0444585605094));
#49057=CARTESIAN_POINT('Ctrl Pts',(-4.5426121046703,6.47975409309515,58.0523428205779));
#49058=CARTESIAN_POINT('Ctrl Pts',(-4.70067068893039,6.36298798319082,58.0602270806464));
#49059=CARTESIAN_POINT('Ctrl Pts',(-4.85874772644488,6.24620824090617,58.0681122611981));
#49060=CARTESIAN_POINT('Ctrl Pts',(-5.01248165408357,6.12352598296695,58.0759974417497));
#49061=CARTESIAN_POINT('Ctrl Pts',(-5.16141647512,5.99530657851288,58.0838826223013));
#49062=CARTESIAN_POINT('Ctrl Pts',(-5.31036987272421,5.86707118131486,58.0917687863677));
#49063=CARTESIAN_POINT('Ctrl Pts',(-5.45452270916307,5.73329748584274,58.0996549504341));
#49064=CARTESIAN_POINT('Ctrl Pts',(-5.59345346139795,5.59438999133733,58.1075411145005));
#49065=CARTESIAN_POINT('Ctrl Pts',(-5.73242485256491,5.45544186470301,58.1154295853656));
#49066=CARTESIAN_POINT('Ctrl Pts',(-5.86617087174895,5.31135719017599,58.1233180562307));
#49067=CARTESIAN_POINT('Ctrl Pts',(-5.99430796580337,5.16257619906053,58.1312065270958));
#49068=CARTESIAN_POINT('Ctrl Pts',(-6.12250404117033,5.01372672427763,58.1390986290123));
#49069=CARTESIAN_POINT('Ctrl Pts',(-6.24508582190272,4.86017688609706,58.1469907309287));
#49070=CARTESIAN_POINT('Ctrl Pts',(-6.36171087831312,4.70239893041335,58.1548828328452));
#49071=CARTESIAN_POINT('Ctrl Pts',(-6.47847113835094,4.54443806247567,58.1627840840889));
#49072=CARTESIAN_POINT('Ctrl Pts',(-6.58926067549652,4.38223956342015,58.1706853353326));
#49073=CARTESIAN_POINT('Ctrl Pts',(-6.69378050152099,4.21630449534393,58.1785865865763));
#49074=CARTESIAN_POINT('Ctrl Pts',(-6.79836958543951,4.05025947383781,58.1864930734202));
#49075=CARTESIAN_POINT('Ctrl Pts',(-6.89668050385122,3.88047324462845,58.1943995602641));
#49076=CARTESIAN_POINT('Ctrl Pts',(-6.9884607543749,3.70747046981656,58.202306047108));
#49077=CARTESIAN_POINT('Ctrl Pts',(-7.08036744742426,3.53422935497321,58.2102234264496));
#49078=CARTESIAN_POINT('Ctrl Pts',(-7.16572535208359,3.35776315241992,58.2181408057912));
#49079=CARTESIAN_POINT('Ctrl Pts',(-7.24433005307879,3.17861653586264,58.2260581851327));
#49080=CARTESIAN_POINT('Ctrl Pts',(-7.2784122141163,3.10094047123132,58.2294910764776));
#49081=CARTESIAN_POINT('Ctrl Pts',(-7.31122540923108,3.02276068703856,58.2329239678225));
#49082=CARTESIAN_POINT('Ctrl Pts',(-7.34275591312242,2.9441223820191,58.2363568591674));
#49083=CARTESIAN_POINT('Ctrl Pts',(-7.42407168264268,2.74131768506709,58.2452101335189));
#49084=CARTESIAN_POINT('Ctrl Pts',(-7.49705846057189,2.53495023216138,58.2540634078704));
#49085=CARTESIAN_POINT('Ctrl Pts',(-7.56142423142031,2.32567938299537,58.2629166822218));
#49086=CARTESIAN_POINT('Ctrl Pts',(-7.62548007002129,2.11741620892984,58.2717273265359));
#49087=CARTESIAN_POINT('Ctrl Pts',(-7.68099762436967,1.90627770533604,58.28053797085));
#49088=CARTESIAN_POINT('Ctrl Pts',(-7.72773460272532,1.6929379521535,58.2893486151641));
#49089=CARTESIAN_POINT('Ctrl Pts',(-7.77432731373501,1.48025673448315,58.2981320628489));
#49090=CARTESIAN_POINT('Ctrl Pts',(-7.81219346255932,1.26538800816939,58.3069155105338));
#49091=CARTESIAN_POINT('Ctrl Pts',(-7.84113994178214,1.04902116918052,58.3156989582187));
#49092=CARTESIAN_POINT('Ctrl Pts',(-7.86993795650493,0.833764060819869,
58.3244373562048));
#49093=CARTESIAN_POINT('Ctrl Pts',(-7.88990747454002,0.617024352549807,
58.3331757541909));
#49094=CARTESIAN_POINT('Ctrl Pts',(-7.90090634659527,0.399499564869185,
58.341914152177));
#49095=CARTESIAN_POINT('Ctrl Pts',(-7.90751625250328,0.268775398608426,
58.3471655987057));
#49096=CARTESIAN_POINT('Ctrl Pts',(-7.91088728971183,0.137768043901693,
58.3524170452345));
#49097=CARTESIAN_POINT('Ctrl Pts',(-7.91099722033409,0.00663173176848126,
58.3576684917633));
#49098=CARTESIAN_POINT('',(-7.91099844885794,-0.00350301049124394,60.3576684917633));
#49099=CARTESIAN_POINT('Ctrl Pts',(-7.911,-7.83262343873048E-12,58.3576684917633));
#49100=CARTESIAN_POINT('Ctrl Pts',(-7.91099999999782,-2.20167589667448,
58.4462559274961));
#49101=CARTESIAN_POINT('Ctrl Pts',(-6.94214576671948,-4.38610418339347,
58.5348433632288));
#49102=CARTESIAN_POINT('Ctrl Pts',(-3.67820201487602,-7.34180684107971,
58.7120182346942));
#49103=CARTESIAN_POINT('Ctrl Pts',(-1.40868175871005,-8.08992666571462,
58.800605670427));
#49104=CARTESIAN_POINT('Ctrl Pts',(2.9730927052195,-7.65454228024991,58.9777805418924));
#49105=CARTESIAN_POINT('Ctrl Pts',(5.05102072676162,-6.47444880833785,59.0663679776251));
#49106=CARTESIAN_POINT('Ctrl Pts',(7.66951518848115,-2.93425195367063,59.2435428490906));
#49107=CARTESIAN_POINT('Ctrl Pts',(8.18956872247118,-0.601881960092444,
59.3321302848233));
#49108=CARTESIAN_POINT('Ctrl Pts',(7.32306689761046,3.71537198233028,59.5093051562887));
#49109=CARTESIAN_POINT('Ctrl Pts',(5.9432995884976,5.66643518936969,59.5978925920214));
#49110=CARTESIAN_POINT('Ctrl Pts',(2.16154501637256,7.92205913233156,59.7750674634869));
#49111=CARTESIAN_POINT('Ctrl Pts',(-0.210816529306346,8.20894963712984,
59.8636548992196));
#49112=CARTESIAN_POINT('Ctrl Pts',(-4.4212390857692,6.91982244717519,60.0408297706851));
#49113=CARTESIAN_POINT('Ctrl Pts',(-6.22631625634551,5.35390358803094,60.1294172064178));
#49114=CARTESIAN_POINT('Ctrl Pts',(-7.65317280859673,2.31334857513943,60.2645592586881));
#49115=CARTESIAN_POINT('Ctrl Pts',(-7.91100000000109,1.15702837835847,60.3111138752257));
#49116=CARTESIAN_POINT('Ctrl Pts',(-7.911,-7.43738404196392E-12,60.3576684917633));
#49117=CARTESIAN_POINT('',(-7.91099999260072,-0.000333258038948825,62.3576819008605));
#49118=CARTESIAN_POINT('Ctrl Pts',(-7.91099689771587,-0.0070060209750505,
60.3576684917633));
#49119=CARTESIAN_POINT('Ctrl Pts',(-7.91078925208212,-0.241473484075867,
60.3670821951403));
#49120=CARTESIAN_POINT('Ctrl Pts',(-7.90015416056753,-0.475476672476813,
60.3764958985172));
#49121=CARTESIAN_POINT('Ctrl Pts',(-7.87923780643971,-0.708189656498227,
60.3859096018942));
#49122=CARTESIAN_POINT('Ctrl Pts',(-7.85816685921297,-0.942622625806779,
60.3953928820993));
#49123=CARTESIAN_POINT('Ctrl Pts',(-7.82666220554321,-1.17574623517179,
60.4048761623045));
#49124=CARTESIAN_POINT('Ctrl Pts',(-7.78492189767097,-1.40673808762081,
60.4143594425097));
#49125=CARTESIAN_POINT('Ctrl Pts',(-7.74280977313407,-1.63978758229913,
60.4239271984122));
#49126=CARTESIAN_POINT('Ctrl Pts',(-7.69027887464612,-1.87066716028862,
60.4334949543147));
#49127=CARTESIAN_POINT('Ctrl Pts',(-7.62758081045792,-2.09855473598716,
60.4430627102172));
#49128=CARTESIAN_POINT('Ctrl Pts',(-7.58189647615823,-2.26460280024169,
60.4500341624432));
#49129=CARTESIAN_POINT('Ctrl Pts',(-7.53081522856453,-2.42906283056237,
60.4570056146692));
#49130=CARTESIAN_POINT('Ctrl Pts',(-7.47445012798801,-2.59162425598698,
60.4639770668951));
#49131=CARTESIAN_POINT('Ctrl Pts',(-7.41104955360762,-2.77447654647518,
60.4718186935554));
#49132=CARTESIAN_POINT('Ctrl Pts',(-7.340835215822,-2.95528893057795,60.4796603202158));
#49133=CARTESIAN_POINT('Ctrl Pts',(-7.26395463026879,-3.13350987383104,
60.4875019468761));
#49134=CARTESIAN_POINT('Ctrl Pts',(-7.18716456581266,-3.31152097535113,
60.4953343406118));
#49135=CARTESIAN_POINT('Ctrl Pts',(-7.10372401991034,-3.48694639223469,
60.5031667343475));
#49136=CARTESIAN_POINT('Ctrl Pts',(-7.01383039931391,-3.65924912101652,
60.5109991280833));
#49137=CARTESIAN_POINT('Ctrl Pts',(-6.92402512227369,-3.83138251814048,
60.5188238244817));
#49138=CARTESIAN_POINT('Ctrl Pts',(-6.82777956102114,-4.00039902913049,
60.5266485208802));
#49139=CARTESIAN_POINT('Ctrl Pts',(-6.7253394560609,-4.16578086326567,60.5344732172787));
#49140=CARTESIAN_POINT('Ctrl Pts',(-6.62298009498893,-4.3310323424745,60.5422917462058));
#49141=CARTESIAN_POINT('Ctrl Pts',(-6.5144360989321,-4.49265455325189,60.5501102751329));
#49142=CARTESIAN_POINT('Ctrl Pts',(-6.39999953864532,-4.65015342815048,
60.55792880406));
#49143=CARTESIAN_POINT('Ctrl Pts',(-6.28563092338073,-4.80755879041183,
60.5657426908507));
#49144=CARTESIAN_POINT('Ctrl Pts',(-6.16537691916071,-4.96084540978745,
60.5735565776415));
#49145=CARTESIAN_POINT('Ctrl Pts',(-6.03957349621163,-5.10954723863651,
60.5813704644322));
#49146=CARTESIAN_POINT('Ctrl Pts',(-5.91382030895259,-5.25818968802828,
60.5891812309899));
#49147=CARTESIAN_POINT('Ctrl Pts',(-5.78252234485846,-5.40225072637248,
60.5969919975476));
#49148=CARTESIAN_POINT('Ctrl Pts',(-5.64605663851594,-5.54129636769864,
60.6048027641053));
#49149=CARTESIAN_POINT('Ctrl Pts',(-5.50959635602139,-5.68033648263695,
60.612613220223));
#49150=CARTESIAN_POINT('Ctrl Pts',(-5.36796898031928,-5.81436134035106,
60.6204236763408));
#49151=CARTESIAN_POINT('Ctrl Pts',(-5.22158960635568,-5.94297257126418,
60.6282341324585));
#49152=CARTESIAN_POINT('Ctrl Pts',(-5.0752061955324,-6.07158734902599,60.6360448039735));
#49153=CARTESIAN_POINT('Ctrl Pts',(-4.92407078928556,-6.19478796965872,
60.6438554754885));
#49154=CARTESIAN_POINT('Ctrl Pts',(-4.76863284851574,-6.31221528118748,
60.6516661470034));
#49155=CARTESIAN_POINT('Ctrl Pts',(-4.61316324623443,-6.42966651175527,
60.6594784094921));
#49156=CARTESIAN_POINT('Ctrl Pts',(-4.45338964439313,-6.54134187845383,
60.6672906719807));
#49157=CARTESIAN_POINT('Ctrl Pts',(-4.2897919745336,-6.64692453810235,60.6751029344693));
#49158=CARTESIAN_POINT('Ctrl Pts',(-4.12613216709922,-6.7525473000972,60.6829181642071));
#49159=CARTESIAN_POINT('Ctrl Pts',(-3.95864569386522,-6.85207255478377,
60.6907333939448));
#49160=CARTESIAN_POINT('Ctrl Pts',(-3.78783877802627,-6.94522846216598,
60.6985486236826));
#49161=CARTESIAN_POINT('Ctrl Pts',(-3.61684610137414,-7.03848568111994,
60.7063723528621));
#49162=CARTESIAN_POINT('Ctrl Pts',(-3.44252607862198,-7.12535954905826,
60.7141960820416));
#49163=CARTESIAN_POINT('Ctrl Pts',(-3.26540764991057,-7.2056251553842,60.7220198112211));
#49164=CARTESIAN_POINT('Ctrl Pts',(-3.08818175926735,-7.28593946074827,
60.7298482872418));
#49165=CARTESIAN_POINT('Ctrl Pts',(-2.90815440362756,-7.35963738128823,
60.7376767632625));
#49166=CARTESIAN_POINT('Ctrl Pts',(-2.72587159942505,-7.42654327553862,
60.7455052392832));
#49167=CARTESIAN_POINT('Ctrl Pts',(-2.54333792299625,-7.49354125105097,
60.7533444894809));
#49168=CARTESIAN_POINT('Ctrl Pts',(-2.35854293136561,-7.55372842099553,
60.7611837396787));
#49169=CARTESIAN_POINT('Ctrl Pts',(-2.17204591570938,-7.60697952804201,
60.7690229898764));
#49170=CARTESIAN_POINT('Ctrl Pts',(-2.06748391828869,-7.63683545950584,
60.7734181682983));
#49171=CARTESIAN_POINT('Ctrl Pts',(-1.96238706989977,-7.66451201217708,
60.7778133467202));
#49172=CARTESIAN_POINT('Ctrl Pts',(-1.85685482900996,-7.68999422262347,
60.7822085251421));
#49173=CARTESIAN_POINT('Ctrl Pts',(-1.66693130152836,-7.73585386944991,
60.7901184091998));
#49174=CARTESIAN_POINT('Ctrl Pts',(-1.475051451079,-7.7747352926267,60.7980282932576));
#49175=CARTESIAN_POINT('Ctrl Pts',(-1.28177052722043,-7.80647073366378,
60.8059381773153));
#49176=CARTESIAN_POINT('Ctrl Pts',(-1.08869973213889,-7.83817167295448,
60.8138394620027));
#49177=CARTESIAN_POINT('Ctrl Pts',(-0.894231234931356,-7.86274204905463,
60.82174074669));
#49178=CARTESIAN_POINT('Ctrl Pts',(-0.698934092500138,-7.88006422146045,
60.8296420313773));
#49179=CARTESIAN_POINT('Ctrl Pts',(-0.503812979898112,-7.89737078063705,
60.8375361942922));
#49180=CARTESIAN_POINT('Ctrl Pts',(-0.307865051381116,-7.90744212028735,
60.8454303572072));
#49181=CARTESIAN_POINT('Ctrl Pts',(-0.111668455390341,-7.91021182750947,
60.8533245201221));
#49182=CARTESIAN_POINT('Ctrl Pts',(0.0843877467139504,-7.91297955279118,
60.861213034151));
#49183=CARTESIAN_POINT('Ctrl Pts',(0.280691918259379,-7.9084560504733,60.8691015481799));
#49184=CARTESIAN_POINT('Ctrl Pts',(0.476661619744055,-7.89662679251483,
60.8769900622088));
#49185=CARTESIAN_POINT('Ctrl Pts',(0.672527486035284,-7.88480380232774,
60.8848743964825));
#49186=CARTESIAN_POINT('Ctrl Pts',(0.868058891883867,-7.86568279062602,
60.8927587307562));
#49187=CARTESIAN_POINT('Ctrl Pts',(1.06267394828886,-7.83930131323118,60.9006430650299));
#49188=CARTESIAN_POINT('Ctrl Pts',(1.25722202610392,-7.81292891526827,60.9085246858363));
#49189=CARTESIAN_POINT('Ctrl Pts',(1.45085404158705,-7.77930107796768,60.9164063066427));
#49190=CARTESIAN_POINT('Ctrl Pts',(1.64299349497953,-7.73850718003511,60.9242879274491));
#49191=CARTESIAN_POINT('Ctrl Pts',(1.83513546489242,-7.69771274781001,60.9321696514839));
#49192=CARTESIAN_POINT('Ctrl Pts',(2.02578449446142,-7.64975213068483,60.9400513755187));
#49193=CARTESIAN_POINT('Ctrl Pts',(2.21437397475913,-7.59476588842009,60.9479330995536));
#49194=CARTESIAN_POINT('Ctrl Pts',(2.40297481572181,-7.53977633377402,60.9558152983849));
#49195=CARTESIAN_POINT('Ctrl Pts',(2.58951552864162,-7.4777604066923,60.9636974972163));
#49196=CARTESIAN_POINT('Ctrl Pts',(2.77344434461483,-7.40890865562021,60.9715796960476));
#49197=CARTESIAN_POINT('Ctrl Pts',(2.9574151902524,-7.34004117120056,60.9794636960441));
#49198=CARTESIAN_POINT('Ctrl Pts',(3.13877262644362,-7.26433487113398,60.9873476960406));
#49199=CARTESIAN_POINT('Ctrl Pts',(3.31698433008067,-7.18202867955839,60.9952316960371));
#49200=CARTESIAN_POINT('Ctrl Pts',(3.49526674509232,-7.09968983028511,61.0031188242708));
#49201=CARTESIAN_POINT('Ctrl Pts',(3.67040062743373,-7.01074601604411,61.0110059525044));
#49202=CARTESIAN_POINT('Ctrl Pts',(3.84187752886709,-6.91548248882072,61.0188930807381));
#49203=CARTESIAN_POINT('Ctrl Pts',(4.01353737656521,-6.82011732629645,61.0267886236366));
#49204=CARTESIAN_POINT('Ctrl Pts',(4.18153214850993,-6.7184191509624,61.0346841665351));
#49205=CARTESIAN_POINT('Ctrl Pts',(4.34538076693062,-6.61071758513321,61.0425797094336));
#49206=CARTESIAN_POINT('Ctrl Pts',(4.50932916348269,-6.50295043278221,61.0504800604441));
#49207=CARTESIAN_POINT('Ctrl Pts',(4.66912609253968,-6.38917280111203,61.0583804114547));
#49208=CARTESIAN_POINT('Ctrl Pts',(4.82432274712431,-6.26975526089966,61.0662807624652));
#49209=CARTESIAN_POINT('Ctrl Pts',(4.97972147427797,-6.15018223402939,61.0741914000649));
#49210=CARTESIAN_POINT('Ctrl Pts',(5.1305076981577,-6.02495485036458,61.0821020376646));
#49211=CARTESIAN_POINT('Ctrl Pts',(5.27626787837343,-5.8944820192825,61.0900126752643));
#49212=CARTESIAN_POINT('Ctrl Pts',(5.34031186522947,-5.83715497518498,61.0934884446391));
#49213=CARTESIAN_POINT('Ctrl Pts',(5.40338605588324,-5.77881573223792,61.0969642140139));
#49214=CARTESIAN_POINT('Ctrl Pts',(5.46545780336309,-5.71950102715765,61.1004399833887));
#49215=CARTESIAN_POINT('Ctrl Pts',(5.60671549841262,-5.58451757877156,61.1083498488321));
#49216=CARTESIAN_POINT('Ctrl Pts',(5.74316021425428,-5.44411577413464,61.1162597142756));
#49217=CARTESIAN_POINT('Ctrl Pts',(5.87435065001632,-5.29867204501777,61.1241695797191));
#49218=CARTESIAN_POINT('Ctrl Pts',(6.00539850900617,-5.15338638304439,61.1320708487807));
#49219=CARTESIAN_POINT('Ctrl Pts',(6.1312032329654,-5.00306996473738,61.1399721178423));
#49220=CARTESIAN_POINT('Ctrl Pts',(6.25135822035415,-4.84813793128976,61.1478733869039));
#49221=CARTESIAN_POINT('Ctrl Pts',(6.3714049518872,-4.69334548671999,61.1557675371712));
#49222=CARTESIAN_POINT('Ctrl Pts',(6.48581187689786,-4.53394598196298,61.1636616874385));
#49223=CARTESIAN_POINT('Ctrl Pts',(6.59421057600542,-4.37038990014601,61.1715558377058));
#49224=CARTESIAN_POINT('Ctrl Pts',(6.70253174808528,-4.20695079405837,61.1794443420565));
#49225=CARTESIAN_POINT('Ctrl Pts',(6.80485306569523,-4.03936132005771,61.1873328464072));
#49226=CARTESIAN_POINT('Ctrl Pts',(6.90084743965403,-3.86810361994355,61.195221350758));
#49227=CARTESIAN_POINT('Ctrl Pts',(6.99679098666944,-3.69693659707506,61.2031056783164));
#49228=CARTESIAN_POINT('Ctrl Pts',(7.0864140970039,-3.52210551845024,61.2109900058748));
#49229=CARTESIAN_POINT('Ctrl Pts',(7.16943379640047,-3.34412021898596,61.2188743334333));
#49230=CARTESIAN_POINT('Ctrl Pts',(7.25242495491509,-3.16619610810051,61.2267559504825));
#49231=CARTESIAN_POINT('Ctrl Pts',(7.32881708129936,-2.98512024980436,61.2346375675317));
#49232=CARTESIAN_POINT('Ctrl Pts',(7.39837371244669,-2.80142596028841,61.2425191845809));
#49233=CARTESIAN_POINT('Ctrl Pts',(7.4679312936594,-2.61772916171497,61.2504009092841));
#49234=CARTESIAN_POINT('Ctrl Pts',(7.53065306293866,-2.43141418001852,61.2582826339873));
#49235=CARTESIAN_POINT('Ctrl Pts',(7.58635096178516,-2.24303367888701,61.2661643586905));
#49236=CARTESIAN_POINT('Ctrl Pts',(7.64205223536903,-2.05464176377526,61.2740465609477));
#49237=CARTESIAN_POINT('Ctrl Pts',(7.69072869204972,-1.86418441069174,61.2819287632048));
#49238=CARTESIAN_POINT('Ctrl Pts',(7.73224235045464,-1.67222882221175,61.289810965462));
#49239=CARTESIAN_POINT('Ctrl Pts',(7.77376550969032,-1.48022930270693,61.2976949716428));
#49240=CARTESIAN_POINT('Ctrl Pts',(7.80812253118399,-1.28673120184782,61.3055789778236));
#49241=CARTESIAN_POINT('Ctrl Pts',(7.83522664353816,-1.09231151435374,61.3134629840044));
#49242=CARTESIAN_POINT('Ctrl Pts',(7.86234151982677,-0.897814616407488,
61.3213501211833));
#49243=CARTESIAN_POINT('Ctrl Pts',(7.88219769998987,-0.702395744051026,
61.3292372583623));
#49244=CARTESIAN_POINT('Ctrl Pts',(7.89476029409556,-0.506636850981302,
61.3371243955412));
#49245=CARTESIAN_POINT('Ctrl Pts',(7.90733629761916,-0.310669003233389,
61.3450199515163));
#49246=CARTESIAN_POINT('Ctrl Pts',(7.91260314256511,-0.114360754286667,
61.3529155074914));
#49247=CARTESIAN_POINT('Ctrl Pts',(7.91057806332336,0.0817049818996074,
61.3608110634664));
#49248=CARTESIAN_POINT('Ctrl Pts',(7.90855175027101,0.277890174144436,61.3687114299301));
#49249=CARTESIAN_POINT('Ctrl Pts',(7.89922467226719,0.473832215323574,61.3766117963938));
#49250=CARTESIAN_POINT('Ctrl Pts',(7.88266595834452,0.668953204010979,61.3845121628575));
#49251=CARTESIAN_POINT('Ctrl Pts',(7.86608567692635,0.864328335083012,61.3924228194391));
#49252=CARTESIAN_POINT('Ctrl Pts',(7.84225498728872,1.0588799361571,61.4003334760207));
#49253=CARTESIAN_POINT('Ctrl Pts',(7.81129433698851,1.25203904928371,61.4082441326023));
#49254=CARTESIAN_POINT('Ctrl Pts',(7.79769090364407,1.3369089436435,61.4117199022801));
#49255=CARTESIAN_POINT('Ctrl Pts',(7.78271166383436,1.42151018952133,61.4151956719579));
#49256=CARTESIAN_POINT('Ctrl Pts',(7.76636987437531,1.50579546233731,61.4186714416357));
#49257=CARTESIAN_POINT('Ctrl Pts',(7.7295145903776,1.6958822135001,61.4265102697461));
#49258=CARTESIAN_POINT('Ctrl Pts',(7.68562068403171,1.88490219238425,61.4343490978565));
#49259=CARTESIAN_POINT('Ctrl Pts',(7.63475875621671,2.07228852585065,61.4421879259669));
#49260=CARTESIAN_POINT('Ctrl Pts',(7.58395384383499,2.25946480213964,61.4500179668724));
#49261=CARTESIAN_POINT('Ctrl Pts',(7.52619655453168,2.4450107436099,61.4578480077779));
#49262=CARTESIAN_POINT('Ctrl Pts',(7.46160890470589,2.62836708874803,61.4656780486834));
#49263=CARTESIAN_POINT('Ctrl Pts',(7.39708108610036,2.81155358045593,61.4735008361758));
#49264=CARTESIAN_POINT('Ctrl Pts',(7.32573562359224,2.99255418583702,61.4813236236683));
#49265=CARTESIAN_POINT('Ctrl Pts',(7.24774504098589,3.17082210489086,61.4891464111607));
#49266=CARTESIAN_POINT('Ctrl Pts',(7.16981153455072,3.34895956139493,61.4969634736702));
#49267=CARTESIAN_POINT('Ctrl Pts',(7.08524273430716,3.52436799398476,61.5047805361796));
#49268=CARTESIAN_POINT('Ctrl Pts',(6.99426029815046,3.69651780486936,61.5125975986891));
#49269=CARTESIAN_POINT('Ctrl Pts',(6.90332675437798,3.86857510542941,61.5204104604447));
#49270=CARTESIAN_POINT('Ctrl Pts',(6.80598660427244,4.0373769623895,61.5282233222002));
#49271=CARTESIAN_POINT('Ctrl Pts',(6.70250881419265,4.20241556675085,61.5360361839558));
#49272=CARTESIAN_POINT('Ctrl Pts',(6.59906651483257,4.36739756631958,61.5438463660631));
#49273=CARTESIAN_POINT('Ctrl Pts',(6.48949095637755,4.52861858731441,61.5516565481703));
#49274=CARTESIAN_POINT('Ctrl Pts',(6.37409615292086,4.68559699860322,61.5594667302775));
#49275=CARTESIAN_POINT('Ctrl Pts',(6.25869614508426,4.84258248971942,61.567277264629));
#49276=CARTESIAN_POINT('Ctrl Pts',(6.13747656880136,4.99532469993766,61.5750877989805));
#49277=CARTESIAN_POINT('Ctrl Pts',(6.01079402253949,5.14337206690353,61.582898333332));
#49278=CARTESIAN_POINT('Ctrl Pts',(5.88410132255246,5.29143130000503,61.5907094937051));
#49279=CARTESIAN_POINT('Ctrl Pts',(5.75194500859647,5.43479467224237,61.5985206540783));
#49280=CARTESIAN_POINT('Ctrl Pts',(5.6147210607534,5.57304480602231,61.6063318144514));
#49281=CARTESIAN_POINT('Ctrl Pts',(5.47746194643577,5.71133036925818,61.614144976596));
#49282=CARTESIAN_POINT('Ctrl Pts',(5.33513285896086,5.84449983381412,61.6219581387405));
#49283=CARTESIAN_POINT('Ctrl Pts',(5.18816571862437,5.97217359728356,61.629771300885));
#49284=CARTESIAN_POINT('Ctrl Pts',(5.04113502881494,6.09990256765408,61.6375878414877));
#49285=CARTESIAN_POINT('Ctrl Pts',(4.88946255643335,6.2221308725666,61.6454043820905));
#49286=CARTESIAN_POINT('Ctrl Pts',(4.73361238585418,6.33851992033534,61.6532209226932));
#49287=CARTESIAN_POINT('Ctrl Pts',(4.57758033528857,6.45504479624178,61.6610465853411));
#49288=CARTESIAN_POINT('Ctrl Pts',(4.41736113078819,6.56571659384646,61.668872247989));
#49289=CARTESIAN_POINT('Ctrl Pts',(4.25344777839035,6.67024010036417,61.6766979106369));
#49290=CARTESIAN_POINT('Ctrl Pts',(4.08942758200694,6.77483173865918,61.6845286743029));
#49291=CARTESIAN_POINT('Ctrl Pts',(3.92170874145689,6.87326692191954,61.692359437969));
#49292=CARTESIAN_POINT('Ctrl Pts',(3.75080786426145,6.96529693303842,61.700190201635));
#49293=CARTESIAN_POINT('Ctrl Pts',(3.57966005326413,7.05745991784887,61.7080322799314));
#49294=CARTESIAN_POINT('Ctrl Pts',(3.40532133696547,7.14319909102459,61.7158743582278));
#49295=CARTESIAN_POINT('Ctrl Pts',(3.22832834390742,7.22231383310944,61.7237164365241));
#49296=CARTESIAN_POINT('Ctrl Pts',(3.1291237058251,7.26665767531414,61.7281119243102));
#49297=CARTESIAN_POINT('Ctrl Pts',(3.0290854894646,7.30892127559068,61.7325074120962));
#49298=CARTESIAN_POINT('Ctrl Pts',(2.92831002128822,7.34907622897075,61.7369028998823));
#49299=CARTESIAN_POINT('Ctrl Pts',(2.74680765997869,7.42139758841114,61.7448194238808));
#49300=CARTESIAN_POINT('Ctrl Pts',(2.56236828562723,7.48709311749584,61.7527359478793));
#49301=CARTESIAN_POINT('Ctrl Pts',(2.37551672861666,7.54591553570953,61.7606524718777));
#49302=CARTESIAN_POINT('Ctrl Pts',(2.18888043598011,7.60467018691481,61.7685598755584));
#49303=CARTESIAN_POINT('Ctrl Pts',(1.99983782129082,7.65656739646813,61.7764672792391));
#49304=CARTESIAN_POINT('Ctrl Pts',(1.80893475291605,7.70140740772052,61.7843746829197));
#49305=CARTESIAN_POINT('Ctrl Pts',(1.6182162411962,7.74620406963048,61.7922744420718));
#49306=CARTESIAN_POINT('Ctrl Pts',(1.42564119176957,7.78395704594293,61.8001742012238));
#49307=CARTESIAN_POINT('Ctrl Pts',(1.23177201580282,7.81451589678369,61.8080739603758));
#49308=CARTESIAN_POINT('Ctrl Pts',(1.03805435169923,7.84505086539355,61.8159675457397));
#49309=CARTESIAN_POINT('Ctrl Pts',(0.843044914796897,7.86840285650722,61.8238611311036));
#49310=CARTESIAN_POINT('Ctrl Pts',(0.647318013532443,7.88447210594066,61.8317547164674));
#49311=CARTESIAN_POINT('Ctrl Pts',(0.451707828785264,7.90053177290579,61.8396435947022));
#49312=CARTESIAN_POINT('Ctrl Pts',(0.255381374618466,7.90931732363015,61.8475324729369));
#49313=CARTESIAN_POINT('Ctrl Pts',(0.058920102984681,7.91078058231072,61.8554213511717));
#49314=CARTESIAN_POINT('Ctrl Pts',(-0.137460390642674,7.91224323935048,
61.8633069857755));
#49315=CARTESIAN_POINT('Ctrl Pts',(-0.333975247228655,7.90638960191985,
61.8711926203793));
#49316=CARTESIAN_POINT('Ctrl Pts',(-0.530040690244659,7.89322354090425,
61.8790782549832));
#49317=CARTESIAN_POINT('Ctrl Pts',(-0.726088691952936,7.88005865109617,
61.8869631881081));
#49318=CARTESIAN_POINT('Ctrl Pts',(-0.921687015649926,7.85958265032517,
61.8948481212329));
#49319=CARTESIAN_POINT('Ctrl Pts',(-1.11625416202244,7.83185148261684,61.9027330543578));
#49320=CARTESIAN_POINT('Ctrl Pts',(-1.31082063381719,7.80412041105439,61.9106179601451));
#49321=CARTESIAN_POINT('Ctrl Pts',(-1.5043555940604,7.76913427075128,61.9185028659324));
#49322=CARTESIAN_POINT('Ctrl Pts',(-1.69628481823644,7.72700063513784,61.9263877717197));
#49323=CARTESIAN_POINT('Ctrl Pts',(-1.88824557814089,7.68486007658239,61.9342739730691));
#49324=CARTESIAN_POINT('Ctrl Pts',(-2.07859973958628,7.63556975658473,61.9421601744186));
#49325=CARTESIAN_POINT('Ctrl Pts',(-2.26678514152769,7.57928796933784,61.9500463757681));
#49326=CARTESIAN_POINT('Ctrl Pts',(-2.45503303722391,7.52298749169214,61.9579351960153));
#49327=CARTESIAN_POINT('Ctrl Pts',(-2.64111040837763,7.45969101943708,61.9658240162626));
#49328=CARTESIAN_POINT('Ctrl Pts',(-2.82447183645689,7.38960620365266,61.9737128365099));
#49329=CARTESIAN_POINT('Ctrl Pts',(-3.00801074147592,7.31945355223476,61.9816092924071));
#49330=CARTESIAN_POINT('Ctrl Pts',(-3.18882813050841,7.24249955629964,61.9895057483043));
#49331=CARTESIAN_POINT('Ctrl Pts',(-3.36639912302167,7.15899978659861,61.9974022042014));
#49332=CARTESIAN_POINT('Ctrl Pts',(-3.54406825920082,7.07545386649101,62.0053030244777));
#49333=CARTESIAN_POINT('Ctrl Pts',(-3.71848711581281,6.98535511714533,62.013203844754));
#49334=CARTESIAN_POINT('Ctrl Pts',(-3.88915663111816,6.88900440547323,62.0211046650303));
#49335=CARTESIAN_POINT('Ctrl Pts',(-4.06003353299557,6.79253661463927,62.0290150858732));
#49336=CARTESIAN_POINT('Ctrl Pts',(-4.22715170019501,6.68980186659931,62.036925506716));
#49337=CARTESIAN_POINT('Ctrl Pts',(-4.39004128030048,6.58114416779162,62.0448359275588));
#49338=CARTESIAN_POINT('Ctrl Pts',(-4.46072892405258,6.53399101840499,62.048268737749));
#49339=CARTESIAN_POINT('Ctrl Pts',(-4.53062065254584,6.48572296513387,62.0517015479392));
#49340=CARTESIAN_POINT('Ctrl Pts',(-4.59968007684202,6.43637042056333,62.0551343581294));
#49341=CARTESIAN_POINT('Ctrl Pts',(-4.76694906485711,6.31683351057001,62.0634489754668));
#49342=CARTESIAN_POINT('Ctrl Pts',(-4.9296995827341,6.19066978758528,62.0717635928043));
#49343=CARTESIAN_POINT('Ctrl Pts',(-5.08740474275343,6.05823687085689,62.0800782101417));
#49344=CARTESIAN_POINT('Ctrl Pts',(-5.244914987101,5.9259676345745,62.0883825510289));
#49345=CARTESIAN_POINT('Ctrl Pts',(-5.39739208704405,5.78744484600442,62.0966868919161));
#49346=CARTESIAN_POINT('Ctrl Pts',(-5.54433962944533,5.64306823220861,62.1049912328033));
#49347=CARTESIAN_POINT('Ctrl Pts',(-5.69111526575402,5.49886051691313,62.113285858885));
#49348=CARTESIAN_POINT('Ctrl Pts',(-5.83237403816444,5.34881283986969,62.1215804849667));
#49349=CARTESIAN_POINT('Ctrl Pts',(-5.96765339521192,5.19336441573434,62.1298751110484));
#49350=CARTESIAN_POINT('Ctrl Pts',(-6.10272906282565,5.03815004949357,62.1381572479542));
#49351=CARTESIAN_POINT('Ctrl Pts',(-6.23184309027495,4.87755138508124,62.14643938486));
#49352=CARTESIAN_POINT('Ctrl Pts',(-6.35457045289099,4.71204364997236,62.1547215217658));
#49353=CARTESIAN_POINT('Ctrl Pts',(-6.47718463692134,4.54668854530368,62.1629960209246));
#49354=CARTESIAN_POINT('Ctrl Pts',(-6.59342372711044,4.37643363246062,62.1712705200834));
#49355=CARTESIAN_POINT('Ctrl Pts',(-6.70290243281007,4.20178771194225,62.1795450192422));
#49356=CARTESIAN_POINT('Ctrl Pts',(-6.81225522067375,4.02734266186921,62.1878100014176));
#49357=CARTESIAN_POINT('Ctrl Pts',(-6.9148629842122,3.8485169296869,62.196074983593));
#49358=CARTESIAN_POINT('Ctrl Pts',(-7.01038313183886,3.66584906192675,62.2043399657683));
#49359=CARTESIAN_POINT('Ctrl Pts',(-7.04856092206612,3.5928397993797,62.2076433395964));
#49360=CARTESIAN_POINT('Ctrl Pts',(-7.08560696786961,3.51921710218892,62.2109467134245));
#49361=CARTESIAN_POINT('Ctrl Pts',(-7.12150134325963,3.44501663536641,62.2142500872526));
#49362=CARTESIAN_POINT('Ctrl Pts',(-7.20926811728443,3.26358610388664,62.2223272988251));
#49363=CARTESIAN_POINT('Ctrl Pts',(-7.29006283849697,3.07887174248909,62.2304045103976));
#49364=CARTESIAN_POINT('Ctrl Pts',(-7.36365968952011,2.89144202378961,62.2384817219701));
#49365=CARTESIAN_POINT('Ctrl Pts',(-7.43730034680104,2.70390074332546,62.2465637412539));
#49366=CARTESIAN_POINT('Ctrl Pts',(-7.503734470668,2.51364117971434,62.2546457605377));
#49367=CARTESIAN_POINT('Ctrl Pts',(-7.56278562785052,2.32124848889076,62.2627277798215));
#49368=CARTESIAN_POINT('Ctrl Pts',(-7.62191733429708,2.12859336308041,62.2708208234567));
#49369=CARTESIAN_POINT('Ctrl Pts',(-7.67364585089429,1.93379960118771,62.2789138670918));
#49370=CARTESIAN_POINT('Ctrl Pts',(-7.71784514141328,1.73746579050163,62.287006910727));
#49371=CARTESIAN_POINT('Ctrl Pts',(-7.7620756290831,1.54099340167475,62.2951056666689));
#49372=CARTESIAN_POINT('Ctrl Pts',(-7.79876622757874,1.34297910977914,62.3032044226107));
#49373=CARTESIAN_POINT('Ctrl Pts',(-7.82784252260321,1.14402903867208,62.3113031785526));
#49374=CARTESIAN_POINT('Ctrl Pts',(-7.85696518990773,0.944761672379959,
62.3194148507817));
#49375=CARTESIAN_POINT('Ctrl Pts',(-7.8784492406051,0.744555862049014,62.3275265230108));
#49376=CARTESIAN_POINT('Ctrl Pts',(-7.89227223078456,0.544022090715932,
62.3356381952399));
#49377=CARTESIAN_POINT('Ctrl Pts',(-7.90477176190875,0.362688089628877,
62.3429732289903));
#49378=CARTESIAN_POINT('Ctrl Pts',(-7.91100766955499,0.181086106885633,
62.3503082627406));
#49379=CARTESIAN_POINT('Ctrl Pts',(-7.91099999291779,-0.00033474584610353,
62.3576432964909));
#49380=CARTESIAN_POINT('',(-7.911,-7.32081062437828E-12,64.3576684917633));
#49381=CARTESIAN_POINT('Ctrl Pts',(-7.91099999260071,-0.000333258038948825,
62.3576819008605));
#49382=CARTESIAN_POINT('Ctrl Pts',(-7.91090223079165,-2.20189632652019,
62.4462648668942));
#49383=CARTESIAN_POINT('Ctrl Pts',(-6.94206342521017,-4.38617874871575,
62.5348478329279));
#49384=CARTESIAN_POINT('Ctrl Pts',(-3.67820201487601,-7.34180684107976,
62.7120182346942));
#49385=CARTESIAN_POINT('Ctrl Pts',(-1.40868175870985,-8.08992666571469,
62.800605670427));
#49386=CARTESIAN_POINT('Ctrl Pts',(2.97309270521997,-7.65454228024977,62.9777805418924));
#49387=CARTESIAN_POINT('Ctrl Pts',(5.05102072676217,-6.47444880833747,63.0663679776251));
#49388=CARTESIAN_POINT('Ctrl Pts',(7.66951518848153,-2.93425195366975,63.2435428490906));
#49389=CARTESIAN_POINT('Ctrl Pts',(8.1895687224713,-0.601881960091314,63.3321302848233));
#49390=CARTESIAN_POINT('Ctrl Pts',(7.32306689760985,3.71537198233157,63.5093051562888));
#49391=CARTESIAN_POINT('Ctrl Pts',(5.94329958849653,5.66643518937088,63.5978925920215));
#49392=CARTESIAN_POINT('Ctrl Pts',(2.16154501637074,7.92205913233209,63.775067463487));
#49393=CARTESIAN_POINT('Ctrl Pts',(-0.210816529308416,8.20894963712982,
63.8636548992197));
#49394=CARTESIAN_POINT('Ctrl Pts',(-4.42123908577121,6.91982244717395,64.0408297706851));
#49395=CARTESIAN_POINT('Ctrl Pts',(-6.22631625634719,5.35390358802904,64.1294172064179));
#49396=CARTESIAN_POINT('Ctrl Pts',(-7.65317280859711,2.31334857513774,64.2645592586882));
#49397=CARTESIAN_POINT('Ctrl Pts',(-7.91100000000107,1.15702837835769,64.3111138752258));
#49398=CARTESIAN_POINT('Ctrl Pts',(-7.911,-7.32081062437828E-12,64.3576684917633));
#49399=CARTESIAN_POINT('',(-7.9109999940852,0.000305915063436288,66.3576880390319));
#49400=CARTESIAN_POINT('Ctrl Pts',(-7.911,-7.32081062437828E-12,64.3576684917633));
#49401=CARTESIAN_POINT('Ctrl Pts',(-7.91099999999796,-2.20167589667412,
64.4462559274961));
#49402=CARTESIAN_POINT('Ctrl Pts',(-6.94214576671962,-4.38610418339331,
64.5348433632288));
#49403=CARTESIAN_POINT('Ctrl Pts',(-3.67820201487596,-7.34180684107979,
64.7120182346942));
#49404=CARTESIAN_POINT('Ctrl Pts',(-1.4086817587098,-8.0899266657147,64.800605670427));
#49405=CARTESIAN_POINT('Ctrl Pts',(2.97309270522002,-7.65454228024975,64.9777805418924));
#49406=CARTESIAN_POINT('Ctrl Pts',(5.05102072676222,-6.47444880833743,65.0663679776251));
#49407=CARTESIAN_POINT('Ctrl Pts',(7.66951518848155,-2.93425195366969,65.2435428490906));
#49408=CARTESIAN_POINT('Ctrl Pts',(8.1895687224713,-0.601881960091258,65.3321302848233));
#49409=CARTESIAN_POINT('Ctrl Pts',(7.32306689760982,3.71537198233162,65.5093051562888));
#49410=CARTESIAN_POINT('Ctrl Pts',(5.94329958849649,5.66643518937092,65.5978925920215));
#49411=CARTESIAN_POINT('Ctrl Pts',(2.16154501637069,7.92205913233211,65.775067463487));
#49412=CARTESIAN_POINT('Ctrl Pts',(-0.210816529308472,8.20894963712982,
65.8636548992197));
#49413=CARTESIAN_POINT('Ctrl Pts',(-4.42123908577125,6.91982244717392,66.0408297706851));
#49414=CARTESIAN_POINT('Ctrl Pts',(-6.22631625634723,5.353903588029,66.1294172064179));
#49415=CARTESIAN_POINT('Ctrl Pts',(-7.65312966182839,2.31344051859464,66.2645551721226));
#49416=CARTESIAN_POINT('Ctrl Pts',(-7.91095473404371,1.15723138115899,66.3111057020946));
#49417=CARTESIAN_POINT('Ctrl Pts',(-7.91099999404008,0.000304691929376763,
66.3576562320666));
#49418=CARTESIAN_POINT('',(-7.91099954886372,-0.00267168074885584,68.3574023474442));
#49419=CARTESIAN_POINT('Ctrl Pts',(-7.9109999940852,0.000305915063436288,
66.3576880390319));
#49420=CARTESIAN_POINT('Ctrl Pts',(-7.91100793685849,-0.2050951487285,66.3659089648299));
#49421=CARTESIAN_POINT('Ctrl Pts',(-7.90301201333921,-0.410360118679733,
66.3741298906278));
#49422=CARTESIAN_POINT('Ctrl Pts',(-7.88706988155102,-0.614857449764415,
66.3823508164258));
#49423=CARTESIAN_POINT('Ctrl Pts',(-7.8711114624684,-0.819563705746012,
66.3905801411405));
#49424=CARTESIAN_POINT('Ctrl Pts',(-7.84719065175379,-1.02350045984394,
66.3988094658553));
#49425=CARTESIAN_POINT('Ctrl Pts',(-7.81541669025749,-1.22604361979689,
66.40703879057));
#49426=CARTESIAN_POINT('Ctrl Pts',(-7.78216777393996,-1.43798888122569,
66.4156501224879));
#49427=CARTESIAN_POINT('Ctrl Pts',(-7.74031937245779,-1.64840771187476,
66.4242614544058));
#49428=CARTESIAN_POINT('Ctrl Pts',(-7.6900554697985,-1.85660116110655,66.4328727863237));
#49429=CARTESIAN_POINT('Ctrl Pts',(-7.64187765064024,-2.05615403735281,
66.4411267254311));
#49430=CARTESIAN_POINT('Ctrl Pts',(-7.58596885857615,-2.2536622577624,66.4493806645385));
#49431=CARTESIAN_POINT('Ctrl Pts',(-7.52254125280714,-2.44852896650516,
66.457634603646));
#49432=CARTESIAN_POINT('Ctrl Pts',(-7.45904666143902,-2.64360147307165,
66.4658972597001));
#49433=CARTESIAN_POINT('Ctrl Pts',(-7.38801750594898,-2.83602661913333,
66.4741599157542));
#49434=CARTESIAN_POINT('Ctrl Pts',(-7.30971382302372,-3.02522806173286,
66.4824225718082));
#49435=CARTESIAN_POINT('Ctrl Pts',(-7.23128197129088,-3.21473919248989,
66.4906987523191));
#49436=CARTESIAN_POINT('Ctrl Pts',(-7.14555191693428,-3.4010158024365,66.49897493283));
#49437=CARTESIAN_POINT('Ctrl Pts',(-7.05283007982976,-3.58350510883528,
66.5072511133408));
#49438=CARTESIAN_POINT('Ctrl Pts',(-7.04116481483934,-3.60646395201113,
66.5082923334221));
#49439=CARTESIAN_POINT('Ctrl Pts',(-7.02938894070794,-3.62936288698674,
66.5093335535034));
#49440=CARTESIAN_POINT('Ctrl Pts',(-7.01750311600732,-3.65220084563096,
66.5103747735847));
#49441=CARTESIAN_POINT('Ctrl Pts',(-6.92258938364662,-3.83457236372255,
66.518689390922));
#49442=CARTESIAN_POINT('Ctrl Pts',(-6.82048096715838,-4.01339878052998,
66.5270040082594));
#49443=CARTESIAN_POINT('Ctrl Pts',(-6.71145811088942,-4.18810828725531,
66.5353186255967));
#49444=CARTESIAN_POINT('Ctrl Pts',(-6.6025700014052,-4.36260186178899,66.5436229664839));
#49445=CARTESIAN_POINT('Ctrl Pts',(-6.48678465096934,-4.53298842694055,
66.551927307371));
#49446=CARTESIAN_POINT('Ctrl Pts',(-6.36442826724767,-4.69872044614902,
66.5602316482582));
#49447=CARTESIAN_POINT('Ctrl Pts',(-6.24221502173409,-4.86425858430666,
66.5685262743398));
#49448=CARTESIAN_POINT('Ctrl Pts',(-6.11344624863497,-5.02515280186179,
66.5768209004215));
#49449=CARTESIAN_POINT('Ctrl Pts',(-5.97849199928957,-5.18088355538229,
66.5851155265031));
#49450=CARTESIAN_POINT('Ctrl Pts',(-5.84374094986418,-5.33637982590716,
66.5933976634088));
#49451=CARTESIAN_POINT('Ctrl Pts',(-5.7028232020138,-5.48672792677824,66.6016798003146));
#49452=CARTESIAN_POINT('Ctrl Pts',(-5.55614972395224,-5.63144042364167,
66.6099619372203));
#49453=CARTESIAN_POINT('Ctrl Pts',(-5.40961150747035,-5.77601946733291,
66.618236436379));
#49454=CARTESIAN_POINT('Ctrl Pts',(-5.2573283535909,-5.91497306562621,66.6265109355377));
#49455=CARTESIAN_POINT('Ctrl Pts',(-5.09975004103882,-6.04784842063065,
66.6347854346964));
#49456=CARTESIAN_POINT('Ctrl Pts',(-4.94235296848039,-6.18057094795145,
66.6430504168718));
#49457=CARTESIAN_POINT('Ctrl Pts',(-4.77967311367969,-6.30722899337593,
66.6513153990472));
#49458=CARTESIAN_POINT('Ctrl Pts',(-4.61219569221497,-6.42740786761768,
66.6595803812226));
#49459=CARTESIAN_POINT('Ctrl Pts',(-4.54525779456572,-6.47544133453663,
66.6628837550511));
#49460=CARTESIAN_POINT('Ctrl Pts',(-4.47755389912394,-6.52244020255479,
66.6661871288795));
#49461=CARTESIAN_POINT('Ctrl Pts',(-4.40911652618476,-6.56837974378191,
66.669490502708));
#49462=CARTESIAN_POINT('Ctrl Pts',(-4.23786450353326,-6.68333505280314,
66.6777565922057));
#49463=CARTESIAN_POINT('Ctrl Pts',(-4.06221137484325,-6.79152428198379,
66.6860226817034));
#49464=CARTESIAN_POINT('Ctrl Pts',(-3.88271586641192,-6.89263654204348,
66.694288771201));
#49465=CARTESIAN_POINT('Ctrl Pts',(-3.70305893742194,-6.9938397324983,66.7025622944044));
#49466=CARTESIAN_POINT('Ctrl Pts',(-3.51955298617807,-7.08795310408813,
66.7108358176078));
#49467=CARTESIAN_POINT('Ctrl Pts',(-3.33277978190764,-7.17471253259026,
66.7191093408112));
#49468=CARTESIAN_POINT('Ctrl Pts',(-3.14582646382379,-7.26155562711706,
66.7273908425456));
#49469=CARTESIAN_POINT('Ctrl Pts',(-2.95559986852891,-7.34103049676887,
66.7356723442801));
#49470=CARTESIAN_POINT('Ctrl Pts',(-2.76270087022072,-7.41292148222829,
66.7439538460145));
#49471=CARTESIAN_POINT('Ctrl Pts',(-2.56948069923837,-7.48493216462887,
66.7522491362708));
#49472=CARTESIAN_POINT('Ctrl Pts',(-2.37357950522289,-7.54933361541845,
66.7605444265272));
#49473=CARTESIAN_POINT('Ctrl Pts',(-2.17561438137431,-7.60595970693753,
66.7688397167835));
#49474=CARTESIAN_POINT('Ctrl Pts',(-1.97746972180394,-7.66263715298824,
66.7771425300868));
#49475=CARTESIAN_POINT('Ctrl Pts',(-1.77725767987169,-7.7115250900311,66.7854453433901));
#49476=CARTESIAN_POINT('Ctrl Pts',(-1.57560590028026,-7.75250843579045,
66.7937481566934));
#49477=CARTESIAN_POINT('Ctrl Pts',(-1.37364488378663,-7.79355463030278,
66.8020637025214));
#49478=CARTESIAN_POINT('Ctrl Pts',(-1.17024000542739,-7.8266719515452,66.8103792483493));
#49479=CARTESIAN_POINT('Ctrl Pts',(-0.966026280522799,-7.85179687876217,
66.8186947941773));
#49480=CARTESIAN_POINT('Ctrl Pts',(-0.884891033184819,-7.86177915191765,
66.8219986067287));
#49481=CARTESIAN_POINT('Ctrl Pts',(-0.803628133299662,-7.87050038989894,
66.8253024192801));
#49482=CARTESIAN_POINT('Ctrl Pts',(-0.722277443167851,-7.8779588914319,
66.8286062318315));
#49483=CARTESIAN_POINT('Ctrl Pts',(-0.52751463616729,-7.89581539261491,
66.8365159349363));
#49484=CARTESIAN_POINT('Ctrl Pts',(-0.331842449390223,-7.90646769815302,
66.8444256380411));
#49485=CARTESIAN_POINT('Ctrl Pts',(-0.135835962244705,-7.90983372716273,
66.8523353411458));
#49486=CARTESIAN_POINT('Ctrl Pts',(0.0599716667651551,-7.91319634117193,
66.8602370194712));
#49487=CARTESIAN_POINT('Ctrl Pts',(0.256112578798345,-7.90928739768237,
66.8681386977966));
#49488=CARTESIAN_POINT('Ctrl Pts',(0.452005680182568,-7.89807646614558,
66.876040376122));
#49489=CARTESIAN_POINT('Ctrl Pts',(0.647736328092416,-7.88687483179571,
66.8839355016128));
#49490=CARTESIAN_POINT('Ctrl Pts',(0.843219232633905,-7.86838329254936,
66.8918306271036));
#49491=CARTESIAN_POINT('Ctrl Pts',(1.03787211072146,-7.84262344383476,66.8997257525944));
#49492=CARTESIAN_POINT('Ctrl Pts',(1.23239961387978,-7.81688018690777,66.907615792875));
#49493=CARTESIAN_POINT('Ctrl Pts',(1.42609781534182,-7.78387799302661,66.9155058331556));
#49494=CARTESIAN_POINT('Ctrl Pts',(1.61838808196957,-7.74369040032844,66.9233958734362));
#49495=CARTESIAN_POINT('Ctrl Pts',(1.81059010084316,-7.70352125091845,66.9312822927414));
#49496=CARTESIAN_POINT('Ctrl Pts',(2.00138513582339,-7.65617334422175,66.9391687120465));
#49497=CARTESIAN_POINT('Ctrl Pts',(2.190203013785,-7.60177161972176,66.9470551313516));
#49498=CARTESIAN_POINT('Ctrl Pts',(2.37896919496613,-7.54738478996604,66.9549393914201));
#49499=CARTESIAN_POINT('Ctrl Pts',(2.56575896727935,-7.4859480870699,66.9628236514886));
#49500=CARTESIAN_POINT('Ctrl Pts',(2.75001535489471,-7.41763685737198,66.9707079115571));
#49501=CARTESIAN_POINT('Ctrl Pts',(2.93429325434585,-7.34931765237414,66.9785930921087));
#49502=CARTESIAN_POINT('Ctrl Pts',(3.11603685255183,-7.27412243024097,66.9864782726603));
#49503=CARTESIAN_POINT('Ctrl Pts',(3.29470666243988,-7.19227564881062,66.994363453212));
#49504=CARTESIAN_POINT('Ctrl Pts',(3.47339875772641,-7.11041865867104,67.0022496172784));
#49505=CARTESIAN_POINT('Ctrl Pts',(3.64901598693531,-7.02190859902328,67.0101357813448));
#49506=CARTESIAN_POINT('Ctrl Pts',(3.82104112217347,-6.92701708837645,67.0180219454112));
#49507=CARTESIAN_POINT('Ctrl Pts',(3.99311657685187,-6.83209782081088,67.0259104162763));
#49508=CARTESIAN_POINT('Ctrl Pts',(4.16159754186321,-6.73079354888768,67.0337988871415));
#49509=CARTESIAN_POINT('Ctrl Pts',(4.3259933504383,-6.62342075758166,67.0416873580066));
#49510=CARTESIAN_POINT('Ctrl Pts',(4.49046483016038,-6.51599854273897,67.0495794599231));
#49511=CARTESIAN_POINT('Ctrl Pts',(4.6508471180396,-6.40250243043345,67.0574715618397));
#49512=CARTESIAN_POINT('Ctrl Pts',(4.80668016985543,-6.28329107591862,67.0653636637563));
#49513=CARTESIAN_POINT('Ctrl Pts',(4.96269387919311,-6.16394151947787,67.073264915));
#49514=CARTESIAN_POINT('Ctrl Pts',(5.11414754425515,-6.03886369579897,67.0811661662437));
#49515=CARTESIAN_POINT('Ctrl Pts',(5.26061485798518,-5.90845600101631,67.0890674174874));
#49516=CARTESIAN_POINT('Ctrl Pts',(5.40717922524051,-5.77796189428149,67.0969739043313));
#49517=CARTESIAN_POINT('Ctrl Pts',(5.54875040633782,-5.64213111356376,67.1048803911752));
#49518=CARTESIAN_POINT('Ctrl Pts',(5.68494020387709,-5.50139762954305,67.112786878019));
#49519=CARTESIAN_POINT('Ctrl Pts',(5.82131762546363,-5.3604702617929,67.1207042573606));
#49520=CARTESIAN_POINT('Ctrl Pts',(5.95229862564975,-5.21462695504968,67.1286216367022));
#49521=CARTESIAN_POINT('Ctrl Pts',(6.07753565096896,-5.06433425152817,67.1365390160438));
#49522=CARTESIAN_POINT('Ctrl Pts',(6.13183709109418,-4.99916893623319,67.1399719073886));
#49523=CARTESIAN_POINT('Ctrl Pts',(6.1850592202821,-4.93316750144315,67.1434047987334));
#49524=CARTESIAN_POINT('Ctrl Pts',(6.23717630797825,-4.86636956089391,67.1468376900782));
#49525=CARTESIAN_POINT('Ctrl Pts',(6.35622544274216,-4.71378549724167,67.1546793167385));
#49526=CARTESIAN_POINT('Ctrl Pts',(6.46985956898129,-4.55658989670021,67.1625209433989));
#49527=CARTESIAN_POINT('Ctrl Pts',(6.57769584434812,-4.39520629541385,67.1703625700592));
#49528=CARTESIAN_POINT('Ctrl Pts',(6.68540515062556,-4.23401271115865,67.178194963795));
#49529=CARTESIAN_POINT('Ctrl Pts',(6.78733000555567,-4.06864123376018,67.1860273575307));
#49530=CARTESIAN_POINT('Ctrl Pts',(6.88312687573189,-3.89954938583643,67.1938597512665));
#49531=CARTESIAN_POINT('Ctrl Pts',(6.97882960089393,-3.73062371405594,67.201684447665));
#49532=CARTESIAN_POINT('Ctrl Pts',(7.0684161621868,-3.55798525633578,67.2095091440634));
#49533=CARTESIAN_POINT('Ctrl Pts',(7.1515854191098,-3.38212167036849,67.2173338404619));
#49534=CARTESIAN_POINT('Ctrl Pts',(7.23468912153964,-3.20639670110487,67.2251523693891));
#49535=CARTESIAN_POINT('Ctrl Pts',(7.31138544418473,-3.02745198285435,67.2329708983163));
#49536=CARTESIAN_POINT('Ctrl Pts',(7.38141833725328,-2.84580117549717,67.2407894272434));
#49537=CARTESIAN_POINT('Ctrl Pts',(7.45140964932264,-2.66425822063245,67.2486033140341));
#49538=CARTESIAN_POINT('Ctrl Pts',(7.51474528652795,-2.48001270434945,67.2564172008249));
#49539=CARTESIAN_POINT('Ctrl Pts',(7.57121657576523,-2.29359991342385,67.2642310876156));
#49540=CARTESIAN_POINT('Ctrl Pts',(7.62766531494716,-2.10726156065625,67.2720418541733));
#49541=CARTESIAN_POINT('Ctrl Pts',(7.67725506553332,-1.91875799363098,67.2798526207311));
#49542=CARTESIAN_POINT('Ctrl Pts',(7.71982638358571,-1.72864154968404,67.2876633872888));
#49543=CARTESIAN_POINT('Ctrl Pts',(7.76239600963511,-1.53853266194172,67.2954738434065));
#49544=CARTESIAN_POINT('Ctrl Pts',(7.79794767318894,-1.34681136617057,67.3032842995243));
#49545=CARTESIAN_POINT('Ctrl Pts',(7.82637251123595,-1.15404259686128,67.311094755642));
#49546=CARTESIAN_POINT('Ctrl Pts',(7.85479813318496,-0.961268511362553,
67.318905427157));
#49547=CARTESIAN_POINT('Ctrl Pts',(7.87609648597023,-0.767447242884585,
67.326716098672));
#49548=CARTESIAN_POINT('Ctrl Pts',(7.89021030313044,-0.573151264828211,
67.334526770187));
#49549=CARTESIAN_POINT('Ctrl Pts',(7.90432699516657,-0.378815710176739,
67.3423390326756));
#49550=CARTESIAN_POINT('Ctrl Pts',(7.91125621081637,-0.184005604321285,
67.3501512951642));
#49551=CARTESIAN_POINT('Ctrl Pts',(7.91099275847185,0.0107039901909737,
67.3579635576529));
#49552=CARTESIAN_POINT('Ctrl Pts',(7.910729206063,0.205487539190638,67.3657787873906));
#49553=CARTESIAN_POINT('Ctrl Pts',(7.90326754433039,0.400170149202142,67.3735940171284));
#49554=CARTESIAN_POINT('Ctrl Pts',(7.8886546475695,0.594179140815355,67.3814092468662));
#49555=CARTESIAN_POINT('Ctrl Pts',(7.87402585857392,0.788399126626365,67.3892329760457));
#49556=CARTESIAN_POINT('Ctrl Pts',(7.85223032742534,0.981943679856485,67.3970567052252));
#49557=CARTESIAN_POINT('Ctrl Pts',(7.82336666886793,1.17424655181365,67.4048804344047));
#49558=CARTESIAN_POINT('Ctrl Pts',(7.79448549804766,1.36666609846189,67.4127089104254));
#49559=CARTESIAN_POINT('Ctrl Pts',(7.75852771829795,1.55784211773711,67.4205373864461));
#49560=CARTESIAN_POINT('Ctrl Pts',(7.71564258387514,1.7472207982658,67.4283658624667));
#49561=CARTESIAN_POINT('Ctrl Pts',(7.67269842748793,1.93686011693613,67.4362051126645));
#49562=CARTESIAN_POINT('Ctrl Pts',(7.6228079637375,2.12469681724964,67.4440443628623));
#49563=CARTESIAN_POINT('Ctrl Pts',(7.56616995667815,2.31019332235661,67.4518836130601));
#49564=CARTESIAN_POINT('Ctrl Pts',(7.53441511530983,2.41419437041388,67.4562787914818));
#49565=CARTESIAN_POINT('Ctrl Pts',(7.50054009812716,2.51746015525612,67.4606739699035));
#49566=CARTESIAN_POINT('Ctrl Pts',(7.46458638868163,2.61989905261806,67.4650691483252));
#49567=CARTESIAN_POINT('Ctrl Pts',(7.39988146754456,2.80425557319383,67.472979032383));
#49568=CARTESIAN_POINT('Ctrl Pts',(7.32825542580156,2.9864624671935,67.4808889164408));
#49569=CARTESIAN_POINT('Ctrl Pts',(7.24986915251191,3.16596245578753,67.4887988004985));
#49570=CARTESIAN_POINT('Ctrl Pts',(7.17156809824657,3.34526729779213,67.4967000851859));
#49571=CARTESIAN_POINT('Ctrl Pts',(7.08652158824193,3.5218707828198,67.5046013698732));
#49572=CARTESIAN_POINT('Ctrl Pts',(6.99494008734091,3.69523127483398,67.5125026545605));
#49573=CARTESIAN_POINT('Ctrl Pts',(6.90344113283932,3.86843550947874,67.5203968174754));
#49574=CARTESIAN_POINT('Ctrl Pts',(6.80541908140425,4.03840227095019,67.5282909803904));
#49575=CARTESIAN_POINT('Ctrl Pts',(6.70113234262546,4.20461012777868,67.5361851433054));
#49576=CARTESIAN_POINT('Ctrl Pts',(6.59692022909914,4.37069904999071,67.5440736573343));
#49577=CARTESIAN_POINT('Ctrl Pts',(6.48645254216465,4.53303413548696,67.5519621713632));
#49578=CARTESIAN_POINT('Ctrl Pts',(6.3700335793673,4.69111854441274,67.5598506853922));
#49579=CARTESIAN_POINT('Ctrl Pts',(6.25367630154217,4.84911919179195,67.5677350196659));
#49580=CARTESIAN_POINT('Ctrl Pts',(6.13137423526002,5.00287337334444,67.5756193539396));
#49581=CARTESIAN_POINT('Ctrl Pts',(6.00347510220884,5.15191301335325,67.5835036882133));
#49582=CARTESIAN_POINT('Ctrl Pts',(5.87561998684066,5.30090135997584,67.5913853090196));
#49583=CARTESIAN_POINT('Ctrl Pts',(5.7421718682063,5.44517813736502,67.5992669298259));
#49584=CARTESIAN_POINT('Ctrl Pts',(5.60351904371278,5.58430795414689,67.6071485506323));
#49585=CARTESIAN_POINT('Ctrl Pts',(5.46486440323129,5.72343959316408,67.6150302746671));
#49586=CARTESIAN_POINT('Ctrl Pts',(5.3210051581103,5.85742388651197,67.622911998702));
#49587=CARTESIAN_POINT('Ctrl Pts',(5.17236719654218,5.98586155738123,67.6307937227369));
#49588=CARTESIAN_POINT('Ctrl Pts',(5.02372028099649,6.1143069653589,67.6386759215682));
#49589=CARTESIAN_POINT('Ctrl Pts',(4.87029433616513,6.23720485891626,67.6465581203995));
#49590=CARTESIAN_POINT('Ctrl Pts',(4.71254915070054,6.35419558262347,67.6544403192309));
#49591=CARTESIAN_POINT('Ctrl Pts',(4.55476791880469,6.47121303993949,67.6623243192274));
#49592=CARTESIAN_POINT('Ctrl Pts',(4.392665756726,6.58232043204918,67.6702083192239));
#49593=CARTESIAN_POINT('Ctrl Pts',(4.22673249676059,6.68720071486029,67.6780923192205));
#49594=CARTESIAN_POINT('Ctrl Pts',(4.06073339729916,6.79212261238424,67.6859794474542));
#49595=CARTESIAN_POINT('Ctrl Pts',(3.89090046245507,6.89081229309079,67.6938665756878));
#49596=CARTESIAN_POINT('Ctrl Pts',(3.71774944231857,6.98299792955289,67.7017537039215));
#49597=CARTESIAN_POINT('Ctrl Pts',(3.54441368982391,7.07528191755805,67.70964924682));
#49598=CARTESIAN_POINT('Ctrl Pts',(3.36775308580008,7.16104783883787,67.7175447897185));
#49599=CARTESIAN_POINT('Ctrl Pts',(3.18830575535423,7.24007095340751,67.725440332617));
#49600=CARTESIAN_POINT('Ctrl Pts',(3.00874914770108,7.31914219031617,67.7333406836276));
#49601=CARTESIAN_POINT('Ctrl Pts',(2.82640275028521,7.39146230753328,67.7412410346381));
#49602=CARTESIAN_POINT('Ctrl Pts',(2.64182152784425,7.45685590681614,67.7491413856487));
#49603=CARTESIAN_POINT('Ctrl Pts',(2.45699997289216,7.5223346513143,67.7570520232484));
#49604=CARTESIAN_POINT('Ctrl Pts',(2.26993810896296,7.58086876098412,67.7649626608482));
#49605=CARTESIAN_POINT('Ctrl Pts',(2.08120392160856,7.63233327604876,67.7728732984479));
#49606=CARTESIAN_POINT('Ctrl Pts',(1.99827805121023,7.65494571190994,67.7763490678226));
#49607=CARTESIAN_POINT('Ctrl Pts',(1.91502944209998,7.67619400301762,67.7798248371972));
#49608=CARTESIAN_POINT('Ctrl Pts',(1.83150667409454,7.69607070541501,67.7833006065719));
#49609=CARTESIAN_POINT('Ctrl Pts',(1.64143253937006,7.7413044434673,67.7912104720154));
#49610=CARTESIAN_POINT('Ctrl Pts',(1.44942515025329,7.77955349249484,67.799120337459));
#49611=CARTESIAN_POINT('Ctrl Pts',(1.25604031289521,7.81065194029168,67.8070302029025));
#49612=CARTESIAN_POINT('Ctrl Pts',(1.06286564471425,7.84171659053089,67.8149314719642));
#49613=CARTESIAN_POINT('Ctrl Pts',(0.868316847569201,7.86564606426011,67.8228327410258));
#49614=CARTESIAN_POINT('Ctrl Pts',(0.672963367964798,7.88232461304262,67.8307340100875));
#49615=CARTESIAN_POINT('Ctrl Pts',(0.477785895686628,7.8989881349785,67.8386281603548));
#49616=CARTESIAN_POINT('Ctrl Pts',(0.281805526730041,7.90841371673059,67.8465223106221));
#49617=CARTESIAN_POINT('Ctrl Pts',(0.0856006284762027,7.91053686752072,
67.8544164608895));
#49618=CARTESIAN_POINT('Ctrl Pts',(-0.110463943530358,7.91265849982795,
67.8623049652403));
#49619=CARTESIAN_POINT('Ctrl Pts',(-0.306752381366858,7.90748810281787,
67.8701934695911));
#49620=CARTESIAN_POINT('Ctrl Pts',(-0.502682199417825,7.89501308462427,
67.8780819739418));
#49621=CARTESIAN_POINT('Ctrl Pts',(-0.698508276873272,7.88254467168264,
67.8859663015004));
#49622=CARTESIAN_POINT('Ctrl Pts',(-0.893975769459908,7.86277936616138,
67.893850629059));
#49623=CARTESIAN_POINT('Ctrl Pts',(-1.0885029155257,7.83575665796814,67.9017349566175));
#49624=CARTESIAN_POINT('Ctrl Pts',(-1.28296318618163,7.80874323976204,67.9096165736668));
#49625=CARTESIAN_POINT('Ctrl Pts',(-1.47648341333973,7.77447743884248,67.9174981907161));
#49626=CARTESIAN_POINT('Ctrl Pts',(-1.66848739715556,7.73305054978519,67.9253798077654));
#49627=CARTESIAN_POINT('Ctrl Pts',(-1.86049400352918,7.69162309488334,67.9332615324686));
#49628=CARTESIAN_POINT('Ctrl Pts',(-2.05098398619798,7.64303442079796,67.9411432571719));
#49629=CARTESIAN_POINT('Ctrl Pts',(-2.23939120623307,7.5874269700239,67.9490249818752));
#49630=CARTESIAN_POINT('Ctrl Pts',(-2.42780984186723,7.53181614999274,67.9569071841324));
#49631=CARTESIAN_POINT('Ctrl Pts',(-2.61414513217561,7.46918580299793,67.9647893863896));
#49632=CARTESIAN_POINT('Ctrl Pts',(-2.79784594470447,7.39972831053281,67.9726715886468));
#49633=CARTESIAN_POINT('Ctrl Pts',(-2.98158879906702,7.33025492200111,67.9805555948276));
#49634=CARTESIAN_POINT('Ctrl Pts',(-3.16269565143175,7.25395139659806,67.9884396010085));
#49635=CARTESIAN_POINT('Ctrl Pts',(-3.34063497619055,7.17105842647042,67.9963236071893));
#49636=CARTESIAN_POINT('Ctrl Pts',(-3.5186449665065,7.08813253681852,68.0042107443682));
#49637=CARTESIAN_POINT('Ctrl Pts',(-3.6934846101381,6.99861213367762,68.0120978815472));
#49638=CARTESIAN_POINT('Ctrl Pts',(-3.86464641054531,6.90278415724114,68.0199850187261));
#49639=CARTESIAN_POINT('Ctrl Pts',(-4.03599091049004,6.80685389322101,68.0278805747013));
#49640=CARTESIAN_POINT('Ctrl Pts',(-4.20364942462189,6.70460277635662,68.0357761306764));
#49641=CARTESIAN_POINT('Ctrl Pts',(-4.36714197427072,6.59636202588691,68.0436716866516));
#49642=CARTESIAN_POINT('Ctrl Pts',(-4.53073413426365,6.48805532807939,68.0515720531153));
#49643=CARTESIAN_POINT('Ctrl Pts',(-4.6901549899213,6.37375192188635,68.0594724195791));
#49644=CARTESIAN_POINT('Ctrl Pts',(-4.84495696967043,6.25382386720652,68.0673727860428));
#49645=CARTESIAN_POINT('Ctrl Pts',(-4.99996057685379,6.13373960789678,68.0752834426244));
#49646=CARTESIAN_POINT('Ctrl Pts',(-5.15033302757959,6.00801628741753,68.0831940992061));
#49647=CARTESIAN_POINT('Ctrl Pts',(-5.29566214425518,5.87706418664137,68.0911047557877));
#49648=CARTESIAN_POINT('Ctrl Pts',(-5.3595165831028,5.81952669448387,68.0945805254648));
#49649=CARTESIAN_POINT('Ctrl Pts',(-5.4223978937926,5.76098022411872,68.0980562951418));
#49650=CARTESIAN_POINT('Ctrl Pts',(-5.48427355201924,5.70146162020076,68.1015320648189));
#49651=CARTESIAN_POINT('Ctrl Pts',(-5.62176696829789,5.56920579586931,68.1092555454379));
#49652=CARTESIAN_POINT('Ctrl Pts',(-5.75470897477497,5.43174660576841,68.1169790260568));
#49653=CARTESIAN_POINT('Ctrl Pts',(-5.88266780366062,5.28943669134764,68.1247025066757));
#49654=CARTESIAN_POINT('Ctrl Pts',(-6.01048128585462,5.14728842482121,68.1324172142982));
#49655=CARTESIAN_POINT('Ctrl Pts',(-6.13332261708519,5.00030066704751,68.1401319219207));
#49656=CARTESIAN_POINT('Ctrl Pts',(-6.25079385755168,4.84886555293031,68.1478466295431));
#49657=CARTESIAN_POINT('Ctrl Pts',(-6.36815590208531,4.69757120602123,68.1555541659236));
#49658=CARTESIAN_POINT('Ctrl Pts',(-6.48015757249965,4.54183801652948,68.163261702304));
#49659=CARTESIAN_POINT('Ctrl Pts',(-6.58643847852492,4.38209415332514,68.1709692386845));
#49660=CARTESIAN_POINT('Ctrl Pts',(-6.6935537676721,4.22109618354351,68.1787372848828));
#49661=CARTESIAN_POINT('Ctrl Pts',(-6.79485781584916,4.05602455587056,68.1865053310811));
#49662=CARTESIAN_POINT('Ctrl Pts',(-6.89002303352795,3.8873517460418,68.1942733772794));
#49663=CARTESIAN_POINT('Ctrl Pts',(-6.98433017398566,3.72019981011489,68.2019713812537));
#49664=CARTESIAN_POINT('Ctrl Pts',(-7.07260854612563,3.54951168638046,68.209669385228));
#49665=CARTESIAN_POINT('Ctrl Pts',(-7.15458292517099,3.37577608363643,68.2173673892023));
#49666=CARTESIAN_POINT('Ctrl Pts',(-7.23653652760632,3.20208451461256,68.2250634420984));
#49667=CARTESIAN_POINT('Ctrl Pts',(-7.31218916276314,3.02534733151858,68.2327594949945));
#49668=CARTESIAN_POINT('Ctrl Pts',(-7.38131200158983,2.84607697281466,68.2404555478905));
#49669=CARTESIAN_POINT('Ctrl Pts',(-7.4504301815942,2.66681869678507,68.248151082079));
#49670=CARTESIAN_POINT('Ctrl Pts',(-7.51301931185719,2.48502792351462,68.2558466162675));
#49671=CARTESIAN_POINT('Ctrl Pts',(-7.56889907121512,2.30123615688587,68.2635421504559));
#49672=CARTESIAN_POINT('Ctrl Pts',(-7.62569483843707,2.11443158731187,68.2713638335383));
#49673=CARTESIAN_POINT('Ctrl Pts',(-7.6755592219986,1.92556021451917,68.2791855166206));
#49674=CARTESIAN_POINT('Ctrl Pts',(-7.71835601555024,1.73519492196681,68.287007199703));
#49675=CARTESIAN_POINT('Ctrl Pts',(-7.7604946658136,1.54775713003351,68.2947085983482));
#49676=CARTESIAN_POINT('Ctrl Pts',(-7.79578150902447,1.35887140329898,68.3024099969934));
#49677=CARTESIAN_POINT('Ctrl Pts',(-7.82413840397329,1.16909333907534,68.3101113956386));
#49678=CARTESIAN_POINT('Ctrl Pts',(-7.85315963795424,0.97486919654394,68.3179932209396));
#49679=CARTESIAN_POINT('Ctrl Pts',(-7.87492218388578,0.779710795304858,
68.3258750462405));
#49680=CARTESIAN_POINT('Ctrl Pts',(-7.88939866528744,0.584217168663089,
68.3337568715414));
#49681=CARTESIAN_POINT('Ctrl Pts',(-7.9038751466891,0.388723542021395,68.3416386968424));
#49682=CARTESIAN_POINT('Ctrl Pts',(-7.91106559513061,0.192895094132201,
68.3495205221433));
#49683=CARTESIAN_POINT('Ctrl Pts',(-7.91099954886372,-0.00267168074885584,
68.3574023474442));
#49684=CARTESIAN_POINT('',(-7.91835117330158,0.00158043531916788,70.357742247265));
#49685=CARTESIAN_POINT('Ctrl Pts',(-7.9109995297644,-0.00265674798181834,
68.3577753899841));
#49686=CARTESIAN_POINT('Ctrl Pts',(-7.91022048351088,-2.20343307818681,
68.4463271929765));
#49687=CARTESIAN_POINT('Ctrl Pts',(-6.94148933469359,-4.38669862313552,
68.5348789959691));
#49688=CARTESIAN_POINT('Ctrl Pts',(-3.67820201487734,-7.34180684107901,
68.7120182346942));
#49689=CARTESIAN_POINT('Ctrl Pts',(-1.40868175871169,-8.08992666571429,
68.8006056704269));
#49690=CARTESIAN_POINT('Ctrl Pts',(2.97309270521765,-7.65454228025058,68.9777805418923));
#49691=CARTESIAN_POINT('Ctrl Pts',(5.05102072675991,-6.47444880833913,69.066367977625));
#49692=CARTESIAN_POINT('Ctrl Pts',(7.66951518848024,-2.93425195367288,69.2435428490905));
#49693=CARTESIAN_POINT('Ctrl Pts',(8.18956872247094,-0.601881960095041,
69.3321302848232));
#49694=CARTESIAN_POINT('Ctrl Pts',(7.32306689761173,3.71537198232768,69.5093051562886));
#49695=CARTESIAN_POINT('Ctrl Pts',(5.94329958849969,5.66643518936744,69.5978925920213));
#49696=CARTESIAN_POINT('Ctrl Pts',(2.16154501637579,7.92205913233063,69.7750674634867));
#49697=CARTESIAN_POINT('Ctrl Pts',(-0.210816529302805,8.20894963712989,
69.8636548992195));
#49698=CARTESIAN_POINT('Ctrl Pts',(-4.42123908576595,6.91982244717722,70.0408297706849));
#49699=CARTESIAN_POINT('Ctrl Pts',(-6.22631625634286,5.35390358803395,70.1294172064176));
#49700=CARTESIAN_POINT('Ctrl Pts',(-7.65294264462806,2.31383904225023,70.2645374591378));
#49701=CARTESIAN_POINT('Ctrl Pts',(-7.91075848970524,1.15811126578363,70.3110702761253));
#49702=CARTESIAN_POINT('Ctrl Pts',(-7.91099983040495,0.00162536129911048,
70.3576030931128));
#49703=CARTESIAN_POINT('',(-7.90558067573546,0.00500151420475855,72.3576672233085));
#49704=CARTESIAN_POINT('Ctrl Pts',(-7.92187310646681,0.00155891186407059,
70.357808914217));
#49705=CARTESIAN_POINT('Ctrl Pts',(-7.90511105438765,-2.38948601125333,
70.4543338530758));
#49706=CARTESIAN_POINT('Ctrl Pts',(-5.47263506421283,-7.43816085005188,
70.6569359446836));
#49707=CARTESIAN_POINT('Ctrl Pts',(1.6316743039881,-8.57466520584624,70.9125766126657));
#49708=CARTESIAN_POINT('Ctrl Pts',(6.11859740475592,-5.49545041821264,71.1247309181634));
#49709=CARTESIAN_POINT('Ctrl Pts',(8.70002820540714,-0.704807661137227,
71.3368852236616));
#49710=CARTESIAN_POINT('Ctrl Pts',(6.73925246187953,6.4964979269881,71.6020781055336));
#49711=CARTESIAN_POINT('Ctrl Pts',(-1.83418328520544,9.17844853159298,71.9203095637806));
#49712=CARTESIAN_POINT('Ctrl Pts',(-7.27268681968312,4.62039446097428,72.1721722487799));
#49713=CARTESIAN_POINT('Ctrl Pts',(-7.90629361575619,0.994517640416839,
72.3179577810305));
#49714=CARTESIAN_POINT('Ctrl Pts',(-7.90104139764401,0.00502514377492854,
72.3576661605321));
#49715=CARTESIAN_POINT('',(-7.90643489614128,-0.00593696359886245,74.3576698040782));
#49716=CARTESIAN_POINT('Ctrl Pts',(-7.91099843674435,0.00497331162246579,
72.3576684917633));
#49717=CARTESIAN_POINT('Ctrl Pts',(-7.91112856116881,-0.202014345030353,
72.3659644912846));
#49718=CARTESIAN_POINT('Ctrl Pts',(-7.90312996393247,-0.409024146823264,
72.3742604908059));
#49719=CARTESIAN_POINT('Ctrl Pts',(-7.88702893860843,-0.615382418950373,
72.3825564903272));
#49720=CARTESIAN_POINT('Ctrl Pts',(-7.87157697295438,-0.813422038736245,
72.3905180640213));
#49721=CARTESIAN_POINT('Ctrl Pts',(-7.84866306220442,-1.01086127600091,
72.3984796377155));
#49722=CARTESIAN_POINT('Ctrl Pts',(-7.81836350731622,-1.20710938504594,
72.4064412114096));
#49723=CARTESIAN_POINT('Ctrl Pts',(-7.78805591091661,-1.40340957840095,
72.414404898108));
#49724=CARTESIAN_POINT('Ctrl Pts',(-7.75035881338431,-1.59851768184371,
72.4223685848063));
#49725=CARTESIAN_POINT('Ctrl Pts',(-7.70539985696176,-1.79185212680445,
72.4303322715046));
#49726=CARTESIAN_POINT('Ctrl Pts',(-7.66042202043323,-1.98526776081186,
72.438299302481));
#49727=CARTESIAN_POINT('Ctrl Pts',(-7.60817632116129,-2.17690792500901,
72.4462663334573));
#49728=CARTESIAN_POINT('Ctrl Pts',(-7.54884067694061,-2.36620485887569,
72.4542333644336));
#49729=CARTESIAN_POINT('Ctrl Pts',(-7.48947094380602,-2.5556105457013,72.462204972548));
#49730=CARTESIAN_POINT('Ctrl Pts',(-7.42300324516288,-2.74266999891853,
72.4701765806623));
#49731=CARTESIAN_POINT('Ctrl Pts',(-7.34966428105129,-2.92683377659868,
72.4781481887767));
#49732=CARTESIAN_POINT('Ctrl Pts',(-7.27623264649205,-3.11123026195236,
72.4861298697425));
#49733=CARTESIAN_POINT('Ctrl Pts',(-7.19591252544145,-3.29272345089769,
72.4941115507083));
#49734=CARTESIAN_POINT('Ctrl Pts',(-7.10897794312644,-3.47078573296334,
72.5020932316741));
#49735=CARTESIAN_POINT('Ctrl Pts',(-7.0219791373449,-3.64897955965377,72.5100808091567));
#49736=CARTESIAN_POINT('Ctrl Pts',(-6.92835628278054,-3.8237371302206,72.5180683866393));
#49737=CARTESIAN_POINT('Ctrl Pts',(-6.82842792612095,-3.99455793020598,
72.5260559641218));
#49738=CARTESIAN_POINT('Ctrl Pts',(-6.72836088398868,-4.16561580367263,
72.534054627156));
#49739=CARTESIAN_POINT('Ctrl Pts',(-6.62197103827709,-4.33272571100648,
72.5420532901902));
#49740=CARTESIAN_POINT('Ctrl Pts',(-6.50961926987508,-4.49541744015736,
72.5500519532245));
#49741=CARTESIAN_POINT('Ctrl Pts',(-6.47815304877411,-4.54098231193084,
72.5522921289077));
#49742=CARTESIAN_POINT('Ctrl Pts',(-6.44621941909069,-4.58620083614637,
72.554532304591));
#49743=CARTESIAN_POINT('Ctrl Pts',(-6.41382684745901,-4.63106317931574,
72.5567724802742));
#49744=CARTESIAN_POINT('Ctrl Pts',(-6.30047866556183,-4.78804562244238,
72.5646113096119));
#49745=CARTESIAN_POINT('Ctrl Pts',(-6.18119242386372,-4.94110127454116,
72.5724501389496));
#49746=CARTESIAN_POINT('Ctrl Pts',(-6.05627048094666,-5.08974546137762,
72.5802889682873));
#49747=CARTESIAN_POINT('Ctrl Pts',(-5.93148857345526,-5.23822302054653,
72.5881190104273));
#49748=CARTESIAN_POINT('Ctrl Pts',(-5.80108376814313,-5.38229869488082,
72.5959490525673));
#49749=CARTESIAN_POINT('Ctrl Pts',(-5.66540187578194,-5.52151633031059,
72.6037790947074));
#49750=CARTESIAN_POINT('Ctrl Pts',(-5.52984567315883,-5.6606050006454,72.6116018834407));
#49751=CARTESIAN_POINT('Ctrl Pts',(-5.38902236232815,-5.79484434408087,
72.619424672174));
#49752=CARTESIAN_POINT('Ctrl Pts',(-5.2433183435068,-5.92381074551214,72.6272474609074));
#49753=CARTESIAN_POINT('Ctrl Pts',(-5.09772095574409,-6.05268276503121,
72.6350645246631));
#49754=CARTESIAN_POINT('Ctrl Pts',(-4.94725023629629,-6.1762892963495,72.6428815884189));
#49755=CARTESIAN_POINT('Ctrl Pts',(-4.79232993588311,-6.29424298749569,
72.6506986521746));
#49756=CARTESIAN_POINT('Ctrl Pts',(-4.63749288684988,-6.41213329245212,
72.658511515181));
#49757=CARTESIAN_POINT('Ctrl Pts',(-4.47821129915083,-6.5243765959394,72.6663243781874));
#49758=CARTESIAN_POINT('Ctrl Pts',(-4.31494268944502,-6.63062520331265,
72.6741372411939));
#49759=CARTESIAN_POINT('Ctrl Pts',(-4.15173007737677,-6.73683736968835,
72.6819474245556));
#49760=CARTESIAN_POINT('Ctrl Pts',(-3.98453346235306,-6.83705874489097,
72.6897576079173));
#49761=CARTESIAN_POINT('Ctrl Pts',(-3.81384023064639,-6.93098432368037,
72.697567791279));
#49762=CARTESIAN_POINT('Ctrl Pts',(-3.64313930051956,-7.02491413859889,
72.705378326887));
#49763=CARTESIAN_POINT('Ctrl Pts',(-3.46894174238145,-7.1125474121264,72.7131888624951));
#49764=CARTESIAN_POINT('Ctrl Pts',(-3.29176094134949,-7.19362432331616,
72.7209993981032));
#49765=CARTESIAN_POINT('Ctrl Pts',(-3.11456593907785,-7.27470773291118,
72.7288105597344));
#49766=CARTESIAN_POINT('Ctrl Pts',(-2.93438753736343,-7.3492335861182,72.7366217213657));
#49767=CARTESIAN_POINT('Ctrl Pts',(-2.75176048389116,-7.4169896345684,72.7444328829969));
#49768=CARTESIAN_POINT('Ctrl Pts',(-2.56908662845072,-7.48476304691055,
72.7522460464003));
#49769=CARTESIAN_POINT('Ctrl Pts',(-2.38396320107523,-7.54576307590045,
72.7600592098036));
#49770=CARTESIAN_POINT('Ctrl Pts',(-2.19694168013937,-7.59982685684789,
72.767872373207));
#49771=CARTESIAN_POINT('Ctrl Pts',(-2.00983928999057,-7.65391401529429,
72.7756889150684));
#49772=CARTESIAN_POINT('Ctrl Pts',(-1.82083750901631,-7.70105885339732,
72.7835054569299));
#49773=CARTESIAN_POINT('Ctrl Pts',(-1.63049975986896,-7.74114923852184,
72.7913219987913));
#49774=CARTESIAN_POINT('Ctrl Pts',(-1.43993988328478,-7.78128640981742,
72.799147662692));
#49775=CARTESIAN_POINT('Ctrl Pts',(-1.24804126890946,-7.8143526125569,72.8069733265927));
#49776=CARTESIAN_POINT('Ctrl Pts',(-1.0553753461434,-7.84028723190373,72.8147989904933));
#49777=CARTESIAN_POINT('Ctrl Pts',(-0.862583837594134,-7.86623875626125,
72.8226297554109));
#49778=CARTESIAN_POINT('Ctrl Pts',(-0.669024372869679,-7.88504939954695,
72.8304605203284));
#49779=CARTESIAN_POINT('Ctrl Pts',(-0.475270250639864,-7.89671065627054,
72.838291285246));
#49780=CARTESIAN_POINT('Ctrl Pts',(-0.281236174430739,-7.90838876226261,
72.8461333647811));
#49781=CARTESIAN_POINT('Ctrl Pts',(-0.0870072292878414,-7.91289684099874,
72.8539754443163));
#49782=CARTESIAN_POINT('Ctrl Pts',(0.106845339014254,-7.91027844475344,
72.8618175238514));
#49783=CARTESIAN_POINT('Ctrl Pts',(0.215499356907363,-7.90881083834007,
72.866212995408));
#49784=CARTESIAN_POINT('Ctrl Pts',(0.324035244514684,-7.90510532434733,
72.8706084669645));
#49785=CARTESIAN_POINT('Ctrl Pts',(0.432353660334651,-7.8991766224332,72.875003938521));
#49786=CARTESIAN_POINT('Ctrl Pts',(0.627441848176251,-7.88849866242129,
72.8829204555249));
#49787=CARTESIAN_POINT('Ctrl Pts',(0.822409615450803,-7.8705741175999,72.8908369725288));
#49788=CARTESIAN_POINT('Ctrl Pts',(1.0166768073984,-7.84539924218635,72.8987534895327));
#49789=CARTESIAN_POINT('Ctrl Pts',(1.21072019175754,-7.82025336975628,72.9066608862288));
#49790=CARTESIAN_POINT('Ctrl Pts',(1.40406427008146,-7.78787384782983,72.9145682829249));
#49791=CARTESIAN_POINT('Ctrl Pts',(1.59612977651121,-7.74830889527091,72.922475679621));
#49792=CARTESIAN_POINT('Ctrl Pts',(1.78800960272789,-7.70878219231213,72.9303754318049));
#49793=CARTESIAN_POINT('Ctrl Pts',(1.97861298425648,-7.66208396562109,72.9382751839889));
#49794=CARTESIAN_POINT('Ctrl Pts',(2.16736637655079,-7.60831413585146,72.9461749361728));
#49795=CARTESIAN_POINT('Ctrl Pts',(2.35597225546501,-7.55458632794559,72.9540685145914));
#49796=CARTESIAN_POINT('Ctrl Pts',(2.54273069577453,-7.49379802149107,72.96196209301));
#49797=CARTESIAN_POINT('Ctrl Pts',(2.72707866063372,-7.42610011908782,72.9698556714287));
#49798=CARTESIAN_POINT('Ctrl Pts',(2.91131669508752,-7.35844258630765,72.9777445427474));
#49799=CARTESIAN_POINT('Ctrl Pts',(3.09314679574391,-7.28388378614634,72.9856334140662));
#49800=CARTESIAN_POINT('Ctrl Pts',(3.27202113046216,-7.20262443292784,72.993522285385));
#49801=CARTESIAN_POINT('Ctrl Pts',(3.45082191905448,-7.12139849037519,73.0014079131086));
#49802=CARTESIAN_POINT('Ctrl Pts',(3.62666905050166,-7.0334776276693,73.0092935408323));
#49803=CARTESIAN_POINT('Ctrl Pts',(3.79903446250772,-6.93911076094615,73.0171791685559));
#49804=CARTESIAN_POINT('Ctrl Pts',(3.97138454308658,-6.84475228789509,73.0250640948748));
#49805=CARTESIAN_POINT('Ctrl Pts',(4.14025321600823,-6.74394911287841,73.0329490211936));
#49806=CARTESIAN_POINT('Ctrl Pts',(4.30513637538387,-6.63699644337306,73.0408339475124));
#49807=CARTESIAN_POINT('Ctrl Pts',(4.47001896408724,-6.53004414403846,73.0487188465409));
#49808=CARTESIAN_POINT('Ctrl Pts',(4.63091577721423,-6.41694257974099,73.0566037455695));
#49809=CARTESIAN_POINT('Ctrl Pts',(4.78735101332433,-6.29803074581432,73.064488644598));
#49810=CARTESIAN_POINT('Ctrl Pts',(4.94381195425236,-6.17909937276644,73.0723748392419));
#49811=CARTESIAN_POINT('Ctrl Pts',(5.09580958298998,-6.05435603636255,73.0802610338858));
#49812=CARTESIAN_POINT('Ctrl Pts',(5.24290036559014,-5.92418068229648,73.0881472285297));
#49813=CARTESIAN_POINT('Ctrl Pts',(5.39003999613593,-5.79396209779472,73.0960360421305));
#49814=CARTESIAN_POINT('Ctrl Pts',(5.53226927578104,-5.65830812962327,73.1039248557311));
#49815=CARTESIAN_POINT('Ctrl Pts',(5.66918061027377,-5.51763646936765,73.1118136693318));
#49816=CARTESIAN_POINT('Ctrl Pts',(5.80622446450122,-5.37682864966863,73.1197101187027));
#49817=CARTESIAN_POINT('Ctrl Pts',(5.93793985156297,-5.23099368398513,73.1276065680736));
#49818=CARTESIAN_POINT('Ctrl Pts',(6.06395795657046,-5.0805841102127,73.1355030174445));
#49819=CARTESIAN_POINT('Ctrl Pts',(6.190045712928,-4.93009140370412,73.1434038312546));
#49820=CARTESIAN_POINT('Ctrl Pts',(6.31042969792822,-4.77501931958236,73.1513046450647));
#49821=CARTESIAN_POINT('Ctrl Pts',(6.4247835647362,-4.61585064167978,73.1592054588749));
#49822=CARTESIAN_POINT('Ctrl Pts',(6.53927638915582,-4.45648854924783,73.1671158733941));
#49823=CARTESIAN_POINT('Ctrl Pts',(6.64772426864196,-4.29302020600155,73.1750262879134));
#49824=CARTESIAN_POINT('Ctrl Pts',(6.74984549421544,-4.12595525959984,73.1829367024327));
#49825=CARTESIAN_POINT('Ctrl Pts',(6.79416324287183,-4.05345375697541,73.1863696005444));
#49826=CARTESIAN_POINT('Ctrl Pts',(6.83729008001318,-3.98027519227827,73.1898024986561));
#49827=CARTESIAN_POINT('Ctrl Pts',(6.87920577123963,-3.90646246071089,73.1932353967677));
#49828=CARTESIAN_POINT('Ctrl Pts',(6.98072775338417,-3.72768418944873,73.2015500543721));
#49829=CARTESIAN_POINT('Ctrl Pts',(7.07536409182775,-3.54479248452029,73.2098647119764));
#49830=CARTESIAN_POINT('Ctrl Pts',(7.16278704580388,-3.35833332718242,73.2181793695808));
#49831=CARTESIAN_POINT('Ctrl Pts',(7.25010194455162,-3.17210463433832,73.2264837502248));
#49832=CARTESIAN_POINT('Ctrl Pts',(7.33022111695024,-2.98231754762191,73.2347881308689));
#49833=CARTESIAN_POINT('Ctrl Pts',(7.40286217443645,-2.78954344405998,73.243092511513));
#49834=CARTESIAN_POINT('Ctrl Pts',(7.47541824782413,-2.59699487043909,73.2513871767106));
#49835=CARTESIAN_POINT('Ctrl Pts',(7.54051355296825,-2.40146652341505,73.2596818419082));
#49836=CARTESIAN_POINT('Ctrl Pts',(7.59791302528611,-2.20355137452878,73.2679765071058));
#49837=CARTESIAN_POINT('Ctrl Pts',(7.65522606353893,-2.00593425296159,73.2762586819163));
#49838=CARTESIAN_POINT('Ctrl Pts',(7.70486631435656,-1.8059377829597,73.2845408567268));
#49839=CARTESIAN_POINT('Ctrl Pts',(7.74664790199489,-1.60417183696703,73.2928230315373));
#49840=CARTESIAN_POINT('Ctrl Pts',(7.78839095501682,-1.40259197708958,73.3010975678054));
#49841=CARTESIAN_POINT('Ctrl Pts',(7.82228973910568,-1.19924618177941,73.3093721040735));
#49842=CARTESIAN_POINT('Ctrl Pts',(7.84820854440072,-0.994758082950565,
73.3176466403415));
#49843=CARTESIAN_POINT('Ctrl Pts',(7.87409753489035,-0.790505209966683,
73.3259116582817));
#49844=CARTESIAN_POINT('Ctrl Pts',(7.89202482691748,-0.585112945734738,
73.3341766762218));
#49845=CARTESIAN_POINT('Ctrl Pts',(7.9019059580874,-0.379213962747772,73.3424416941619));
#49846=CARTESIAN_POINT('Ctrl Pts',(7.90585498741587,-0.296925699538259,
73.3457448380717));
#49847=CARTESIAN_POINT('Ctrl Pts',(7.90851943387131,-0.214556603258294,
73.3490479819815));
#49848=CARTESIAN_POINT('Ctrl Pts',(7.90989621070171,-0.132147402270342,
73.3523511258913));
#49849=CARTESIAN_POINT('Ctrl Pts',(7.91334156146494,0.0740796326801837,
73.360617163741));
#49850=CARTESIAN_POINT('Ctrl Pts',(7.9087155022605,0.280324671188554,73.3688832015908));
#49851=CARTESIAN_POINT('Ctrl Pts',(7.89606065348131,0.485949746933029,73.3771492394405));
#49852=CARTESIAN_POINT('Ctrl Pts',(7.88339442547667,0.691759720508842,73.385422710102));
#49853=CARTESIAN_POINT('Ctrl Pts',(7.86268501313782,0.896948325257189,73.3936961807634));
#49854=CARTESIAN_POINT('Ctrl Pts',(7.8340268165024,1.10088366248269,73.4019696514249));
#49855=CARTESIAN_POINT('Ctrl Pts',(7.8053409857925,1.30501564726314,73.4102510998983));
#49856=CARTESIAN_POINT('Ctrl Pts',(7.76869110950227,1.50789166131395,73.4185325483718));
#49857=CARTESIAN_POINT('Ctrl Pts',(7.72422265443761,1.70889010315842,73.4268139968452));
#49858=CARTESIAN_POINT('Ctrl Pts',(7.6796801631823,1.91022319029111,73.4351092332251));
#49859=CARTESIAN_POINT('Ctrl Pts',(7.62729313179226,2.10967216826892,73.4434044696049));
#49860=CARTESIAN_POINT('Ctrl Pts',(7.56725742111864,2.30662873530287,73.4516997059848));
#49861=CARTESIAN_POINT('Ctrl Pts',(7.50716726540431,2.50376391783397,73.4600024651287));
#49862=CARTESIAN_POINT('Ctrl Pts',(7.43941467652915,2.69840189908309,73.4683052242726));
#49863=CARTESIAN_POINT('Ctrl Pts',(7.36424410043606,2.8899532572678,73.4766079834164));
#49864=CARTESIAN_POINT('Ctrl Pts',(7.28895824773573,3.08179836590421,73.4849234751207));
#49865=CARTESIAN_POINT('Ctrl Pts',(7.20623178261639,3.27054711904865,73.493238966825));
#49866=CARTESIAN_POINT('Ctrl Pts',(7.1163564409016,3.45563192571755,73.5015544585294));
#49867=CARTESIAN_POINT('Ctrl Pts',(7.08064478154718,3.52917474003488,73.5048585906911));
#49868=CARTESIAN_POINT('Ctrl Pts',(7.04380492569719,3.60213936756197,73.5081627228529));
#49869=CARTESIAN_POINT('Ctrl Pts',(7.00585711220989,3.67449141015436,73.5114668550147));
#49870=CARTESIAN_POINT('Ctrl Pts',(6.91501452263554,3.84769366625495,73.5193765576902));
#49871=CARTESIAN_POINT('Ctrl Pts',(6.81763001644092,4.01774461916287,73.5272862603657));
#49872=CARTESIAN_POINT('Ctrl Pts',(6.71394718237391,4.18411689993163,73.5351959630412));
#49873=CARTESIAN_POINT('Ctrl Pts',(6.61036954002703,4.35032038722022,73.5430976409049));
#49874=CARTESIAN_POINT('Ctrl Pts',(6.50050647898477,4.51285234657526,73.5509993187687));
#49875=CARTESIAN_POINT('Ctrl Pts',(6.3846482154567,4.67120842661357,73.5589009966324));
#49876=CARTESIAN_POINT('Ctrl Pts',(6.26888603325946,4.82943318185507,73.5667961216297));
#49877=CARTESIAN_POINT('Ctrl Pts',(6.14713875560896,4.9834886801912,73.574691246627));
#49878=CARTESIAN_POINT('Ctrl Pts',(6.01974091973089,5.1328978422834,73.5825863716243));
#49879=CARTESIAN_POINT('Ctrl Pts',(5.89242514065964,5.28221077009762,73.5904764113802));
#49880=CARTESIAN_POINT('Ctrl Pts',(5.75946627760064,5.4268830630797,73.5983664511361));
#49881=CARTESIAN_POINT('Ctrl Pts',(5.62124048922088,5.56646893122954,73.606256490892));
#49882=CARTESIAN_POINT('Ctrl Pts',(5.48307813732961,5.7059907387043,73.6141429096419));
#49883=CARTESIAN_POINT('Ctrl Pts',(5.33965391884534,5.84043052864044,73.6220293283918));
#49884=CARTESIAN_POINT('Ctrl Pts',(5.19138254565954,5.96937754415161,73.6299157471416));
#49885=CARTESIAN_POINT('Ctrl Pts',(5.04315176851963,6.09828925454051,73.637800006625));
#49886=CARTESIAN_POINT('Ctrl Pts',(4.89007674163458,6.22171096210383,73.6456842661083));
#49887=CARTESIAN_POINT('Ctrl Pts',(4.73260732106132,6.3392703795182,73.6535685255916));
#49888=CARTESIAN_POINT('Ctrl Pts',(4.57511951687059,6.45684352129474,73.6614537055153));
#49889=CARTESIAN_POINT('Ctrl Pts',(4.41323656598173,6.56855279372756,73.6693388854389));
#49890=CARTESIAN_POINT('Ctrl Pts',(4.24744004924162,6.67406727776236,73.6772240653626));
#49891=CARTESIAN_POINT('Ctrl Pts',(4.08162285334157,6.77959492221172,73.6851102287744));
#49892=CARTESIAN_POINT('Ctrl Pts',(3.91189140947407,6.87892605291088,73.6929963921861));
#49893=CARTESIAN_POINT('Ctrl Pts',(3.73875479338658,6.97177406367482,73.7008825555978));
#49894=CARTESIAN_POINT('Ctrl Pts',(3.56556753330826,7.06464923330274,73.7087710257821));
#49895=CARTESIAN_POINT('Ctrl Pts',(3.38897341986887,7.15103734103321,73.7166594959664));
#49896=CARTESIAN_POINT('Ctrl Pts',(3.20950476013447,7.23069845828701,73.7245479661506));
#49897=CARTESIAN_POINT('Ctrl Pts',(3.0299534918202,7.31039624317837,73.7324400673606));
#49898=CARTESIAN_POINT('Ctrl Pts',(2.84752535525844,7.38336072758949,73.7403321685706));
#49899=CARTESIAN_POINT('Ctrl Pts',(2.66277141849326,7.44940060493832,73.7482242697806));
#49900=CARTESIAN_POINT('Ctrl Pts',(2.47780329698364,7.51551704214022,73.7561255202824));
#49901=CARTESIAN_POINT('Ctrl Pts',(2.29050431416554,7.57469272137233,73.7640267707842));
#49902=CARTESIAN_POINT('Ctrl Pts',(2.10144056717119,7.62678625258682,73.771928021286));
#49903=CARTESIAN_POINT('Ctrl Pts',(1.9122515415065,7.67891430236145,73.7798345073666));
#49904=CARTESIAN_POINT('Ctrl Pts',(1.72129575480019,7.72395076983101,73.7877409934473));
#49905=CARTESIAN_POINT('Ctrl Pts',(1.52914845974499,7.7618055881386,73.7956474795279));
#49906=CARTESIAN_POINT('Ctrl Pts',(1.33673645052244,7.79971255761857,73.8035648580798));
#49907=CARTESIAN_POINT('Ctrl Pts',(1.14312999333838,7.83041806185964,73.8114822366316));
#49908=CARTESIAN_POINT('Ctrl Pts',(0.948909598373037,7.85388385285366,73.8193996151835));
#49909=CARTESIAN_POINT('Ctrl Pts',(0.864697498993089,7.86405839463426,73.8228325145428));
#49910=CARTESIAN_POINT('Ctrl Pts',(0.780369984610552,7.87287253021289,73.8262654139021));
#49911=CARTESIAN_POINT('Ctrl Pts',(0.695974292246004,7.88032618516091,73.8296983132614));
#49912=CARTESIAN_POINT('Ctrl Pts',(0.503191545222375,7.89735236310893,73.8375399903683));
#49913=CARTESIAN_POINT('Ctrl Pts',(0.309480002828726,7.90732678778585,73.8453816674753));
#49914=CARTESIAN_POINT('Ctrl Pts',(0.115403255200916,7.91015822146997,73.8532233445822));
#49915=CARTESIAN_POINT('Ctrl Pts',(-0.0784449856718756,7.91298632141252,
73.8610557888665));
#49916=CARTESIAN_POINT('Ctrl Pts',(-0.272657227937992,7.90868817129676,
73.8688882331508));
#49917=CARTESIAN_POINT('Ctrl Pts',(-0.46666271122103,7.89722400049257,73.8767206774351));
#49918=CARTESIAN_POINT('Ctrl Pts',(-0.660477537208162,7.88577109600811,
73.8845454244491));
#49919=CARTESIAN_POINT('Ctrl Pts',(-0.854085660550979,7.86716621558343,
73.8923701714631));
#49920=CARTESIAN_POINT('Ctrl Pts',(-1.0469140595466,7.84142155172923,73.9001949184771));
#49921=CARTESIAN_POINT('Ctrl Pts',(-1.23959047185993,7.81569717973072,73.9080134980523));
#49922=CARTESIAN_POINT('Ctrl Pts',(-1.43148803704333,7.78284427883069,73.9158320776276));
#49923=CARTESIAN_POINT('Ctrl Pts',(-1.62203640744121,7.74292702360904,73.9236506572028));
#49924=CARTESIAN_POINT('Ctrl Pts',(-1.81247164325526,7.70303346852217,73.9314645946405));
#49925=CARTESIAN_POINT('Ctrl Pts',(-2.00155893676101,7.65608398599158,73.9392785320782));
#49926=CARTESIAN_POINT('Ctrl Pts',(-2.18873552943269,7.60219427416841,73.9470924695159));
#49927=CARTESIAN_POINT('Ctrl Pts',(-2.37583737860299,7.54832608162654,73.9549032866861));
#49928=CARTESIAN_POINT('Ctrl Pts',(-2.56102970958169,7.48752327855418,73.9627141038562));
#49929=CARTESIAN_POINT('Ctrl Pts',(-2.74376220126369,7.41995215502881,73.9705249210264));
#49930=CARTESIAN_POINT('Ctrl Pts',(-2.9264874260422,7.35238371867105,73.9783354275761));
#49931=CARTESIAN_POINT('Ctrl Pts',(-3.10675267343504,7.27804761155472,73.9861459341258));
#49932=CARTESIAN_POINT('Ctrl Pts',(-3.28402453278888,7.1971594305004,73.9939564406755));
#49933=CARTESIAN_POINT('Ctrl Pts',(-3.46130127854716,7.11626901980642,74.0017671625176));
#49934=CARTESIAN_POINT('Ctrl Pts',(-3.63558415135138,7.02882632079456,74.0095778843597));
#49935=CARTESIAN_POINT('Ctrl Pts',(-3.80636144908283,6.93509434102637,74.0173886062018));
#49936=CARTESIAN_POINT('Ctrl Pts',(-3.97717352965858,6.84134327051895,74.0252009188826));
#49937=CARTESIAN_POINT('Ctrl Pts',(-4.14447830433175,6.74130053681446,74.0330132315634));
#49938=CARTESIAN_POINT('Ctrl Pts',(-4.30779019458443,6.63527427009934,74.0408255442442));
#49939=CARTESIAN_POINT('Ctrl Pts',(-4.47116411001637,6.52920773504742,74.0486408240089));
#49940=CARTESIAN_POINT('Ctrl Pts',(-4.63054182539353,6.41715333171838,74.0564561037737));
#49941=CARTESIAN_POINT('Ctrl Pts',(-4.78546805500666,6.29946160354286,74.0642713835384));
#49942=CARTESIAN_POINT('Ctrl Pts',(-4.94056276388966,6.18164188789561,74.0720951622683));
#49943=CARTESIAN_POINT('Ctrl Pts',(-5.09119603804208,6.05817281595878,74.0799189409983));
#49944=CARTESIAN_POINT('Ctrl Pts',(-5.23694610556563,5.9294448717735,74.0877427197282));
#49945=CARTESIAN_POINT('Ctrl Pts',(-5.38278459903386,5.8006388288932,74.0955712451113));
#49946=CARTESIAN_POINT('Ctrl Pts',(-5.52373372750108,5.66656779709337,74.1033997704944));
#49947=CARTESIAN_POINT('Ctrl Pts',(-5.65940967696242,5.52765801296572,74.1112282958776));
#49948=CARTESIAN_POINT('Ctrl Pts',(-5.79527234117178,5.38855706374621,74.1190675947334));
#49949=CARTESIAN_POINT('Ctrl Pts',(-5.92584709633149,5.24460432154438,74.1269068935893));
#49950=CARTESIAN_POINT('Ctrl Pts',(-6.05079066015617,5.09625876373707,74.1347461924452));
#49951=CARTESIAN_POINT('Ctrl Pts',(-6.12083108011365,5.01309973697655,74.1391407187995));
#49952=CARTESIAN_POINT('Ctrl Pts',(-6.18910269560798,4.92856081806555,74.1435352451539));
#49953=CARTESIAN_POINT('Ctrl Pts',(-6.25555115585064,4.84272658081537,74.1479297715083));
#49954=CARTESIAN_POINT('Ctrl Pts',(-6.37559513174575,4.68766078892482,74.1558688029596));
#49955=CARTESIAN_POINT('Ctrl Pts',(-6.49003378158572,4.52791714201392,74.1638078344109));
#49956=CARTESIAN_POINT('Ctrl Pts',(-6.5984834164448,4.3639360218618,74.1717468658621));
#49957=CARTESIAN_POINT('Ctrl Pts',(-6.70676445788647,4.20020982315291,74.1796735554697));
#49958=CARTESIAN_POINT('Ctrl Pts',(-6.80907485952521,4.03225956734306,74.1876002450773));
#49959=CARTESIAN_POINT('Ctrl Pts',(-6.90507137652646,3.86055828670867,74.1955269346849));
#49960=CARTESIAN_POINT('Ctrl Pts',(-7.00098019317911,3.68901386866302,74.2034463826397));
#49961=CARTESIAN_POINT('Ctrl Pts',(-7.09058644894565,3.51372554759673,74.2113658305945));
#49962=CARTESIAN_POINT('Ctrl Pts',(-7.17358974895407,3.33519581339703,74.2192852785494));
#49963=CARTESIAN_POINT('Ctrl Pts',(-7.25653085123015,3.15679985875332,74.2271987921413));
#49964=CARTESIAN_POINT('Ctrl Pts',(-7.33287871113123,2.97516763810119,74.2351123057332));
#49965=CARTESIAN_POINT('Ctrl Pts',(-7.40237837150453,2.79082701812241,74.2430258193252));
#49966=CARTESIAN_POINT('Ctrl Pts',(-7.47183736547843,2.60659426153802,74.2509347024757));
#49967=CARTESIAN_POINT('Ctrl Pts',(-7.53445602383177,2.41965658213687,74.2588435856262));
#49968=CARTESIAN_POINT('Ctrl Pts',(-7.59002701499753,2.23056291361793,74.2667524687767));
#49969=CARTESIAN_POINT('Ctrl Pts',(-7.64557659394122,2.04154210533663,74.2746583045322));
#49970=CARTESIAN_POINT('Ctrl Pts',(-7.6940838197897,1.85036729046182,74.2825641402877));
#49971=CARTESIAN_POINT('Ctrl Pts',(-7.73539073835603,1.65760403141272,74.2904699760432));
#49972=CARTESIAN_POINT('Ctrl Pts',(-7.77668764955054,1.46488747286015,74.2983738964625));
#49973=CARTESIAN_POINT('Ctrl Pts',(-7.81078765953284,1.27058357133946,74.3062778168818));
#49974=CARTESIAN_POINT('Ctrl Pts',(-7.83758354196369,1.07526983717572,74.314181737301));
#49975=CARTESIAN_POINT('Ctrl Pts',(-7.86438252247724,0.879933521255138,
74.3220865715547));
#49976=CARTESIAN_POINT('Ctrl Pts',(-7.88387563669531,0.68358747748106,74.3299914058084));
#49977=CARTESIAN_POINT('Ctrl Pts',(-7.89600724731406,0.486816752345093,
74.3378962400621));
#49978=CARTESIAN_POINT('Ctrl Pts',(-7.90612212347712,0.322756795278237,
74.3444869906292));
#49979=CARTESIAN_POINT('Ctrl Pts',(-7.91112049543788,0.158401844073439,
74.3510777411962));
#49980=CARTESIAN_POINT('Ctrl Pts',(-7.91099779416079,-0.00590768847896494,
74.3576684917633));
#49981=CARTESIAN_POINT('',(-7.91846474044373,-0.0010690628187093,76.3576290758486));
#49982=CARTESIAN_POINT('Ctrl Pts',(-7.90280119522295,-0.00596027707849772,
74.3576708491509));
#49983=CARTESIAN_POINT('Ctrl Pts',(-7.90869288684778,-0.90659764281454,
74.3938343093522));
#49984=CARTESIAN_POINT('Ctrl Pts',(-7.34860918258986,-4.44156078704885,
74.5360749223026));
#49985=CARTESIAN_POINT('Ctrl Pts',(-2.13974124634984,-9.11203122848944,
74.7843926880019));
#49986=CARTESIAN_POINT('Ctrl Pts',(6.51845747696313,-6.71804149910057,75.1026241462487));
#49987=CARTESIAN_POINT('Ctrl Pts',(8.71876257165608,0.413892218516685,75.3678170281211));
#49988=CARTESIAN_POINT('Ctrl Pts',(6.29868987220236,5.28787691418045,75.5799713336189));
#49989=CARTESIAN_POINT('Ctrl Pts',(1.91734040228322,8.51567395457576,75.792125639117));
#49990=CARTESIAN_POINT('Ctrl Pts',(-5.320841699348,7.60369065835455,76.0513265910671));
#49991=CARTESIAN_POINT('Ctrl Pts',(-7.91108836642875,2.47685045337626,76.2574889666432));
#49992=CARTESIAN_POINT('Ctrl Pts',(-7.92335669526798,-0.00104753037717561,
76.3575741894703));
#49993=CARTESIAN_POINT('',(-7.911,-5.90194559890733E-12,78.3576684917633));
#49994=CARTESIAN_POINT('Ctrl Pts',(-7.91099991910456,-0.00110191999642655,
76.3577128290767));
#49995=CARTESIAN_POINT('Ctrl Pts',(-7.9106767122703,-2.20240473643408,76.4462854857049));
#49996=CARTESIAN_POINT('Ctrl Pts',(-6.94187350370004,-4.38635073437256,
76.5348581423331));
#49997=CARTESIAN_POINT('Ctrl Pts',(-3.67820201487791,-7.34180684107874,
76.7120182346942));
#49998=CARTESIAN_POINT('Ctrl Pts',(-1.40868175871223,-8.08992666571422,
76.8006056704269));
#49999=CARTESIAN_POINT('Ctrl Pts',(2.97309270521729,-7.65454228025075,76.9777805418923));
#50000=CARTESIAN_POINT('Ctrl Pts',(5.05102072675967,-6.47444880833934,77.066367977625));
#50001=CARTESIAN_POINT('Ctrl Pts',(7.6695151884802,-2.93425195367305,77.2435428490905));
#50002=CARTESIAN_POINT('Ctrl Pts',(8.18956872247096,-0.601881960095122,
77.3321302848232));
#50003=CARTESIAN_POINT('Ctrl Pts',(7.32306689761172,3.71537198232775,77.5093051562886));
#50004=CARTESIAN_POINT('Ctrl Pts',(5.9432995884996,5.66643518936756,77.5978925920213));
#50005=CARTESIAN_POINT('Ctrl Pts',(2.16154501637551,7.92205913233073,77.7750674634868));
#50006=CARTESIAN_POINT('Ctrl Pts',(-0.210816529303192,8.2089496371299,77.8636548992195));
#50007=CARTESIAN_POINT('Ctrl Pts',(-4.42123908576641,6.91982244717695,78.0408297706849));
#50008=CARTESIAN_POINT('Ctrl Pts',(-6.22631625634328,5.35390358803349,78.1294172064176));
#50009=CARTESIAN_POINT('Ctrl Pts',(-7.65317280859601,2.31334857514211,78.264559258688));
#50010=CARTESIAN_POINT('Ctrl Pts',(-7.91100000000086,1.15702837836061,78.3111138752256));
#50011=CARTESIAN_POINT('Ctrl Pts',(-7.911,-5.90194559890733E-12,78.3576684917633));
#50012=CARTESIAN_POINT('',(-7.90317141111203,-0.000228506537956913,80.3576684917633));
#50013=CARTESIAN_POINT('Ctrl Pts',(-7.911,-5.90194559890733E-12,78.3576684917633));
#50014=CARTESIAN_POINT('Ctrl Pts',(-7.91099999999836,-2.20167589667262,
78.446255927496));
#50015=CARTESIAN_POINT('Ctrl Pts',(-6.94214576672048,-4.38610418339192,
78.5348433632287));
#50016=CARTESIAN_POINT('Ctrl Pts',(-3.67820201487754,-7.34180684107897,
78.7120182346942));
#50017=CARTESIAN_POINT('Ctrl Pts',(-1.40868175871163,-8.08992666571436,
78.8006056704269));
#50018=CARTESIAN_POINT('Ctrl Pts',(2.97309270521814,-7.65454228025046,78.9777805418923));
#50019=CARTESIAN_POINT('Ctrl Pts',(5.05102072676055,-6.47444880833871,79.0663679776251));
#50020=CARTESIAN_POINT('Ctrl Pts',(7.66951518848072,-2.93425195367178,79.2435428490905));
#50021=CARTESIAN_POINT('Ctrl Pts',(8.18956872247111,-0.601881960093584,
79.3321302848233));
#50022=CARTESIAN_POINT('Ctrl Pts',(7.32306689761092,3.7153719823294,79.5093051562887));
#50023=CARTESIAN_POINT('Ctrl Pts',(5.94329958849824,5.66643518936905,79.5978925920214));
#50024=CARTESIAN_POINT('Ctrl Pts',(2.1615450163733,7.92205913233138,79.7750674634869));
#50025=CARTESIAN_POINT('Ctrl Pts',(-0.210816529305671,8.20894963712987,
79.8636548992196));
#50026=CARTESIAN_POINT('Ctrl Pts',(-4.42123908576876,6.91982244717549,80.040829770685));
#50027=CARTESIAN_POINT('Ctrl Pts',(-6.22631625634523,5.35390358803129,80.1294172064178));
#50028=CARTESIAN_POINT('Ctrl Pts',(-7.65317280859644,2.31334857514018,80.2645592586881));
#50029=CARTESIAN_POINT('Ctrl Pts',(-7.91100000000084,1.15702837835973,80.3111138752257));
#50030=CARTESIAN_POINT('Ctrl Pts',(-7.911,-5.73152636462737E-12,80.3576684917633));
#50031=CARTESIAN_POINT('',(-7.91272987124828,-0.0069511639008941,82.3576684917633));
#50032=CARTESIAN_POINT('Ctrl Pts',(-7.8982622858675,-0.000371797647241044,
80.3576684917633));
#50033=CARTESIAN_POINT('Ctrl Pts',(-7.89966465680796,-1.28819607809109,
80.4092986399904));
#50034=CARTESIAN_POINT('Ctrl Pts',(-6.99340059655887,-5.22096879316791,
80.5670059409665));
#50035=CARTESIAN_POINT('Ctrl Pts',(-0.782238527603077,-9.32791637320139,
80.8307903946915));
#50036=CARTESIAN_POINT('Ctrl Pts',(6.03998710817404,-6.30125683006582,81.0959832765638));
#50037=CARTESIAN_POINT('Ctrl Pts',(8.12481793067604,-1.27457286690791,81.3081375820617));
#50038=CARTESIAN_POINT('Ctrl Pts',(7.67936794651516,4.14904204326629,81.5202918875595));
#50039=CARTESIAN_POINT('Ctrl Pts',(2.11166538450812,9.11936872126833,81.7854847694319));
#50040=CARTESIAN_POINT('Ctrl Pts',(-5.95633015797621,6.86030266448923,82.0822898296246));
#50041=CARTESIAN_POINT('Ctrl Pts',(-7.89397529231162,2.09439459744815,82.2730177370685));
#50042=CARTESIAN_POINT('Ctrl Pts',(-7.91272987124828,-0.0069511639008941,
82.3576684917633));
#50043=CARTESIAN_POINT('',(-7.91724620790701,0.00276230921017722,84.3576684917632));
#50044=CARTESIAN_POINT('Ctrl Pts',(-7.91272987124828,-0.0069511639008941,
82.3576684917633));
#50045=CARTESIAN_POINT('Ctrl Pts',(-7.91747694143191,-0.538833849344243,
82.3790948898174));
#50046=CARTESIAN_POINT('Ctrl Pts',(-7.62500664949156,-3.69864297510493,
82.5065984406204));
#50047=CARTESIAN_POINT('Ctrl Pts',(-3.380753567549,-8.72803821522355,82.7401791441724));
#50048=CARTESIAN_POINT('Ctrl Pts',(5.5255655561909,-7.5558013701102,83.058410602419));
#50049=CARTESIAN_POINT('Ctrl Pts',(8.6920369109565,-0.797332397813895,83.3236034842915));
#50050=CARTESIAN_POINT('Ctrl Pts',(6.97023541016857,4.36497741430031,83.5357577897894));
#50051=CARTESIAN_POINT('Ctrl Pts',(3.07771910783116,8.16791831007078,83.7479120952873));
#50052=CARTESIAN_POINT('Ctrl Pts',(-4.38505643770802,8.27002356725942,84.0131049771596));
#50053=CARTESIAN_POINT('Ctrl Pts',(-7.81686525122821,3.06263226942611,84.2340366347764));
#50054=CARTESIAN_POINT('Ctrl Pts',(-7.92391013983324,0.220078610135003,
84.3488911396443));
#50055=CARTESIAN_POINT('Ctrl Pts',(-7.92261405080686,0.00276418203836634,
84.3576684917632));
#50056=CARTESIAN_POINT('',(-7.91099839329515,0.0035651983779998,86.3576684917632));
#50057=CARTESIAN_POINT('Ctrl Pts',(-7.91099951849852,0.00276012975443844,
84.3576684917632));
#50058=CARTESIAN_POINT('Ctrl Pts',(-7.91106692192262,-0.190429503722451,
84.3654829140546));
#50059=CARTESIAN_POINT('Ctrl Pts',(-7.90405347510339,-0.383899768578029,
84.3732973363459));
#50060=CARTESIAN_POINT('Ctrl Pts',(-7.88992372170109,-0.57708289329906,
84.3811117586372));
#50061=CARTESIAN_POINT('Ctrl Pts',(-7.8758085715249,-0.770066361538518,
84.3889181046535));
#50062=CARTESIAN_POINT('Ctrl Pts',(-7.85459178483221,-0.962762930611376,
84.3967244506698));
#50063=CARTESIAN_POINT('Ctrl Pts',(-7.82628987288226,-1.1546028865461,84.404530796686));
#50064=CARTESIAN_POINT('Ctrl Pts',(-7.79801162681802,-1.34628242708271,
84.4123306150834));
#50065=CARTESIAN_POINT('Ctrl Pts',(-7.76266010513328,-1.53710643273618,
84.4201304334808));
#50066=CARTESIAN_POINT('Ctrl Pts',(-7.72030377557192,-1.72650821396538,
84.4279302518783));
#50067=CARTESIAN_POINT('Ctrl Pts',(-7.67797451163443,-1.91578896777265,
84.4357250862048));
#50068=CARTESIAN_POINT('Ctrl Pts',(-7.62864943192344,-2.10364896292528,
84.4435199205313));
#50069=CARTESIAN_POINT('Ctrl Pts',(-7.57244846598746,-2.28952947785438,
84.4513147548578));
#50070=CARTESIAN_POINT('Ctrl Pts',(-7.51627233435907,-2.47532785515815,
84.4591061447717));
#50071=CARTESIAN_POINT('Ctrl Pts',(-7.45322647154974,-2.65914815643696,
84.4668975346857));
#50072=CARTESIAN_POINT('Ctrl Pts',(-7.38348129528783,-2.84044450080171,
84.4746889245996));
#50073=CARTESIAN_POINT('Ctrl Pts',(-7.3137431265908,-3.02172262962868,84.4824795316828));
#50074=CARTESIAN_POINT('Ctrl Pts',(-7.23730710512835,-3.20047697360211,
84.4902701387659));
#50075=CARTESIAN_POINT('Ctrl Pts',(-7.15439279207838,-3.37617902023232,
84.4980607458491));
#50076=CARTESIAN_POINT('Ctrl Pts',(-7.07147906752829,-3.55187981978434,
84.505851297637));
#50077=CARTESIAN_POINT('Ctrl Pts',(-6.98208729351078,-3.72452804443674,
84.5136418494249));
#50078=CARTESIAN_POINT('Ctrl Pts',(-6.88648423743967,-3.8936173216554,84.5214324012127));
#50079=CARTESIAN_POINT('Ctrl Pts',(-6.7908647923431,-4.06273558548373,84.5292242885181));
#50080=CARTESIAN_POINT('Ctrl Pts',(-6.68903211880367,-4.22829337836133,
84.5370161758234));
#50081=CARTESIAN_POINT('Ctrl Pts',(-6.58129784696126,-4.38981088995678,
84.5448080631288));
#50082=CARTESIAN_POINT('Ctrl Pts',(-6.47352587108237,-4.55138492824558,
84.5526026773807));
#50083=CARTESIAN_POINT('Ctrl Pts',(-6.35984837987453,-4.70891557471506,
84.5603972916326));
#50084=CARTESIAN_POINT('Ctrl Pts',(-6.24061909826932,-4.86195375032674,
84.5681919058845));
#50085=CARTESIAN_POINT('Ctrl Pts',(-6.1212668145275,-5.01514980680737,84.5759945614011));
#50086=CARTESIAN_POINT('Ctrl Pts',(-5.99635151992537,-5.16384385726863,
84.5837972169177));
#50087=CARTESIAN_POINT('Ctrl Pts',(-5.86626647117264,-5.30762081249177,
84.5915998724342));
#50088=CARTESIAN_POINT('Ctrl Pts',(-5.73610523332489,-5.45148197597871,
84.5994070978631));
#50089=CARTESIAN_POINT('Ctrl Pts',(-5.60076845418176,-5.59042005269074,
84.6072143232919));
#50090=CARTESIAN_POINT('Ctrl Pts',(-5.4606847014455,-5.72405831481468,84.6150215487207));
#50091=CARTESIAN_POINT('Ctrl Pts',(-5.32041782530811,-5.85787127452206,
84.6228389800846));
#50092=CARTESIAN_POINT('Ctrl Pts',(-5.17539184732898,-5.98637035017073,
84.6306564114484));
#50093=CARTESIAN_POINT('Ctrl Pts',(-5.0260675072528,-6.10921978754551,84.6384738428122));
#50094=CARTESIAN_POINT('Ctrl Pts',(-4.95542999033655,-6.16733341594853,
84.6421718597593));
#50095=CARTESIAN_POINT('Ctrl Pts',(-4.88383102554381,-6.22418343540095,
84.6458698767063));
#50096=CARTESIAN_POINT('Ctrl Pts',(-4.81132146298963,-6.2797377954637,84.6495678936533));
#50097=CARTESIAN_POINT('Ctrl Pts',(-4.65622728924412,-6.39856567510311,
84.657477759093));
#50098=CARTESIAN_POINT('Ctrl Pts',(-4.4965190550354,-6.51180483402569,84.6653876245328));
#50099=CARTESIAN_POINT('Ctrl Pts',(-4.33263655781297,-6.61907708505518,
84.6732974899725));
#50100=CARTESIAN_POINT('Ctrl Pts',(-4.16893216684854,-6.72623275341391,
84.6811987590303));
#50101=CARTESIAN_POINT('Ctrl Pts',(-4.00106283495899,-6.82743424330512,
84.689100028088));
#50102=CARTESIAN_POINT('Ctrl Pts',(-3.82950127463175,-6.92234360513792,
84.6970012971458));
#50103=CARTESIAN_POINT('Ctrl Pts',(-3.65809428586274,-7.01716745662725,
84.7048954474093));
#50104=CARTESIAN_POINT('Ctrl Pts',(-3.48300199539357,-7.10571030720473,
84.7127895976726));
#50105=CARTESIAN_POINT('Ctrl Pts',(-3.30472616788266,-7.18767736861579,
84.7206837479361));
#50106=CARTESIAN_POINT('Ctrl Pts',(-3.12657784370117,-7.26958580697415,
84.7285722522829));
#50107=CARTESIAN_POINT('Ctrl Pts',(-2.94525083089561,-7.34492768260881,
84.7364607566299));
#50108=CARTESIAN_POINT('Ctrl Pts',(-2.76127182287398,-7.41345391300183,
84.7443492609768));
#50109=CARTESIAN_POINT('Ctrl Pts',(-2.57739022775557,-7.48194386023886,
84.7522335885313));
#50110=CARTESIAN_POINT('Ctrl Pts',(-2.39085975790355,-7.54362523295766,
84.7601179160859));
#50111=CARTESIAN_POINT('Ctrl Pts',(-2.20222768896848,-7.59829679638408,
84.7680022436404));
#50112=CARTESIAN_POINT('Ctrl Pts',(-2.01366046880723,-7.65294956457662,
84.7758838606857));
#50113=CARTESIAN_POINT('Ctrl Pts',(-1.8229934204459,-7.70059723046942,84.783765477731));
#50114=CARTESIAN_POINT('Ctrl Pts',(-1.63078987163276,-7.74108812729709,
84.7916470947762));
#50115=CARTESIAN_POINT('Ctrl Pts',(-1.43858369753527,-7.78157957718489,
84.7995288194755));
#50116=CARTESIAN_POINT('Ctrl Pts',(-1.24484131681875,-7.81491398321496,
84.8074105441748));
#50117=CARTESIAN_POINT('Ctrl Pts',(-1.05013773361246,-7.84099048210386,
84.8152922688741));
#50118=CARTESIAN_POINT('Ctrl Pts',(-0.85542235331027,-7.8670685609686,84.8231744711273));
#50119=CARTESIAN_POINT('Ctrl Pts',(-0.659745996512131,-7.88588780999542,
84.8310566733806));
#50120=CARTESIAN_POINT('Ctrl Pts',(-0.463690335164545,-7.8973990828041,
84.8389388756338));
#50121=CARTESIAN_POINT('Ctrl Pts',(-0.267589804447896,-7.9089129900868,
84.8468228818107));
#50122=CARTESIAN_POINT('Ctrl Pts',(-0.0711101407053061,-7.91311556819726,
84.8547068879876));
#50123=CARTESIAN_POINT('Ctrl Pts',(0.125165180769629,-7.91000977733422,
84.8625908941644));
#50124=CARTESIAN_POINT('Ctrl Pts',(0.321518449630203,-7.90690275305947,
84.8704780313395));
#50125=CARTESIAN_POINT('Ctrl Pts',(0.517666869767976,-7.89648158200195,
84.8783651685144));
#50126=CARTESIAN_POINT('Ctrl Pts',(0.713030041484756,-7.87880125145572,
84.8862523056895));
#50127=CARTESIAN_POINT('Ctrl Pts',(0.908601745483325,-7.86110204877694,
84.8941478616606));
#50128=CARTESIAN_POINT('Ctrl Pts',(1.10338618309347,-7.83612824070503,84.9020434176318));
#50129=CARTESIAN_POINT('Ctrl Pts',(1.29681001872961,-7.80398646688489,84.9099389736029));
#50130=CARTESIAN_POINT('Ctrl Pts',(1.49035170080613,-7.77182511019576,84.9178393400627));
#50131=CARTESIAN_POINT('Ctrl Pts',(1.68253079111909,-7.73248715020807,84.9257397065225));
#50132=CARTESIAN_POINT('Ctrl Pts',(1.87278688468571,-7.68612973378339,84.9336400729823));
#50133=CARTESIAN_POINT('Ctrl Pts',(2.06329078417946,-7.6397119374658,84.94155072956));
#50134=CARTESIAN_POINT('Ctrl Pts',(2.25186635304459,-7.58625651641438,84.9494613861377));
#50135=CARTESIAN_POINT('Ctrl Pts',(2.43796991255272,-7.52596995114169,84.9573720427154));
#50136=CARTESIAN_POINT('Ctrl Pts',(2.51973975202122,-7.49948135104461,84.9608478124436));
#50137=CARTESIAN_POINT('Ctrl Pts',(2.6010326365727,-7.47167459710296,84.9643235821718));
#50138=CARTESIAN_POINT('Ctrl Pts',(2.68180384210392,-7.44257006365924,84.9677993519));
#50139=CARTESIAN_POINT('Ctrl Pts',(2.86396539073789,-7.37693124039904,84.9756381800099));
#50140=CARTESIAN_POINT('Ctrl Pts',(3.0439908152153,-7.30450145393577,84.9834770081197));
#50141=CARTESIAN_POINT('Ctrl Pts',(3.22133083401293,-7.22543761012699,84.9913158362296));
#50142=CARTESIAN_POINT('Ctrl Pts',(3.39847205739639,-7.14646239566245,84.9991458771346));
#50143=CARTESIAN_POINT('Ctrl Pts',(3.57293355134956,-7.06086807350537,85.0069759180395));
#50144=CARTESIAN_POINT('Ctrl Pts',(3.74418145949518,-6.96886118374965,85.0148059589445));
#50145=CARTESIAN_POINT('Ctrl Pts',(3.91527073094477,-6.876939525219,85.0226287464363));
#50146=CARTESIAN_POINT('Ctrl Pts',(4.08315203739093,-6.7786172942189,85.0304515339282));
#50147=CARTESIAN_POINT('Ctrl Pts',(4.24731160023756,-6.67414902219657,85.0382743214201));
#50148=CARTESIAN_POINT('Ctrl Pts',(4.41135102551132,-6.56975720362249,85.046091383929));
#50149=CARTESIAN_POINT('Ctrl Pts',(4.57167383663879,-6.4592284904982,85.0539084464379));
#50150=CARTESIAN_POINT('Ctrl Pts',(4.72779080603319,-6.34286331985705,85.0617255089468));
#50151=CARTESIAN_POINT('Ctrl Pts',(4.88382388087507,-6.22656068184102,85.0695383707018));
#50152=CARTESIAN_POINT('Ctrl Pts',(5.03565533495399,-6.10442804376578,85.0773512324568));
#50153=CARTESIAN_POINT('Ctrl Pts',(5.18282474310586,-5.97680923923875,85.0851640942119));
#50154=CARTESIAN_POINT('Ctrl Pts',(5.32994367522474,-5.84923420529603,85.0929742763185));
#50155=CARTESIAN_POINT('Ctrl Pts',(5.47240348187388,-5.71617698412542,85.1007844584252));
#50156=CARTESIAN_POINT('Ctrl Pts',(5.60977652967726,-5.57802189732903,85.1085946405318));
#50157=CARTESIAN_POINT('Ctrl Pts',(5.74715577309297,-5.43986057964985,85.1164051748827));
#50158=CARTESIAN_POINT('Ctrl Pts',(5.87944754472689,-5.29660117992593,85.1242157092336));
#50159=CARTESIAN_POINT('Ctrl Pts',(6.00626046896467,-5.14866547553366,85.1320262435844));
#50160=CARTESIAN_POINT('Ctrl Pts',(6.13308355737754,-5.00071791395563,85.1398374039569));
#50161=CARTESIAN_POINT('Ctrl Pts',(6.25442669387939,-4.8480935678095,85.1476485643295));
#50162=CARTESIAN_POINT('Ctrl Pts',(6.36993833532186,-4.6912478728156,85.155459724702));
#50163=CARTESIAN_POINT('Ctrl Pts',(6.48547957901117,-4.5343619828689,85.1632728868459));
#50164=CARTESIAN_POINT('Ctrl Pts',(6.59518614180641,-4.37325287230649,85.1710860489898));
#50165=CARTESIAN_POINT('Ctrl Pts',(6.69874933173292,-4.20840568275062,85.1788992111337));
#50166=CARTESIAN_POINT('Ctrl Pts',(6.8023573030043,-4.04348721228066,85.1867157517358));
#50167=CARTESIAN_POINT('Ctrl Pts',(6.89981642268535,-3.87482774060308,85.1945322923379));
#50168=CARTESIAN_POINT('Ctrl Pts',(6.99086346655203,-3.70293788660142,85.20234883294));
#50169=CARTESIAN_POINT('Ctrl Pts',(7.082016763976,-3.53084743401166,85.2101744955873));
#50170=CARTESIAN_POINT('Ctrl Pts',(7.16674287510643,-3.35551938045594,85.2180001582345));
#50171=CARTESIAN_POINT('Ctrl Pts',(7.24482588504999,-3.17748625414961,85.2258258208818));
#50172=CARTESIAN_POINT('Ctrl Pts',(7.32295979200657,-2.99933708013512,85.2336565845472));
#50173=CARTESIAN_POINT('Ctrl Pts',(7.39444183966971,-2.81847964557318,85.2414873482126));
#50174=CARTESIAN_POINT('Ctrl Pts',(7.4591056843464,-2.63546265193633,85.2493181118781));
#50175=CARTESIAN_POINT('Ctrl Pts',(7.5238629614807,-2.45218121798378,85.2571601901738));
#50176=CARTESIAN_POINT('Ctrl Pts',(7.58178225433932,-2.26673432712953,85.2650022684695));
#50177=CARTESIAN_POINT('Ctrl Pts',(7.63274782294268,-2.07968306993249,85.2728443467652));
#50178=CARTESIAN_POINT('Ctrl Pts',(7.66131404305145,-1.97484077088352,85.2772398345591));
#50179=CARTESIAN_POINT('Ctrl Pts',(7.68769660438673,-1.86949459325518,85.281635322353));
#50180=CARTESIAN_POINT('Ctrl Pts',(7.71188224768466,-1.7637440851343,85.2860308101469));
#50181=CARTESIAN_POINT('Ctrl Pts',(7.75544196951926,-1.57328139365785,85.2939473341471));
#50182=CARTESIAN_POINT('Ctrl Pts',(7.7920031200178,-1.38093517548524,85.3018638581474));
#50183=CARTESIAN_POINT('Ctrl Pts',(7.82140203908545,-1.18726203636348,85.3097803821477));
#50184=CARTESIAN_POINT('Ctrl Pts',(7.85076708880784,-0.993812020493328,
85.3176877858301));
#50185=CARTESIAN_POINT('Ctrl Pts',(7.87298629100036,-0.799038465821142,
85.3255951895126));
#50186=CARTESIAN_POINT('Ctrl Pts',(7.88794617865336,-0.603511460262248,
85.333502593195));
#50187=CARTESIAN_POINT('Ctrl Pts',(7.90289160374776,-0.408173481575882,
85.3414023523489));
#50188=CARTESIAN_POINT('Ctrl Pts',(7.91059166837858,-0.212083844154115,
85.3493021115027));
#50189=CARTESIAN_POINT('Ctrl Pts',(7.91098417918274,-0.015821400708789,
85.3572018706566));
#50190=CARTESIAN_POINT('Ctrl Pts',(7.91137638323342,0.180287660496274,85.3650954560222));
#50191=CARTESIAN_POINT('Ctrl Pts',(7.90447241075511,0.376568915716337,85.3729890413879));
#50192=CARTESIAN_POINT('Ctrl Pts',(7.89026197064616,0.572439546655319,85.3808826267536));
#50193=CARTESIAN_POINT('Ctrl Pts',(7.87606000455408,0.768193375368819,85.3887715049902));
#50194=CARTESIAN_POINT('Ctrl Pts',(7.85456027743801,0.963536725033094,85.3966603832268));
#50195=CARTESIAN_POINT('Ctrl Pts',(7.82580457151532,1.15788764932089,85.4045492614634));
#50196=CARTESIAN_POINT('Ctrl Pts',(7.7970606889336,1.35215866330318,85.4124348960691));
#50197=CARTESIAN_POINT('Ctrl Pts',(7.76106682369745,1.5454377247974,85.4203205306747));
#50198=CARTESIAN_POINT('Ctrl Pts',(7.71791654339741,1.73714859155818,85.4282061652804));
#50199=CARTESIAN_POINT('Ctrl Pts',(7.67477010159794,1.92884240437944,85.4360910984071));
#50200=CARTESIAN_POINT('Ctrl Pts',(7.62446858240579,2.11896796295587,85.4439760315338));
#50201=CARTESIAN_POINT('Ctrl Pts',(7.56715665749851,2.30695928028128,85.4518609646605));
#50202=CARTESIAN_POINT('Ctrl Pts',(7.50984493129567,2.4949499458277,85.4597458704496));
#50203=CARTESIAN_POINT('Ctrl Pts',(7.44552294778714,2.68080605496448,85.4676307762388));
#50204=CARTESIAN_POINT('Ctrl Pts',(7.374385276009,2.86397674588702,85.4755156820279));
#50205=CARTESIAN_POINT('Ctrl Pts',(7.30323591565984,3.04717753343177,85.4834018833793));
#50206=CARTESIAN_POINT('Ctrl Pts',(7.22526876041979,3.22769170225382,85.4912880847306));
#50207=CARTESIAN_POINT('Ctrl Pts',(7.14072664268969,3.40498810781795,85.499174286082));
#50208=CARTESIAN_POINT('Ctrl Pts',(7.05615644969819,3.58234339105234,85.5070631063311));
#50209=CARTESIAN_POINT('Ctrl Pts',(6.96500709200787,3.7564784709895,85.5149519265802));
#50210=CARTESIAN_POINT('Ctrl Pts',(6.86756759842163,3.92688633412139,85.5228407468294));
#50211=CARTESIAN_POINT('Ctrl Pts',(6.7700337923989,4.09745913633679,85.5307372027284));
#50212=CARTESIAN_POINT('Ctrl Pts',(6.66619786074414,4.26429721646477,85.5386336586274));
#50213=CARTESIAN_POINT('Ctrl Pts',(6.55639302505851,4.4269212214545,85.5465301145265));
#50214=CARTESIAN_POINT('Ctrl Pts',(6.44652750012939,4.58963510889588,85.5544309348047));
#50215=CARTESIAN_POINT('Ctrl Pts',(6.33068669649665,4.74812999968534,85.5623317550828));
#50216=CARTESIAN_POINT('Ctrl Pts',(6.20924462442865,4.90195901594495,85.570232575361));
#50217=CARTESIAN_POINT('Ctrl Pts',(6.08765498379892,5.05597495528891,85.5781429962057));
#50218=CARTESIAN_POINT('Ctrl Pts',(5.96045070211805,5.20531343325787,85.5860534170503));
#50219=CARTESIAN_POINT('Ctrl Pts',(5.82804392610434,5.34956306583989,85.5939638378949));
#50220=CARTESIAN_POINT('Ctrl Pts',(5.77058461569455,5.41216170817954,85.5973966480612));
#50221=CARTESIAN_POINT('Ctrl Pts',(5.71214600837681,5.47380250434962,85.6008294582275));
#50222=CARTESIAN_POINT('Ctrl Pts',(5.65276374922151,5.53445417322135,85.6042622683938));
#50223=CARTESIAN_POINT('Ctrl Pts',(5.50893384386499,5.68135871874766,85.6125768857281));
#50224=CARTESIAN_POINT('Ctrl Pts',(5.35925051171007,5.8227797783906,85.6208915030624));
#50225=CARTESIAN_POINT('Ctrl Pts',(5.20414811838676,5.95825170346902,85.6292061203967));
#50226=CARTESIAN_POINT('Ctrl Pts',(5.04923742384508,6.09355619204035,85.6375104612809));
#50227=CARTESIAN_POINT('Ctrl Pts',(4.88892124611641,6.22292601884921,85.6458148021651));
#50228=CARTESIAN_POINT('Ctrl Pts',(4.72367087332647,6.34593212069647,85.6541191430492));
#50229=CARTESIAN_POINT('Ctrl Pts',(4.55861381813629,6.46879432426402,85.6624137691278));
#50230=CARTESIAN_POINT('Ctrl Pts',(4.38863431520403,6.58530747682992,85.6707083952064));
#50231=CARTESIAN_POINT('Ctrl Pts',(4.21423746538685,6.69508204470489,85.679003021285));
#50232=CARTESIAN_POINT('Ctrl Pts',(4.04010320400824,6.80469132557839,85.6872851581878));
#50233=CARTESIAN_POINT('Ctrl Pts',(3.86156511659703,6.90758211432676,85.6955672950906));
#50234=CARTESIAN_POINT('Ctrl Pts',(3.67915811983896,7.00340749415761,85.7038494319934));
#50235=CARTESIAN_POINT('Ctrl Pts',(3.49691933794007,7.09914450428193,85.7121239311492));
#50236=CARTESIAN_POINT('Ctrl Pts',(3.31081902033116,7.18782896284675,85.720398430305));
#50237=CARTESIAN_POINT('Ctrl Pts',(3.12141914942105,7.26915837588008,85.7286729294608));
#50238=CARTESIAN_POINT('Ctrl Pts',(2.93223711833086,7.35039424721984,85.7369379116333));
#50239=CARTESIAN_POINT('Ctrl Pts',(2.73976337548252,7.42429183793646,85.7452028938058));
#50240=CARTESIAN_POINT('Ctrl Pts',(2.54458273169738,7.49059541835945,85.7534678759783));
#50241=CARTESIAN_POINT('Ctrl Pts',(2.46657232338421,7.5170958401283,85.7567712498246));
#50242=CARTESIAN_POINT('Ctrl Pts',(2.38812975283229,7.5423836682559,85.7600746236709));
#50243=CARTESIAN_POINT('Ctrl Pts',(2.30929332429207,7.56644469631412,85.7633779975171));
#50244=CARTESIAN_POINT('Ctrl Pts',(2.11201956587983,7.62665302289864,85.7716440870161));
#50245=CARTESIAN_POINT('Ctrl Pts',(1.91250164971992,7.67910807102709,85.7799101765151));
#50246=CARTESIAN_POINT('Ctrl Pts',(1.71136454832781,7.72367479783598,85.7881762660141));
#50247=CARTESIAN_POINT('Ctrl Pts',(1.51004656406251,7.76828160356387,85.7964497892188));
#50248=CARTESIAN_POINT('Ctrl Pts',(1.30710677430522,7.80498586218106,85.8047233124235));
#50249=CARTESIAN_POINT('Ctrl Pts',(1.10317860488045,7.83370397485979,85.8129968356282));
#50250=CARTESIAN_POINT('Ctrl Pts',(0.899053778333808,7.86244978170848,85.8212783373641));
#50251=CARTESIAN_POINT('Ctrl Pts',(0.693938959777478,7.88319402637382,85.8295598391));
#50252=CARTESIAN_POINT('Ctrl Pts',(0.488471766304341,7.89590503574628,85.8378413408359));
#50253=CARTESIAN_POINT('Ctrl Pts',(0.282662474383059,7.90863720867535,85.8461366310937));
#50254=CARTESIAN_POINT('Ctrl Pts',(0.0764999282259149,7.91330938770227,
85.8544319213514));
#50255=CARTESIAN_POINT('Ctrl Pts',(-0.129377135245994,7.90994200717525,
85.8627272116092));
#50256=CARTESIAN_POINT('Ctrl Pts',(-0.335440909823312,7.90657157275125,
85.8710300249139));
#50257=CARTESIAN_POINT('Ctrl Pts',(-0.541218391845821,7.89514703645119,
85.8793328382187));
#50258=CARTESIAN_POINT('Ctrl Pts',(-0.74607558734896,7.8757407409057,85.8876356515234));
#50259=CARTESIAN_POINT('Ctrl Pts',(-0.951246935321723,7.85630468543083,
85.8959511973528));
#50260=CARTESIAN_POINT('Ctrl Pts',(-1.15549488415217,7.82886243844658,85.9042667431822));
#50261=CARTESIAN_POINT('Ctrl Pts',(-1.35819337639028,7.79353782003588,85.9125822890117));
#50262=CARTESIAN_POINT('Ctrl Pts',(-1.43872661315376,7.77950315294666,85.9158861015546));
#50263=CARTESIAN_POINT('Ctrl Pts',(-1.51901540936514,7.76422480033309,85.9191899140976));
#50264=CARTESIAN_POINT('Ctrl Pts',(-1.59902112962635,7.74771272228188,85.9224937266406));
#50265=CARTESIAN_POINT('Ctrl Pts',(-1.79056392623238,7.70818092883787,85.9304034297453));
#50266=CARTESIAN_POINT('Ctrl Pts',(-1.98088258563153,7.66149169908155,85.93831313285));
#50267=CARTESIAN_POINT('Ctrl Pts',(-2.16940300255316,7.60773367123964,85.9462228359547));
#50268=CARTESIAN_POINT('Ctrl Pts',(-2.35773215632278,7.5540301835373,85.9541245142801));
#50269=CARTESIAN_POINT('Ctrl Pts',(-2.54426637299649,7.49327227687575,85.9620261926054));
#50270=CARTESIAN_POINT('Ctrl Pts',(-2.72844080741549,7.42559975762429,85.9699278709308));
#50271=CARTESIAN_POINT('Ctrl Pts',(-2.91246250661091,7.35798335895976,85.9778229964216));
#50272=CARTESIAN_POINT('Ctrl Pts',(-3.09412800047449,7.28346388948508,85.9857181219123));
#50273=CARTESIAN_POINT('Ctrl Pts',(-3.27288642964673,7.20223128055704,85.9936132474031));
#50274=CARTESIAN_POINT('Ctrl Pts',(-3.45152972142404,7.1210509931392,86.0015032876837));
#50275=CARTESIAN_POINT('Ctrl Pts',(-3.62726936653998,7.03316632334309,86.0093933279643));
#50276=CARTESIAN_POINT('Ctrl Pts',(-3.79957309760087,6.93881584104865,86.0172833682449));
#50277=CARTESIAN_POINT('Ctrl Pts',(-3.97179775332592,6.84450865901259,86.02516978755));
#50278=CARTESIAN_POINT('Ctrl Pts',(-4.14058933554998,6.74374174275647,86.0330562068551));
#50279=CARTESIAN_POINT('Ctrl Pts',(-4.30543861381387,6.63680038442324,86.0409426261602));
#50280=CARTESIAN_POINT('Ctrl Pts',(-4.47024275770401,6.52988830575255,86.0488268862288));
#50281=CARTESIAN_POINT('Ctrl Pts',(-4.63110646018127,6.41680534183075,86.0567111462972));
#50282=CARTESIAN_POINT('Ctrl Pts',(-4.78754777132697,6.29788117840137,86.0645954063658));
#50283=CARTESIAN_POINT('Ctrl Pts',(-4.94400734691083,6.17894313064045,86.0724805869174));
#50284=CARTESIAN_POINT('Ctrl Pts',(-5.09604322096018,6.05416272383731,86.0803657674689));
#50285=CARTESIAN_POINT('Ctrl Pts',(-5.24320445367384,5.92391155040104,86.0882509480205));
#50286=CARTESIAN_POINT('Ctrl Pts',(-5.39038404173693,5.79364413079886,86.0961371120869));
#50287=CARTESIAN_POINT('Ctrl Pts',(-5.53268751823247,5.65790481287382,86.1040232761533));
#50288=CARTESIAN_POINT('Ctrl Pts',(-5.66969895078601,5.51710384236657,86.1119094402196));
#50289=CARTESIAN_POINT('Ctrl Pts',(-5.80675046084643,5.37626168586661,86.1197979110847));
#50290=CARTESIAN_POINT('Ctrl Pts',(-5.93850660177277,5.23035517330234,86.1276863819497));
#50291=CARTESIAN_POINT('Ctrl Pts',(-6.06458989786054,5.07982975804975,86.1355748528148));
#50292=CARTESIAN_POINT('Ctrl Pts',(-6.19073122990261,4.92923505617166,86.1434669547313));
#50293=CARTESIAN_POINT('Ctrl Pts',(-6.31119429257198,4.77401747886304,86.1513590566478));
#50294=CARTESIAN_POINT('Ctrl Pts',(-6.4256431690895,4.6146539267353,86.1592511585643));
#50295=CARTESIAN_POINT('Ctrl Pts',(-6.54022472638397,4.45510562417087,86.167152409808));
#50296=CARTESIAN_POINT('Ctrl Pts',(-6.64877796971867,4.29140202617195,86.1750536610516));
#50297=CARTESIAN_POINT('Ctrl Pts',(-6.75101081512904,4.12404825068897,86.1829549122953));
#50298=CARTESIAN_POINT('Ctrl Pts',(-6.85331140301262,3.95658358170001,86.1908613991391));
#50299=CARTESIAN_POINT('Ctrl Pts',(-6.9492830757254,3.7854642130014,86.1987678859829));
#50300=CARTESIAN_POINT('Ctrl Pts',(-7.03868055463757,3.61121822239629,86.2066743728267));
#50301=CARTESIAN_POINT('Ctrl Pts',(-7.12820119341234,3.4367321790232,86.2145917521682));
#50302=CARTESIAN_POINT('Ctrl Pts',(-7.21112940236688,3.25911122110945,86.2225091315097));
#50303=CARTESIAN_POINT('Ctrl Pts',(-7.28726826007096,3.07890277627637,86.2304265108512));
#50304=CARTESIAN_POINT('Ctrl Pts',(-7.32028125772858,3.00076631420494,86.2338594021966));
#50305=CARTESIAN_POINT('Ctrl Pts',(-7.35201849637787,2.92214359411228,86.2372922935419));
#50306=CARTESIAN_POINT('Ctrl Pts',(-7.38246687227592,2.84307999883024,86.2407251848872));
#50307=CARTESIAN_POINT('Ctrl Pts',(-7.46186561464569,2.6369097238164,86.2496769679453));
#50308=CARTESIAN_POINT('Ctrl Pts',(-7.53269619445423,2.42722379759038,86.2586287510035));
#50309=CARTESIAN_POINT('Ctrl Pts',(-7.59467025546627,2.2147019462528,86.2675805340616));
#50310=CARTESIAN_POINT('Ctrl Pts',(-7.65631623356132,2.00330515897866,86.2764849275014));
#50311=CARTESIAN_POINT('Ctrl Pts',(-7.7091991241833,1.78910254853394,86.2853893209411));
#50312=CARTESIAN_POINT('Ctrl Pts',(-7.7530808313697,1.57278689664167,86.2942937143809));
#50313=CARTESIAN_POINT('Ctrl Pts',(-7.79680836482911,1.35723124686413,86.3031668231782));
#50314=CARTESIAN_POINT('Ctrl Pts',(-7.83159774763029,1.13957753073449,86.3120399319754));
#50315=CARTESIAN_POINT('Ctrl Pts',(-7.85726037723687,0.920532652491735,
86.3209130407727));
#50316=CARTESIAN_POINT('Ctrl Pts',(-7.88277750392521,0.702729722930816,
86.3297358404923));
#50317=CARTESIAN_POINT('Ctrl Pts',(-7.89927099049118,0.483551527721885,
86.3385586402119));
#50318=CARTESIAN_POINT('Ctrl Pts',(-7.90660338426671,0.263711819799972,
86.3473814399316));
#50319=CARTESIAN_POINT('Ctrl Pts',(-7.90945314916429,0.178270216156082,
86.3508104572088));
#50320=CARTESIAN_POINT('Ctrl Pts',(-7.91091963434882,0.0927288781526532,
86.354239474486));
#50321=CARTESIAN_POINT('Ctrl Pts',(-7.9109967865903,0.00713039676099505,
86.3576684917632));
#50322=CARTESIAN_POINT('',(-7.91099856105006,-0.0033739488622614,88.3576684917632));
#50323=CARTESIAN_POINT('Ctrl Pts',(-7.911,-4.99544849930089E-12,86.3576684917632));
#50324=CARTESIAN_POINT('Ctrl Pts',(-7.91099999999861,-2.20167589667164,
86.4462559274959));
#50325=CARTESIAN_POINT('Ctrl Pts',(-6.94214576672105,-4.38610418339098,
86.5348433632287));
#50326=CARTESIAN_POINT('Ctrl Pts',(-3.67820201487865,-7.3418068410784,86.7120182346941));
#50327=CARTESIAN_POINT('Ctrl Pts',(-1.40868175871295,-8.08992666571411,
86.8006056704268));
#50328=CARTESIAN_POINT('Ctrl Pts',(2.97309270521675,-7.65454228025098,86.9777805418923));
#50329=CARTESIAN_POINT('Ctrl Pts',(5.0510207267593,-6.47444880833966,87.066367977625));
#50330=CARTESIAN_POINT('Ctrl Pts',(7.66951518848009,-2.93425195367338,87.2435428490904));
#50331=CARTESIAN_POINT('Ctrl Pts',(8.18956872247096,-0.601881960095381,
87.3321302848232));
#50332=CARTESIAN_POINT('Ctrl Pts',(7.32306689761179,3.71537198232766,87.5093051562886));
#50333=CARTESIAN_POINT('Ctrl Pts',(5.94329958849964,5.66643518936756,87.5978925920213));
#50334=CARTESIAN_POINT('Ctrl Pts',(2.1615450163754,7.92205913233078,87.7750674634868));
#50335=CARTESIAN_POINT('Ctrl Pts',(-0.210816529303402,8.20894963712991,
87.8636548992195));
#50336=CARTESIAN_POINT('Ctrl Pts',(-4.42123908576671,6.91982244717678,88.0408297706849));
#50337=CARTESIAN_POINT('Ctrl Pts',(-6.22631625634359,5.35390358803317,88.1294172064177));
#50338=CARTESIAN_POINT('Ctrl Pts',(-7.65317280859594,2.3133485751421,88.264559258688));
#50339=CARTESIAN_POINT('Ctrl Pts',(-7.9110000000007,1.15702837836116,88.3111138752256));
#50340=CARTESIAN_POINT('Ctrl Pts',(-7.911,-4.82447415350862E-12,88.3576684917632));
#50341=CARTESIAN_POINT('',(-7.91099998641113,-0.000451624858829035,90.3576866635156));
#50342=CARTESIAN_POINT('Ctrl Pts',(-7.91099712210012,-0.00674789771969833,
88.3576684917632));
#50343=CARTESIAN_POINT('Ctrl Pts',(-7.91079974958978,-0.238140462654705,
88.3669549096822));
#50344=CARTESIAN_POINT('Ctrl Pts',(-7.90044647194352,-0.469090082543646,
88.3762413276011));
#50345=CARTESIAN_POINT('Ctrl Pts',(-7.88007661870822,-0.698794306851447,
88.3855277455201));
#50346=CARTESIAN_POINT('Ctrl Pts',(-7.85957817621448,-0.929948590495647,
88.3948727860309));
#50347=CARTESIAN_POINT('Ctrl Pts',(-7.82893639447855,-1.15984165263072,
88.4042178265418));
#50348=CARTESIAN_POINT('Ctrl Pts',(-7.78834219788504,-1.38767676662948,
88.4135628670527));
#50349=CARTESIAN_POINT('Ctrl Pts',(-7.74741882746136,-1.6173593702552,88.4229836854588));
#50350=CARTESIAN_POINT('Ctrl Pts',(-7.69638104062731,-1.84495046201203,
88.432404503865));
#50351=CARTESIAN_POINT('Ctrl Pts',(-7.63547284515937,-2.06965587256285,
88.4418253222711));
#50352=CARTESIAN_POINT('Ctrl Pts',(-7.57831964966171,-2.28050815869487,
88.4506653457191));
#50353=CARTESIAN_POINT('Ctrl Pts',(-7.51247604239519,-2.4888197816889,88.4595053691671));
#50354=CARTESIAN_POINT('Ctrl Pts',(-7.43818125172721,-2.69395261028362,
88.4683453926152));
#50355=CARTESIAN_POINT('Ctrl Pts',(-7.37227735286866,-2.87591763187833,
88.4761870192755));
#50356=CARTESIAN_POINT('Ctrl Pts',(-7.29958832600452,-3.05574943342999,
88.4840286459358));
#50357=CARTESIAN_POINT('Ctrl Pts',(-7.22026924162715,-3.23289855677732,
88.4918702725962));
#50358=CARTESIAN_POINT('Ctrl Pts',(-7.14104354949535,-3.40983910037918,
88.4997026663319));
#50359=CARTESIAN_POINT('Ctrl Pts',(-7.05520348569415,-3.5841029378101,88.5075350600677));
#50360=CARTESIAN_POINT('Ctrl Pts',(-6.96295380772239,-3.75515582519878,
88.5153674538035));
#50361=CARTESIAN_POINT('Ctrl Pts',(-6.87079478873815,-3.92604060921923,
88.5231921502019));
#50362=CARTESIAN_POINT('Ctrl Pts',(-6.77223886523992,-4.09372042014354,
88.5310168466004));
#50363=CARTESIAN_POINT('Ctrl Pts',(-6.66753886026993,-4.25768088832293,
88.5388415429989));
#50364=CARTESIAN_POINT('Ctrl Pts',(-6.56292138045455,-4.42151212190496,
88.546660071926));
#50365=CARTESIAN_POINT('Ctrl Pts',(-6.45216965273698,-4.58162955663426,
88.5544786008531));
#50366=CARTESIAN_POINT('Ctrl Pts',(-6.33558250049089,-4.73754317969489,
88.5622971297803));
#50367=CARTESIAN_POINT('Ctrl Pts',(-6.21906457014911,-4.89336423133845,
88.570111016571));
#50368=CARTESIAN_POINT('Ctrl Pts',(-6.09671832684766,-5.04498616234068,
88.5779249033618));
#50369=CARTESIAN_POINT('Ctrl Pts',(-5.96888610478008,-5.19194757948916,
88.5857387901525));
#50370=CARTESIAN_POINT('Ctrl Pts',(-5.8411049285406,-5.33885031215952,88.5935495567102));
#50371=CARTESIAN_POINT('Ctrl Pts',(-5.70784236861505,-5.48109597383794,
88.6013603232679));
#50372=CARTESIAN_POINT('Ctrl Pts',(-5.56948137970588,-5.61825579349227,
88.6091710898256));
#50373=CARTESIAN_POINT('Ctrl Pts',(-5.43112588997301,-5.75541016171094,
88.6169815459433));
#50374=CARTESIAN_POINT('Ctrl Pts',(-5.28767261831783,-5.88747883659304,
88.6247920020611));
#50375=CARTESIAN_POINT('Ctrl Pts',(-5.13954208745199,-6.01406918245123,
88.6326024581788));
#50376=CARTESIAN_POINT('Ctrl Pts',(-4.99140747143296,-6.14066301942602,
88.6404131296938));
#50377=CARTESIAN_POINT('Ctrl Pts',(-4.83859560631866,-6.26177799713768,
88.6482238012088));
#50378=CARTESIAN_POINT('Ctrl Pts',(-4.68156083935325,-6.37706116541421,
88.6560344727238));
#50379=CARTESIAN_POINT('Ctrl Pts',(-4.52449408561535,-6.49236781598418,
88.6638467352124));
#50380=CARTESIAN_POINT('Ctrl Pts',(-4.36320300018651,-6.60184008248953,
88.671658997701));
#50381=CARTESIAN_POINT('Ctrl Pts',(-4.1981718174763,-6.705167737719,88.6794712601896));
#50382=CARTESIAN_POINT('Ctrl Pts',(-4.03307795271457,-6.80853463880069,
88.6872864899274));
#50383=CARTESIAN_POINT('Ctrl Pts',(-3.86424145900895,-6.9057520931507,88.6951017196652));
#50384=CARTESIAN_POINT('Ctrl Pts',(-3.69217224236431,-6.99655523330693,
88.702916949403));
#50385=CARTESIAN_POINT('Ctrl Pts',(-3.51991589209342,-7.08745712628613,
88.7107406785825));
#50386=CARTESIAN_POINT('Ctrl Pts',(-3.34442010821241,-7.17193060794182,
88.718564407762));
#50387=CARTESIAN_POINT('Ctrl Pts',(-3.16621686751772,-7.2497580475383,88.7263881369415));
#50388=CARTESIAN_POINT('Ctrl Pts',(-2.98790550671005,-7.32763270687965,
88.7342166129622));
#50389=CARTESIAN_POINT('Ctrl Pts',(-2.80688374181482,-7.39885315973558,
88.7420450889829));
#50390=CARTESIAN_POINT('Ctrl Pts',(-2.62369994818983,-7.46325127420139,
88.7498735650036));
#50391=CARTESIAN_POINT('Ctrl Pts',(-2.44026404232468,-7.52773801852129,
88.7577128152014));
#50392=CARTESIAN_POINT('Ctrl Pts',(-2.25466049935241,-7.58538356643291,
88.7655520653991));
#50393=CARTESIAN_POINT('Ctrl Pts',(-2.06745027669823,-7.63607034759243,
88.7733913155969));
#50394=CARTESIAN_POINT('Ctrl Pts',(-1.96248841042801,-7.66448855611922,
88.7777864940185));
#50395=CARTESIAN_POINT('Ctrl Pts',(-1.85702165132031,-7.69072025127963,
88.7821816724401));
#50396=CARTESIAN_POINT('Ctrl Pts',(-1.75114965382108,-7.71475183592592,
88.7865768508617));
#50397=CARTESIAN_POINT('Ctrl Pts',(-1.56061467552175,-7.75800083062928,
88.7944867349195));
#50398=CARTESIAN_POINT('Ctrl Pts',(-1.36821932111949,-7.79424541203708,
88.8023966189773));
#50399=CARTESIAN_POINT('Ctrl Pts',(-1.17452109004874,-7.82332545718448,
88.8103065030351));
#50400=CARTESIAN_POINT('Ctrl Pts',(-0.981033441438009,-7.85237388744613,
88.8182077877225));
#50401=CARTESIAN_POINT('Ctrl Pts',(-0.786246075529237,-7.87427324520897,
88.8261090724098));
#50402=CARTESIAN_POINT('Ctrl Pts',(-0.590729610027844,-7.88891371025418,
88.8340103570972));
#50403=CARTESIAN_POINT('Ctrl Pts',(-0.395389372041236,-7.90354097920993,
88.8419045200121));
#50404=CARTESIAN_POINT('Ctrl Pts',(-0.199321685415827,-7.91092236349717,
88.8497986829271));
#50405=CARTESIAN_POINT('Ctrl Pts',(-0.00310555553988154,-7.91099939043891,
88.8576928458421));
#50406=CARTESIAN_POINT('Ctrl Pts',(0.192970166471871,-7.9110763622619,88.865581359871));
#50407=CARTESIAN_POINT('Ctrl Pts',(0.38919377655344,-7.90385939016733,88.8734698738999));
#50408=CARTESIAN_POINT('Ctrl Pts',(0.584982690679458,-7.88934194033985,
88.8813583879289));
#50409=CARTESIAN_POINT('Ctrl Pts',(0.780667865402883,-7.87483218263111,
88.8892427222026));
#50410=CARTESIAN_POINT('Ctrl Pts',(0.975918459923912,-7.85302968045513,
88.8971270564763));
#50411=CARTESIAN_POINT('Ctrl Pts',(1.17015315541674,-7.82397997139999,88.9050113907501));
#50412=CARTESIAN_POINT('Ctrl Pts',(1.36432100322448,-7.79494026007363,88.9128930115565));
#50413=CARTESIAN_POINT('Ctrl Pts',(1.55747330806565,-7.75865836381019,88.9207746323629));
#50414=CARTESIAN_POINT('Ctrl Pts',(1.74903485101827,-7.71523156424507,88.9286562531694));
#50415=CARTESIAN_POINT('Ctrl Pts',(1.94059890292189,-7.67180419590341,88.9365379772043));
#50416=CARTESIAN_POINT('Ctrl Pts',(2.13057181301397,-7.62123180519448,88.9444197012391));
#50417=CARTESIAN_POINT('Ctrl Pts',(2.3183889546336,-7.56366271425643,88.952301425274));
#50418=CARTESIAN_POINT('Ctrl Pts',(2.5062174103923,-7.50609015534577,88.9601836241054));
#50419=CARTESIAN_POINT('Ctrl Pts',(2.69188950870627,-7.4415201569228,88.9680658229368));
#50420=CARTESIAN_POINT('Ctrl Pts',(2.87485614753901,-7.37015082145252,88.9759480217682));
#50421=CARTESIAN_POINT('Ctrl Pts',(3.05786459616895,-7.29876517734005,88.9838320217647));
#50422=CARTESIAN_POINT('Ctrl Pts',(3.23816603190562,-7.22057722556154,88.9917160217612));
#50423=CARTESIAN_POINT('Ctrl Pts',(3.41523146054028,-7.13583317286327,88.9996000217578));
#50424=CARTESIAN_POINT('Ctrl Pts',(3.59236714572668,-7.05105549516566,89.0074871499915));
#50425=CARTESIAN_POINT('Ctrl Pts',(3.76626395433527,-6.95971668199355,89.0153742782252));
#50426=CARTESIAN_POINT('Ctrl Pts',(3.93641740053939,-6.86210893594169,89.0232614064589));
#50427=CARTESIAN_POINT('Ctrl Pts',(4.10675238103278,-6.7643970535752,89.0311569493574));
#50428=CARTESIAN_POINT('Ctrl Pts',(4.27333572252414,-6.66040305084007,89.0390524922559));
#50429=CARTESIAN_POINT('Ctrl Pts',(4.43569091597372,-6.55046312087536,89.0469480351545));
#50430=CARTESIAN_POINT('Ctrl Pts',(4.59814497811076,-6.44045624130255,89.054848386165));
#50431=CARTESIAN_POINT('Ctrl Pts',(4.75636548145493,-6.32449641926763,89.0627487371756));
#50432=CARTESIAN_POINT('Ctrl Pts',(4.90990874665963,-6.20296034966171,89.0706490881862));
#50433=CARTESIAN_POINT('Ctrl Pts',(5.0636519316507,-6.08126603498369,89.0785597257859));
#50434=CARTESIAN_POINT('Ctrl Pts',(5.2127054525779,-5.95398119365958,89.0864703633857));
#50435=CARTESIAN_POINT('Ctrl Pts',(5.35666141948419,-5.82152037160479,89.0943810009854));
#50436=CARTESIAN_POINT('Ctrl Pts',(5.41991267258949,-5.76331984569136,89.0978567703599));
#50437=CARTESIAN_POINT('Ctrl Pts',(5.48218033033942,-5.70412052482345,89.1013325397343));
#50438=CARTESIAN_POINT('Ctrl Pts',(5.54343225297704,-5.64395959027471,89.1048083091088));
#50439=CARTESIAN_POINT('Ctrl Pts',(5.68282425918286,-5.50705036357862,89.1127181745523));
#50440=CARTESIAN_POINT('Ctrl Pts',(5.8173293829207,-5.36478933970217,89.1206280399957));
#50441=CARTESIAN_POINT('Ctrl Pts',(5.94651153067353,-5.21755897097165,89.1285379054392));
#50442=CARTESIAN_POINT('Ctrl Pts',(6.07555328424637,-5.07048861109102,89.1364391745007));
#50443=CARTESIAN_POINT('Ctrl Pts',(6.19928335909494,-4.91845992050672,89.1443404435623));
#50444=CARTESIAN_POINT('Ctrl Pts',(6.31730088897865,-4.76189358114076,89.1522417126239));
#50445=CARTESIAN_POINT('Ctrl Pts',(6.43521208878854,-4.60546830311069,89.1601358628912));
#50446=CARTESIAN_POINT('Ctrl Pts',(6.54742079014679,-4.44451379417601,89.1680300131584));
#50447=CARTESIAN_POINT('Ctrl Pts',(6.65356479037635,-4.27948555088857,89.1759241634256));
#50448=CARTESIAN_POINT('Ctrl Pts',(6.75963287614463,-4.11457533622413,89.1838126677764));
#50449=CARTESIAN_POINT('Ctrl Pts',(6.85964471663764,-3.94559748088743,89.1917011721271));
#50450=CARTESIAN_POINT('Ctrl Pts',(6.95327986994004,-3.7730385699442,89.1995896764778));
#50451=CARTESIAN_POINT('Ctrl Pts',(7.04686544545525,-3.60057102520975,89.2074740040362));
#50452=CARTESIAN_POINT('Ctrl Pts',(7.13408089736744,-3.42452650553766,89.2153583315946));
#50453=CARTESIAN_POINT('Ctrl Pts',(7.21465027456597,-3.24541868111113,89.223242659153));
#50454=CARTESIAN_POINT('Ctrl Pts',(7.2951919532653,-3.06637243116992,89.2311242762021));
#50455=CARTESIAN_POINT('Ctrl Pts',(7.36909196958923,-2.88426528957942,89.2390058932513));
#50456=CARTESIAN_POINT('Ctrl Pts',(7.43612120143288,-2.69963376731,89.2468875103004));
#50457=CARTESIAN_POINT('Ctrl Pts',(7.50315134882047,-2.51499972318162,89.2547692350036));
#50458=CARTESIAN_POINT('Ctrl Pts',(7.56331039846575,-2.32784155079379,89.2626509597068));
#50459=CARTESIAN_POINT('Ctrl Pts',(7.61641789382016,-2.13871444253227,89.27053268441));
#50460=CARTESIAN_POINT('Ctrl Pts',(7.66952860695933,-1.9495758750535,89.2784148866671));
#50461=CARTESIAN_POINT('Ctrl Pts',(7.71558682054423,-1.75846846614513,89.2862970889242));
#50462=CARTESIAN_POINT('Ctrl Pts',(7.75446234995561,-1.56596125849935,89.2941792911814));
#50463=CARTESIAN_POINT('Ctrl Pts',(7.79334677643459,-1.37340999358505,89.3020632973621));
#50464=CARTESIAN_POINT('Ctrl Pts',(7.82504517484067,-1.17945862983582,89.3099473035429));
#50465=CARTESIAN_POINT('Ctrl Pts',(7.84947870008574,-0.984685298407717,
89.3178313097236));
#50466=CARTESIAN_POINT('Ctrl Pts',(7.87392192868729,-0.789834616083665,
89.3257184469025));
#50467=CARTESIAN_POINT('Ctrl Pts',(7.89109449236527,-0.594161657757231,
89.3336055840815));
#50468=CARTESIAN_POINT('Ctrl Pts',(7.90096949066409,-0.398248801122208,
89.3414927212604));
#50469=CARTESIAN_POINT('Ctrl Pts',(7.91085502961861,-0.202126825466925,
89.3493882772354));
#50470=CARTESIAN_POINT('Ctrl Pts',(7.91342742691867,-0.00576478475610737,
89.3572838332104));
#50471=CARTESIAN_POINT('Ctrl Pts',(7.90871191469999,0.190254698450245,89.3651793891855));
#50472=CARTESIAN_POINT('Ctrl Pts',(7.90399352948313,0.38639360953459,89.3730797556492));
#50473=CARTESIAN_POINT('Ctrl Pts',(7.89197840357576,0.582189203546922,89.3809801221129));
#50474=CARTESIAN_POINT('Ctrl Pts',(7.87274359008219,0.777064582142223,89.3888804885765));
#50475=CARTESIAN_POINT('Ctrl Pts',(7.85348372351049,0.972193783218559,89.3967911451581));
#50476=CARTESIAN_POINT('Ctrl Pts',(7.82698543281866,1.16640003399136,89.4047018017396));
#50477=CARTESIAN_POINT('Ctrl Pts',(7.79337696207088,1.35911608299763,89.4126124583212));
#50478=CARTESIAN_POINT('Ctrl Pts',(7.77861013426741,1.44379130467012,89.4160882279993));
#50479=CARTESIAN_POINT('Ctrl Pts',(7.76247131623399,1.52817902287073,89.4195639976774));
#50480=CARTESIAN_POINT('Ctrl Pts',(7.74497441297671,1.61223209940011,89.4230397673555));
#50481=CARTESIAN_POINT('Ctrl Pts',(7.70551402583924,1.80179518328834,89.4308785954659));
#50482=CARTESIAN_POINT('Ctrl Pts',(7.65903031854054,1.99019500384961,89.4387174235763));
#50483=CARTESIAN_POINT('Ctrl Pts',(7.60560166455082,2.17686571018558,89.4465562516867));
#50484=CARTESIAN_POINT('Ctrl Pts',(7.55223290325468,2.36332716155107,89.4543862925922));
#50485=CARTESIAN_POINT('Ctrl Pts',(7.49193479291027,2.54806302366974,89.4622163334977));
#50486=CARTESIAN_POINT('Ctrl Pts',(7.42483701321142,2.73051576213097,89.4700463744032));
#50487=CARTESIAN_POINT('Ctrl Pts',(7.35780139000911,2.91279948422447,89.4778691618957));
#50488=CARTESIAN_POINT('Ctrl Pts',(7.28397876196211,3.09280396682753,89.4856919493881));
#50489=CARTESIAN_POINT('Ctrl Pts',(7.20354914040319,3.26998482898566,89.4935147368806));
#50490=CARTESIAN_POINT('Ctrl Pts',(7.12317837998744,3.44703602413938,89.5013317993901));
#50491=CARTESIAN_POINT('Ctrl Pts',(7.03621040116478,3.62126739576317,89.5091488618996));
#50492=CARTESIAN_POINT('Ctrl Pts',(6.94287410866501,3.79215243776263,89.516965924409));
#50493=CARTESIAN_POINT('Ctrl Pts',(6.84958797347095,3.96294564910262,89.5247787861646));
#50494=CARTESIAN_POINT('Ctrl Pts',(6.74994050990455,4.1303958050917,89.5325916479202));
#50495=CARTESIAN_POINT('Ctrl Pts',(6.64420762769525,4.29399883559326,89.5404045096758));
#50496=CARTESIAN_POINT('Ctrl Pts',(6.53851100965514,4.45754575367403,89.5482146917831));
#50497=CARTESIAN_POINT('Ctrl Pts',(6.42673332223231,4.61724788019711,89.5560248738904));
#50498=CARTESIAN_POINT('Ctrl Pts',(6.30919515940801,4.77262793862066,89.5638350559977));
#50499=CARTESIAN_POINT('Ctrl Pts',(6.1916516955372,4.92801500478449,89.5716455903491));
#50500=CARTESIAN_POINT('Ctrl Pts',(6.0683474420616,5.07907932728141,89.5794561247006));
#50501=CARTESIAN_POINT('Ctrl Pts',(5.93964516069064,5.22537427990419,89.5872666590521));
#50502=CARTESIAN_POINT('Ctrl Pts',(5.81093256371075,5.37168095820506,89.5950778194253));
#50503=CARTESIAN_POINT('Ctrl Pts',(5.67682130887087,5.51321724027827,89.6028889797984));
#50504=CARTESIAN_POINT('Ctrl Pts',(5.53771306666677,5.64957122189535,89.6107001401716));
#50505=CARTESIAN_POINT('Ctrl Pts',(5.39856917509871,5.78596014704015,89.6185133023162));
#50506=CARTESIAN_POINT('Ctrl Pts',(5.25442599636751,5.91716387967365,89.6263264644607));
#50507=CARTESIAN_POINT('Ctrl Pts',(5.10572061940688,6.04280878040696,89.6341396266053));
#50508=CARTESIAN_POINT('Ctrl Pts',(4.95695094134949,6.16850801074881,89.641956167208));
#50509=CARTESIAN_POINT('Ctrl Pts',(4.80361540382972,6.28864339410337,89.6497727078107));
#50510=CARTESIAN_POINT('Ctrl Pts',(4.64618269403846,6.40288273933058,89.6575892484134));
#50511=CARTESIAN_POINT('Ctrl Pts',(4.48856625740856,6.51725540395358,89.6654149110613));
#50512=CARTESIAN_POINT('Ctrl Pts',(4.32684338332908,6.62571808083098,89.6732405737092));
#50513=CARTESIAN_POINT('Ctrl Pts',(4.16151108263852,6.7279823505325,89.6810662363572));
#50514=CARTESIAN_POINT('Ctrl Pts',(3.99607101304628,6.83031327936826,89.6888970000232));
#50515=CARTESIAN_POINT('Ctrl Pts',(3.8270171330316,6.92643757614659,89.6967277636893));
#50516=CARTESIAN_POINT('Ctrl Pts',(3.65486941463108,7.01611363662207,89.7045585273554));
#50517=CARTESIAN_POINT('Ctrl Pts',(3.48247296087428,7.10591926957787,89.7124006056518));
#50518=CARTESIAN_POINT('Ctrl Pts',(3.30697405670186,7.18925790678759,89.7202426839482));
#50519=CARTESIAN_POINT('Ctrl Pts',(3.12891203323844,7.2659363118772,89.7280847622445));
#50520=CARTESIAN_POINT('Ctrl Pts',(3.02910820322112,7.30891458629368,89.7324802500305));
#50521=CARTESIAN_POINT('Ctrl Pts',(2.92849942072416,7.34980137541722,89.7368757378164));
#50522=CARTESIAN_POINT('Ctrl Pts',(2.82718239294255,7.388569598849,89.7412712256024));
#50523=CARTESIAN_POINT('Ctrl Pts',(2.64470465191667,7.45839337862535,89.7491877496008));
#50524=CARTESIAN_POINT('Ctrl Pts',(2.45938110114356,7.52155164713901,89.7571042735993));
#50525=CARTESIAN_POINT('Ctrl Pts',(2.27173991503261,7.57780434944369,89.7650207975978));
#50526=CARTESIAN_POINT('Ctrl Pts',(2.08431490299651,7.63399224520918,89.7729282012784));
#50527=CARTESIAN_POINT('Ctrl Pts',(1.89457790064729,7.68329032293475,89.7808356049591));
#50528=CARTESIAN_POINT('Ctrl Pts',(1.70307746622446,7.72550633577104,89.7887430086398));
#50529=CARTESIAN_POINT('Ctrl Pts',(1.51176216596351,7.7676815360307,89.7966427677918));
#50530=CARTESIAN_POINT('Ctrl Pts',(1.31868716380311,7.80278823657131,89.8045425269438));
#50531=CARTESIAN_POINT('Ctrl Pts',(1.12441688244685,7.83068372969235,89.8124422860958));
#50532=CARTESIAN_POINT('Ctrl Pts',(0.93029842642419,7.85855742203913,89.8203358714597));
#50533=CARTESIAN_POINT('Ctrl Pts',(0.734986891740987,7.87923108619266,89.8282294568235));
#50534=CARTESIAN_POINT('Ctrl Pts',(0.539057901824469,7.89261284863768,89.8361230421874));
#50535=CARTESIAN_POINT('Ctrl Pts',(0.343245748935179,7.90598663122559,89.8440119204221));
#50536=CARTESIAN_POINT('Ctrl Pts',(0.146817217275051,7.91207715313049,89.8519007986569));
#50537=CARTESIAN_POINT('Ctrl Pts',(-0.0496456348362537,7.91084422239129,
89.8597896768916));
#50538=CARTESIAN_POINT('Ctrl Pts',(-0.246027708291441,7.90961179859011,
89.8676753114954));
#50539=CARTESIAN_POINT('Ctrl Pts',(-0.442443730037354,7.90106192539069,
89.8755609460992));
#50540=CARTESIAN_POINT('Ctrl Pts',(-0.638310031637585,7.88520648451966,
89.8834465807031));
#50541=CARTESIAN_POINT('Ctrl Pts',(-0.8341589096448,7.86935245409415,89.8913315138279));
#50542=CARTESIAN_POINT('Ctrl Pts',(-1.02945782110312,7.84619417212444,89.8992164469528));
#50543=CARTESIAN_POINT('Ctrl Pts',(-1.22362608918042,7.81579555732345,89.9071013800777));
#50544=CARTESIAN_POINT('Ctrl Pts',(-1.41779368406282,7.78539704791658,89.914986285865));
#50545=CARTESIAN_POINT('Ctrl Pts',(-1.61083030271615,7.74775830845246,89.9228711916522));
#50546=CARTESIAN_POINT('Ctrl Pts',(-1.80216325093471,7.70299478235449,89.9307560974395));
#50547=CARTESIAN_POINT('Ctrl Pts',(-1.99352763690808,7.65822390119942,89.938642298789));
#50548=CARTESIAN_POINT('Ctrl Pts',(-2.18318745903772,7.60632597932667,89.9465285001384));
#50549=CARTESIAN_POINT('Ctrl Pts',(-2.37058278149718,7.54746701059826,89.9544147014879));
#50550=CARTESIAN_POINT('Ctrl Pts',(-2.55804033533732,7.48858849562483,89.9623035217351));
#50551=CARTESIAN_POINT('Ctrl Pts',(-2.7432315625057,7.42274443108365,89.9701923419824));
#50552=CARTESIAN_POINT('Ctrl Pts',(-2.92561394544023,7.35014993331739,89.9780811622297));
#50553=CARTESIAN_POINT('Ctrl Pts',(-3.10817285768912,7.27748517077714,89.9859776181269));
#50554=CARTESIAN_POINT('Ctrl Pts',(-3.28791717490341,7.19805705172566,89.9938740740241));
#50555=CARTESIAN_POINT('Ctrl Pts',(-3.46432557319129,7.11212832582012,90.0017705299213));
#50556=CARTESIAN_POINT('Ctrl Pts',(-3.64083147257813,7.02615210702144,90.0096713501976));
#50557=CARTESIAN_POINT('Ctrl Pts',(-3.81399747353355,6.93366827984826,90.0175721704739));
#50558=CARTESIAN_POINT('Ctrl Pts',(-3.98332869013005,6.83498453153969,90.0254729907502));
#50559=CARTESIAN_POINT('Ctrl Pts',(-4.15286566708425,6.73618086911392,90.033383411593));
#50560=CARTESIAN_POINT('Ctrl Pts',(-4.31855826141697,6.63116242099108,90.0412938324358));
#50561=CARTESIAN_POINT('Ctrl Pts',(-4.47994138578039,6.52027960903304,90.0492042532786));
#50562=CARTESIAN_POINT('Ctrl Pts',(-4.5499752872436,6.47216084842989,90.0526370634688));
#50563=CARTESIAN_POINT('Ctrl Pts',(-4.61919804849276,6.42293821132822,90.0560698736589));
#50564=CARTESIAN_POINT('Ctrl Pts',(-4.68757370137022,6.37264260681723,90.0595026838491));
#50565=CARTESIAN_POINT('Ctrl Pts',(-4.85318652508569,6.25082150920415,90.0678173011866));
#50566=CARTESIAN_POINT('Ctrl Pts',(-5.01419036393472,6.12243622989692,90.076131918524));
#50567=CARTESIAN_POINT('Ctrl Pts',(-5.17006328744622,5.98785158498445,90.0844465358615));
#50568=CARTESIAN_POINT('Ctrl Pts',(-5.32574355983871,5.85343327994589,90.0927508767487));
#50569=CARTESIAN_POINT('Ctrl Pts',(-5.47630534384549,5.7128310816791,90.101055217636));
#50570=CARTESIAN_POINT('Ctrl Pts',(-5.62125775855654,5.56645149191726,90.1093595585233));
#50571=CARTESIAN_POINT('Ctrl Pts',(-5.76604060116759,5.42024314383142,90.117654184605));
#50572=CARTESIAN_POINT('Ctrl Pts',(-5.90522695718064,5.26827109222717,90.1259488106867));
#50573=CARTESIAN_POINT('Ctrl Pts',(-6.03836034606067,5.11098085802735,90.1342434367684));
#50574=CARTESIAN_POINT('Ctrl Pts',(-6.1712932766807,4.9539274549255,90.1425255736742));
#50575=CARTESIAN_POINT('Ctrl Pts',(-6.29819123942203,4.7915720726692,90.15080771058));
#50576=CARTESIAN_POINT('Ctrl Pts',(-6.41863577121813,4.62439572662625,90.1590898474858));
#50577=CARTESIAN_POINT('Ctrl Pts',(-6.53896922964461,4.4573735498079,90.1673643466447));
#50578=CARTESIAN_POINT('Ctrl Pts',(-6.65286095413846,4.28553951206331,90.1756388458036));
#50579=CARTESIAN_POINT('Ctrl Pts',(-6.75993267263712,4.1094076533502,90.1839133449624));
#50580=CARTESIAN_POINT('Ctrl Pts',(-6.86688124171569,3.933478374147,90.1921783271379));
#50581=CARTESIAN_POINT('Ctrl Pts',(-6.96702530521538,3.75326138778045,90.2004433093133));
#50582=CARTESIAN_POINT('Ctrl Pts',(-7.06002969432137,3.5692998914774,90.2087082914887));
#50583=CARTESIAN_POINT('Ctrl Pts',(-7.09720197834301,3.49577358744641,90.2120116653167));
#50584=CARTESIAN_POINT('Ctrl Pts',(-7.13323420630645,3.42164943754332,90.2153150391446));
#50585=CARTESIAN_POINT('Ctrl Pts',(-7.16810694353174,3.34696337686747,90.2186184129726));
#50586=CARTESIAN_POINT('Ctrl Pts',(-7.25289334992292,3.16537847140652,90.2266499361086));
#50587=CARTESIAN_POINT('Ctrl Pts',(-7.33074559233991,2.98063483199827,90.2346814592445));
#50588=CARTESIAN_POINT('Ctrl Pts',(-7.40144652869959,2.79329738531379,90.2427129823805));
#50589=CARTESIAN_POINT('Ctrl Pts',(-7.47218534022186,2.60585958018117,90.2507488080797));
#50590=CARTESIAN_POINT('Ctrl Pts',(-7.53576509030279,2.41582550177319,90.2587846337788));
#50591=CARTESIAN_POINT('Ctrl Pts',(-7.5920182070502,2.22377619013655,90.266820459478));
#50592=CARTESIAN_POINT('Ctrl Pts',(-7.64834272464466,2.03148311452171,90.2748664848744));
#50593=CARTESIAN_POINT('Ctrl Pts',(-7.69732193257746,1.83717000750674,90.2829125102708));
#50594=CARTESIAN_POINT('Ctrl Pts',(-7.7388388401238,1.6414305975555,90.2909585356672));
#50595=CARTESIAN_POINT('Ctrl Pts',(-7.78038381628874,1.44555885272749,90.2990100007949));
#50596=CARTESIAN_POINT('Ctrl Pts',(-7.81445637095806,1.24825920224464,90.3070614659225));
#50597=CARTESIAN_POINT('Ctrl Pts',(-7.84099122394232,1.05013219456386,90.3151129310502));
#50598=CARTESIAN_POINT('Ctrl Pts',(-7.86756582474199,0.851708403036846,
90.3231764568495));
#50599=CARTESIAN_POINT('Ctrl Pts',(-7.88658012332793,0.652455101885583,
90.3312399826488));
#50600=CARTESIAN_POINT('Ctrl Pts',(-7.89802086058761,0.452976252934894,
90.3393035084481));
#50601=CARTESIAN_POINT('Ctrl Pts',(-7.90668697854369,0.301875218490092,
90.3454114597219));
#50602=CARTESIAN_POINT('Ctrl Pts',(-7.91100865671468,0.150644818809502,
90.3515194109957));
#50603=CARTESIAN_POINT('Ctrl Pts',(-7.91099998697758,-0.000453917034045954,
90.3576273622695));
#50604=CARTESIAN_POINT('',(-7.91348203759552,0.000837024955133735,92.3578223768916));
#50605=CARTESIAN_POINT('Ctrl Pts',(-7.91099998641113,-0.000451624858829035,
90.3576866635156));
#50606=CARTESIAN_POINT('Ctrl Pts',(-7.91086750422562,-2.20197461812199,
90.4462680419976));
#50607=CARTESIAN_POINT('Ctrl Pts',(-6.94203417908043,-4.38620523289174,
90.5348494204795));
#50608=CARTESIAN_POINT('Ctrl Pts',(-3.67820201487802,-7.34180684107875,
90.7120182346941));
#50609=CARTESIAN_POINT('Ctrl Pts',(-1.40868175871207,-8.08992666571431,
90.8006056704269));
#50610=CARTESIAN_POINT('Ctrl Pts',(2.97309270521788,-7.65454228025058,90.9777805418923));
#50611=CARTESIAN_POINT('Ctrl Pts',(5.0510207267604,-6.47444880833885,91.066367977625));
#50612=CARTESIAN_POINT('Ctrl Pts',(7.66951518848072,-2.93425195367184,91.2435428490905));
#50613=CARTESIAN_POINT('Ctrl Pts',(8.18956872247113,-0.601881960093553,
91.3321302848232));
#50614=CARTESIAN_POINT('Ctrl Pts',(7.32306689761086,3.71537198232957,91.5093051562887));
#50615=CARTESIAN_POINT('Ctrl Pts',(5.94329958849807,5.66643518936925,91.5978925920214));
#50616=CARTESIAN_POINT('Ctrl Pts',(2.16154501637291,7.9220591323315,91.7750674634869));
#50617=CARTESIAN_POINT('Ctrl Pts',(-0.210816529306171,8.20894963712988,
91.8636548992196));
#50618=CARTESIAN_POINT('Ctrl Pts',(-4.42123908576931,6.91982244717516,92.040829770685));
#50619=CARTESIAN_POINT('Ctrl Pts',(-6.22631625634573,5.35390358803074,92.1294172064178));
#50620=CARTESIAN_POINT('Ctrl Pts',(-7.65305292437075,2.31360404201413,92.2645479040777));
#50621=CARTESIAN_POINT('Ctrl Pts',(-7.91087421866498,1.15759242186707,92.3110911660047));
#50622=CARTESIAN_POINT('Ctrl Pts',(-7.91099995398858,0.00084659301766466,
92.3576344279319));
#50623=CARTESIAN_POINT('',(-7.89534346295974,0.00069161415478913,94.3576955927382));
#50624=CARTESIAN_POINT('Ctrl Pts',(-7.9137082678045,0.000836152871381276,
92.3578395075525));
#50625=CARTESIAN_POINT('Ctrl Pts',(-7.90855828367506,-0.731198149654099,
92.3873058786017));
#50626=CARTESIAN_POINT('Ctrl Pts',(-7.60962963928138,-2.78494886841547,
92.4698108260254));
#50627=CARTESIAN_POINT('Ctrl Pts',(-5.22373353997936,-6.99284294143041,
92.6583929261981));
#50628=CARTESIAN_POINT('Ctrl Pts',(1.91752129298265,-9.16215704951927,92.9235858080707));
#50629=CARTESIAN_POINT('Ctrl Pts',(8.74828639842495,-3.32800690420377,93.2418172663172));
#50630=CARTESIAN_POINT('Ctrl Pts',(7.52558118799366,5.55410540008025,93.560048724564));
#50631=CARTESIAN_POINT('Ctrl Pts',(-0.601507980866756,9.34057455472231,
93.8782801828113));
#50632=CARTESIAN_POINT('Ctrl Pts',(-6.94138208571764,5.32395168258709,94.1441534385439));
#50633=CARTESIAN_POINT('Ctrl Pts',(-7.89629725284548,1.34085654164704,94.3039495415281));
#50634=CARTESIAN_POINT('Ctrl Pts',(-7.89534399850304,0.00136738064416724,
94.3576684917632));
#50635=CARTESIAN_POINT('',(-7.91175229129129,-4.45848290299239E-5,96.3563650965844));
#50636=CARTESIAN_POINT('Ctrl Pts',(-7.89534292741644,1.58476654102983E-5,
94.3577226937131));
#50637=CARTESIAN_POINT('Ctrl Pts',(-7.89534100553285,-0.00218476492922217,
94.3578109471868));
#50638=CARTESIAN_POINT('Ctrl Pts',(-7.89533858281069,-0.00411872059818796,
94.3578885065983));
#50639=CARTESIAN_POINT('Ctrl Pts',(-7.89533499935064,-0.00631604597571947,
94.357976628182));
#50640=CARTESIAN_POINT('Ctrl Pts',(-7.89494973591493,-0.242553959490402,
94.3674507184937));
#50641=CARTESIAN_POINT('Ctrl Pts',(-7.8841455758433,-0.479166263720991,
94.376708057421));
#50642=CARTESIAN_POINT('Ctrl Pts',(-7.86299604179089,-0.71502109617178,
94.3858293751233));
#50643=CARTESIAN_POINT('Ctrl Pts',(-7.8417777960691,-0.951642185658164,
94.3949803266211));
#50644=CARTESIAN_POINT('Ctrl Pts',(-7.81014756052766,-1.18750036699406,
94.403994371633));
#50645=CARTESIAN_POINT('Ctrl Pts',(-7.76821154680769,-1.42149411747968,
94.4129530297179));
#50646=CARTESIAN_POINT('Ctrl Pts',(-7.72630123746556,-1.65534444317972,
94.4219061966579));
#50647=CARTESIAN_POINT('Ctrl Pts',(-7.67409852972891,-1.88733229461253,
94.4308040445481));
#50648=CARTESIAN_POINT('Ctrl Pts',(-7.61173028829981,-2.1164056968663,94.4397279431391));
#50649=CARTESIAN_POINT('Ctrl Pts',(-7.54951510244527,-2.34491693862951,
94.4486299419236));
#50650=CARTESIAN_POINT('Ctrl Pts',(-7.47718496765697,-2.57052786406193,
94.4575578637056));
#50651=CARTESIAN_POINT('Ctrl Pts',(-7.39487531212015,-2.79224511439129,
94.466592480645));
#50652=CARTESIAN_POINT('Ctrl Pts',(-7.31283718645635,-3.01323094558839,
94.4755972934457));
#50653=CARTESIAN_POINT('Ctrl Pts',(-7.22088601136339,-3.23034875908435,
94.4847080986156));
#50654=CARTESIAN_POINT('Ctrl Pts',(-7.11915418516265,-3.44266666809989,
94.4940048715749));
#50655=CARTESIAN_POINT('Ctrl Pts',(-7.0699761682239,-3.54530292379201,94.4984990094976));
#50656=CARTESIAN_POINT('Ctrl Pts',(-7.01851247856327,-3.64681829260696,
94.5030366050537));
#50657=CARTESIAN_POINT('Ctrl Pts',(-6.96477715111767,-3.74711178296017,
94.5076266926376));
#50658=CARTESIAN_POINT('Ctrl Pts',(-6.85450764867543,-3.95292263040759,
94.5170459461921));
#50659=CARTESIAN_POINT('Ctrl Pts',(-6.73467378089451,-4.15358522068934,
94.5266862466224));
#50660=CARTESIAN_POINT('Ctrl Pts',(-6.60615843297703,-4.34865370677128,
94.5366256641826));
#50661=CARTESIAN_POINT('Ctrl Pts',(-6.48405065385526,-4.53399639150189,
94.5460695183502));
#50662=CARTESIAN_POINT('Ctrl Pts',(-6.3541058958454,-4.71428950597768,94.5557834062116));
#50663=CARTESIAN_POINT('Ctrl Pts',(-6.21705650342287,-4.88918645561241,
94.5658342931876));
#50664=CARTESIAN_POINT('Ctrl Pts',(-6.10664964088334,-5.03008327489469,
94.5739312783484));
#50665=CARTESIAN_POINT('Ctrl Pts',(-5.99137346960744,-5.1670881326108,94.5819830907967));
#50666=CARTESIAN_POINT('Ctrl Pts',(-5.87141429726191,-5.29988137000902,
94.589879209913));
#50667=CARTESIAN_POINT('Ctrl Pts',(-5.75157619366024,-5.43254058588864,
94.5977673598745));
#50668=CARTESIAN_POINT('Ctrl Pts',(-5.62706391422946,-5.56099639982551,
94.6055001306122));
#50669=CARTESIAN_POINT('Ctrl Pts',(-5.49808382191283,-5.68488255749942,
94.612967335798));
#50670=CARTESIAN_POINT('Ctrl Pts',(-5.43572154205482,-5.74478190395382,
94.6165777529655));
#50671=CARTESIAN_POINT('Ctrl Pts',(-5.37231516452397,-5.80361229321,94.6201260874695));
#50672=CARTESIAN_POINT('Ctrl Pts',(-5.30789038223661,-5.86132864337651,
94.6235998848297));
#50673=CARTESIAN_POINT('Ctrl Pts',(-5.08342662142632,-6.06241941246647,
94.6357030164522));
#50674=CARTESIAN_POINT('Ctrl Pts',(-4.84723506706229,-6.25108700614638,
94.6476322608195));
#50675=CARTESIAN_POINT('Ctrl Pts',(-4.60109727133566,-6.42610935418111,
94.6594544706515));
#50676=CARTESIAN_POINT('Ctrl Pts',(-4.50680645297714,-6.49315716525988,
94.6639833396803));
#50677=CARTESIAN_POINT('Ctrl Pts',(-4.41105590223857,-6.55820305847355,
94.6684965012432));
#50678=CARTESIAN_POINT('Ctrl Pts',(-4.31394518764209,-6.62118026040317,
94.6729977136483));
#50679=CARTESIAN_POINT('Ctrl Pts',(-4.05854234315178,-6.78681138131193,
94.6848359794534));
#50680=CARTESIAN_POINT('Ctrl Pts',(-3.79373341421565,-6.93813033637002,
94.6965915930514));
#50681=CARTESIAN_POINT('Ctrl Pts',(-3.5214291932744,-7.07413416149846,94.7083329248413));
#50682=CARTESIAN_POINT('Ctrl Pts',(-3.24875448172607,-7.21032303017695,
94.7200902316062));
#50683=CARTESIAN_POINT('Ctrl Pts',(-2.96856483070124,-7.33115582289544,
94.7318332176736));
#50684=CARTESIAN_POINT('Ctrl Pts',(-2.68274243446052,-7.43566256934059,
94.7436305328917));
#50685=CARTESIAN_POINT('Ctrl Pts',(-2.39793828801589,-7.53979700775578,
94.7553858198644));
#50686=CARTESIAN_POINT('Ctrl Pts',(-2.10754195593512,-7.62772242160117,
94.7671950495793));
#50687=CARTESIAN_POINT('Ctrl Pts',(-1.81337008770093,-7.69850348437741,
94.7791261407947));
#50688=CARTESIAN_POINT('Ctrl Pts',(-1.52167118980876,-7.76868952265293,
94.7909569327025));
#50689=CARTESIAN_POINT('Ctrl Pts',(-1.22626018781794,-7.82201924741345,
94.8029075458534));
#50690=CARTESIAN_POINT('Ctrl Pts',(-0.928858225085867,-7.85759046373914,
94.8150442004776));
#50691=CARTESIAN_POINT('Ctrl Pts',(-0.824197036538944,-7.87010862516789,
94.8193153111532));
#50692=CARTESIAN_POINT('Ctrl Pts',(-0.719288805131689,-7.88042747494532,
94.8236094624102));
#50693=CARTESIAN_POINT('Ctrl Pts',(-0.614207000587532,-7.88850761447765,
94.8279295403805));
#50694=CARTESIAN_POINT('Ctrl Pts',(-0.321228819834413,-7.91103582086582,
94.8399743333869));
#50695=CARTESIAN_POINT('Ctrl Pts',(-0.0269049073670538,-7.91616263996339,
94.8522206671931));
#50696=CARTESIAN_POINT('Ctrl Pts',(0.267116403962486,-7.90475530100067,
94.8647310935471));
#50697=CARTESIAN_POINT('Ctrl Pts',(0.438879687916884,-7.898091287455,94.872039515867));
#50698=CARTESIAN_POINT('Ctrl Pts',(0.610540626108601,-7.88578434077762,
94.8794380660752));
#50699=CARTESIAN_POINT('Ctrl Pts',(0.781778134030084,-7.86800393038236,
94.8869392149633));
#50700=CARTESIAN_POINT('Ctrl Pts',(0.990272335153488,-7.84635497913328,
94.8960724128468));
#50701=CARTESIAN_POINT('Ctrl Pts',(1.19769759054455,-7.81605049268673,94.9050024100971));
#50702=CARTESIAN_POINT('Ctrl Pts',(1.4035102551961,-7.77751410296379,94.9137855452439));
#50703=CARTESIAN_POINT('Ctrl Pts',(1.61153801110222,-7.73856295927029,94.9226632102676));
#50704=CARTESIAN_POINT('Ctrl Pts',(1.81791877285403,-7.69120199890053,94.931390834923));
#50705=CARTESIAN_POINT('Ctrl Pts',(2.02212431683724,-7.63582626547788,94.9400265964449));
#50706=CARTESIAN_POINT('Ctrl Pts',(2.22898882802423,-7.5797294827821,94.9487748045058));
#50707=CARTESIAN_POINT('Ctrl Pts',(2.43362168331101,-7.5154080927409,94.9574287415523));
#50708=CARTESIAN_POINT('Ctrl Pts',(2.63549947541872,-7.44322580125453,94.9660488871222));
#50709=CARTESIAN_POINT('Ctrl Pts',(2.75827799668934,-7.39932580156614,94.9712915079928));
#50710=CARTESIAN_POINT('Ctrl Pts',(2.88003792388024,-7.35251723702134,94.9765216298747));
#50711=CARTESIAN_POINT('Ctrl Pts',(3.00066460806138,-7.30287304158761,94.9817528581273));
#50712=CARTESIAN_POINT('Ctrl Pts',(3.25249594460139,-7.19923126305081,94.9926740503292));
#50713=CARTESIAN_POINT('Ctrl Pts',(3.499365700582,-7.08278886020871,95.0033667402724));
#50714=CARTESIAN_POINT('Ctrl Pts',(3.73986399801828,-6.95426081533967,95.0139265904244));
#50715=CARTESIAN_POINT('Ctrl Pts',(3.98899794096346,-6.82111767487423,95.0248656163275));
#50716=CARTESIAN_POINT('Ctrl Pts',(4.23129481725793,-6.6750066424291,95.035662091327));
#50717=CARTESIAN_POINT('Ctrl Pts',(4.46524258947272,-6.51670421475433,95.046422357286));
#50718=CARTESIAN_POINT('Ctrl Pts',(4.691060121441,-6.36390317209562,95.0568086784686));
#50719=CARTESIAN_POINT('Ctrl Pts',(4.90909972038032,-6.1997441618502,95.0671612635803));
#50720=CARTESIAN_POINT('Ctrl Pts',(5.11804272480831,-6.02489396212108,95.0775757484205));
#50721=CARTESIAN_POINT('Ctrl Pts',(5.32415330391685,-5.85241402663785,95.0878490548056));
#50722=CARTESIAN_POINT('Ctrl Pts',(5.52141317268533,-5.66953150135819,95.0981825940724));
#50723=CARTESIAN_POINT('Ctrl Pts',(5.7085837663623,-5.47684411697809,95.108668165197));
#50724=CARTESIAN_POINT('Ctrl Pts',(5.88994050679585,-5.29014194722298,95.1188280357375));
#50725=CARTESIAN_POINT('Ctrl Pts',(6.06182604291708,-5.09423494806226,95.1291306400588));
#50726=CARTESIAN_POINT('Ctrl Pts',(6.22312501876962,-4.88961927936072,95.1396594857775));
#50727=CARTESIAN_POINT('Ctrl Pts',(6.25109883642619,-4.85413311848659,95.1414854862758));
#50728=CARTESIAN_POINT('Ctrl Pts',(6.27875424423695,-4.81838489689965,95.1433182915265));
#50729=CARTESIAN_POINT('Ctrl Pts',(6.30608542407995,-4.78237703912036,95.1451583371284));
#50730=CARTESIAN_POINT('Ctrl Pts',(6.32526741042165,-4.75710545406317,95.1464497460542));
#50731=CARTESIAN_POINT('Ctrl Pts',(6.34428969055677,-4.73170597803243,95.1477447213798));
#50732=CARTESIAN_POINT('Ctrl Pts',(6.36315210291656,-4.70618089701231,95.1490434136937));
#50733=CARTESIAN_POINT('Ctrl Pts',(6.50744063091238,-4.5109261068446,95.1589777952948));
#50734=CARTESIAN_POINT('Ctrl Pts',(6.64197303335215,-4.30883982975102,95.1690924217835));
#50735=CARTESIAN_POINT('Ctrl Pts',(6.76661025656409,-4.100890200801,95.1793029581414));
#50736=CARTESIAN_POINT('Ctrl Pts',(6.89623385261474,-3.8846211119425,95.1899219883654));
#50737=CARTESIAN_POINT('Ctrl Pts',(7.01515418370291,-3.66200912270891,95.2006447561186));
#50738=CARTESIAN_POINT('Ctrl Pts',(7.12316187524308,-3.43416186488374,95.2113763940341));
#50739=CARTESIAN_POINT('Ctrl Pts',(7.23238618389855,-3.20374809656665,95.222228914955));
#50740=CARTESIAN_POINT('Ctrl Pts',(7.33044977485948,-2.9679796290668,95.2330905069936));
#50741=CARTESIAN_POINT('Ctrl Pts',(7.41709369809658,-2.72803464773274,95.2438630607299));
#50742=CARTESIAN_POINT('Ctrl Pts',(7.5040678757603,-2.48717508532628,95.2546766754365));
#50743=CARTESIAN_POINT('Ctrl Pts',(7.57953421124156,-2.24210651772726,95.2654005717852));
#50744=CARTESIAN_POINT('Ctrl Pts',(7.64320198233374,-1.99406408260649,95.2759355142046));
#50745=CARTESIAN_POINT('Ctrl Pts',(7.66664902386801,-1.90271706073385,95.2798152358947));
#50746=CARTESIAN_POINT('Ctrl Pts',(7.68849568765391,-1.81096717658473,95.2836693308816));
#50747=CARTESIAN_POINT('Ctrl Pts',(7.70872687526107,-1.71887781026362,95.2874928426938));
#50748=CARTESIAN_POINT('Ctrl Pts',(7.75898361138552,-1.49011659896288,95.2969909121075));
#50749=CARTESIAN_POINT('Ctrl Pts',(7.79954659050739,-1.25928664176328,95.3064578422713));
#50750=CARTESIAN_POINT('Ctrl Pts',(7.83026459247564,-1.02719205262028,95.3158665627013));
#50751=CARTESIAN_POINT('Ctrl Pts',(7.86070706604573,-0.797179260673331,
95.3251908906089));
#50752=CARTESIAN_POINT('Ctrl Pts',(7.88148014767695,-0.565923622146464,
95.3344580483361));
#50753=CARTESIAN_POINT('Ctrl Pts',(7.89238767747411,-0.334220330441234,
95.3436416873198));
#50754=CARTESIAN_POINT('Ctrl Pts',(7.9031503468454,-0.105594237527625,95.3527033604799));
#50755=CARTESIAN_POINT('Ctrl Pts',(7.90430751752217,0.123468375233821,95.3616837185523));
#50756=CARTESIAN_POINT('Ctrl Pts',(7.89562647892617,0.352180447046821,95.3705574488811));
#50757=CARTESIAN_POINT('Ctrl Pts',(7.88717230511806,0.574915501814209,95.3791992787378));
#50758=CARTESIAN_POINT('Ctrl Pts',(7.8693871037499,0.797318582573102,95.3877399811137));
#50759=CARTESIAN_POINT('Ctrl Pts',(7.84201791527239,1.01863228290947,95.3961561764574));
#50760=CARTESIAN_POINT('Ctrl Pts',(7.81972748646366,1.19887793709816,95.403010621678));
#50761=CARTESIAN_POINT('Ctrl Pts',(7.79107922300819,1.37840056851073,95.409782480812));
#50762=CARTESIAN_POINT('Ctrl Pts',(7.75591905237436,1.55677219662619,95.4164591237919));
#50763=CARTESIAN_POINT('Ctrl Pts',(7.70399925959459,1.8201673338681,95.4263182886859));
#50764=CARTESIAN_POINT('Ctrl Pts',(7.63898456107242,2.08058599369728,95.4365195678523));
#50765=CARTESIAN_POINT('Ctrl Pts',(7.56051601014418,2.33664673504757,95.4469859602393));
#50766=CARTESIAN_POINT('Ctrl Pts',(7.52068164815656,2.46663532463033,95.4522991979393));
#50767=CARTESIAN_POINT('Ctrl Pts',(7.47738015587361,2.59549999938065,95.4576807568967));
#50768=CARTESIAN_POINT('Ctrl Pts',(7.43056524834723,2.72305495898814,95.463120563543));
#50769=CARTESIAN_POINT('Ctrl Pts',(7.33699259977474,2.97800911867122,95.4739935341951));
#50770=CARTESIAN_POINT('Ctrl Pts',(7.22938209043632,3.22773380596663,95.4850992111801));
#50771=CARTESIAN_POINT('Ctrl Pts',(7.10875465450052,3.47122856406998,95.4963571534699));
#50772=CARTESIAN_POINT('Ctrl Pts',(6.98745956561423,3.71607102547493,95.5076774066124));
#50773=CARTESIAN_POINT('Ctrl Pts',(6.85300226629674,3.95461386141648,95.5191516152508));
#50774=CARTESIAN_POINT('Ctrl Pts',(6.70644811440811,4.18579495424151,95.530697995267));
#50775=CARTESIAN_POINT('Ctrl Pts',(6.5591113642813,4.41821055263064,95.542306032879));
#50776=CARTESIAN_POINT('Ctrl Pts',(6.39954757251653,4.64318485801121,95.5539870147162));
#50777=CARTESIAN_POINT('Ctrl Pts',(6.22887775388047,4.85960282968115,95.5656578394716));
#50778=CARTESIAN_POINT('Ctrl Pts',(6.05843496404739,5.07573291733362,95.5773131394353));
#50779=CARTESIAN_POINT('Ctrl Pts',(5.8769152431992,5.2833285187262,95.5889583093217));
#50780=CARTESIAN_POINT('Ctrl Pts',(5.68548149276933,5.48125562332238,95.6005105790124));
#50781=CARTESIAN_POINT('Ctrl Pts',(5.49590911641781,5.67725821679619,95.6119505221394));
#50782=CARTESIAN_POINT('Ctrl Pts',(5.29661439405186,5.86377840795389,95.6232993628868));
#50783=CARTESIAN_POINT('Ctrl Pts',(5.08877650123915,6.03970626308767,95.6344767221404));
#50784=CARTESIAN_POINT('Ctrl Pts',(4.9435858722972,6.16260529554803,95.6422849605611));
#50785=CARTESIAN_POINT('Ctrl Pts',(4.79422715432221,6.28033496272848,95.6500095144926));
#50786=CARTESIAN_POINT('Ctrl Pts',(4.64111741998645,6.39251848315742,95.6576229817758));
#50787=CARTESIAN_POINT('Ctrl Pts',(4.50985051667586,6.48869775871474,95.664150302054));
#50788=CARTESIAN_POINT('Ctrl Pts',(4.37573012004144,6.5810382843292,95.6706810766281));
#50789=CARTESIAN_POINT('Ctrl Pts',(4.2388122776661,6.6692204070492,95.6771207269103));
#50790=CARTESIAN_POINT('Ctrl Pts',(4.17603526051647,6.70965203038073,95.6800733153326));
#50791=CARTESIAN_POINT('Ctrl Pts',(4.11267048510002,6.74920882288298,95.6830067472875));
#50792=CARTESIAN_POINT('Ctrl Pts',(4.04872521441862,6.78785680626155,95.6859119065566));
#50793=CARTESIAN_POINT('Ctrl Pts',(3.8594739302814,6.90223868948401,95.6945099641839));
#50794=CARTESIAN_POINT('Ctrl Pts',(3.66522601748946,7.00886792686582,95.7029934026401));
#50795=CARTESIAN_POINT('Ctrl Pts',(3.46675775369528,7.10714538394219,95.7114238857058));
#50796=CARTESIAN_POINT('Ctrl Pts',(3.2690302159716,7.20505604849865,95.7198229044031));
#50797=CARTESIAN_POINT('Ctrl Pts',(3.06711452315287,7.29467719512274,95.728169362254));
#50798=CARTESIAN_POINT('Ctrl Pts',(2.86177508594341,7.37546778374205,95.7365242351857));
#50799=CARTESIAN_POINT('Ctrl Pts',(2.65822634073895,7.45555382644906,95.7448062482501));
#50800=CARTESIAN_POINT('Ctrl Pts',(2.4513139447209,7.52696280965348,95.7530965302653));
#50801=CARTESIAN_POINT('Ctrl Pts',(2.24176898568361,7.5892168383936,95.7614544757817));
#50802=CARTESIAN_POINT('Ctrl Pts',(2.07152115430481,7.63979602405519,95.7682450094481));
#50803=CARTESIAN_POINT('Ctrl Pts',(1.89953544225083,7.68433299485283,95.7750802076896));
#50804=CARTESIAN_POINT('Ctrl Pts',(1.72619315043018,7.72259443194149,95.7819919241935));
#50805=CARTESIAN_POINT('Ctrl Pts',(1.51152103309105,7.76997850437985,95.7905515942011));
#50806=CARTESIAN_POINT('Ctrl Pts',(1.29476966977163,7.80773694119226,95.7992286207526));
#50807=CARTESIAN_POINT('Ctrl Pts',(1.07680296937618,7.83621616594034,95.808083506307));
#50808=CARTESIAN_POINT('Ctrl Pts',(0.858510041804163,7.86473801507583,95.816951644823));
#50809=CARTESIAN_POINT('Ctrl Pts',(0.638998681851458,7.88395354531904,95.8259981751378));
#50810=CARTESIAN_POINT('Ctrl Pts',(0.419097366059129,7.89424503100409,95.8352838717764));
#50811=CARTESIAN_POINT('Ctrl Pts',(0.200450360998181,7.9044778143531,95.8445166030705));
#50812=CARTESIAN_POINT('Ctrl Pts',(-0.0185817889182326,7.90588874189786,
95.8539857800743));
#50813=CARTESIAN_POINT('Ctrl Pts',(-0.237230341947614,7.89887720199766,
95.8637511432652));
#50814=CARTESIAN_POINT('Ctrl Pts',(-0.274561099084255,7.89768009326064,
95.8654184234579));
#50815=CARTESIAN_POINT('Ctrl Pts',(-0.311880789818695,7.8962375108515,95.8670943375142));
#50816=CARTESIAN_POINT('Ctrl Pts',(-0.349185733300582,7.89455149027729,
95.8687791827576));
#50817=CARTESIAN_POINT('Ctrl Pts',(-0.538494228772429,7.88599557279161,
95.8773291358834));
#50818=CARTESIAN_POINT('Ctrl Pts',(-0.72735735993748,7.87030059175063,95.8856029470287));
#50819=CARTESIAN_POINT('Ctrl Pts',(-0.915345549147819,7.84777852947421,
95.8936804113027));
#50820=CARTESIAN_POINT('Ctrl Pts',(-1.10475219890014,7.8250865274968,95.9018188238969));
#50821=CARTESIAN_POINT('Ctrl Pts',(-1.29327105689764,7.79546439524873,95.9097579153795));
#50822=CARTESIAN_POINT('Ctrl Pts',(-1.4805043442638,7.7591980005021,95.9175793007997));
#50823=CARTESIAN_POINT('Ctrl Pts',(-1.66924469039254,7.72263969405132,95.9254636413045));
#50824=CARTESIAN_POINT('Ctrl Pts',(-1.85667916095413,7.67933010587731,95.933228373266));
#50825=CARTESIAN_POINT('Ctrl Pts',(-2.04243577504038,7.62952283008212,95.9409570984214));
#50826=CARTESIAN_POINT('Ctrl Pts',(-2.13273456251568,7.60531084369404,95.9447141356267));
#50827=CARTESIAN_POINT('Ctrl Pts',(-2.22263734885794,7.57956279034144,95.9484626641976));
#50828=CARTESIAN_POINT('Ctrl Pts',(-2.31210385396676,7.55230409462123,95.9522122876043));
#50829=CARTESIAN_POINT('Ctrl Pts',(-2.52277369089802,7.4881171122936,95.9610416539766));
#50830=CARTESIAN_POINT('Ctrl Pts',(-2.73113406439668,7.41506052231833,95.9696350598388));
#50831=CARTESIAN_POINT('Ctrl Pts',(-2.93628257126045,7.33347201603543,95.9780772240315));
#50832=CARTESIAN_POINT('Ctrl Pts',(-3.14175621895565,7.25175419974598,95.9865327682499));
#50833=CARTESIAN_POINT('Ctrl Pts',(-3.34400753884291,7.16147815677355,95.9948365910117));
#50834=CARTESIAN_POINT('Ctrl Pts',(-3.5421783994591,7.06300229683345,96.0030738146103));
#50835=CARTESIAN_POINT('Ctrl Pts',(-3.7400392144396,6.96468050601582,96.0112981507681));
#50836=CARTESIAN_POINT('Ctrl Pts',(-3.93383221393402,6.85818527569541,96.0194560959933));
#50837=CARTESIAN_POINT('Ctrl Pts',(-4.12275452664767,6.74388114006049,96.0276323736732));
#50838=CARTESIAN_POINT('Ctrl Pts',(-4.31122247602586,6.62985190900183,96.0357889871814));
#50839=CARTESIAN_POINT('Ctrl Pts',(-4.49484316467593,6.508051989285,96.0439638450702));
#50840=CARTESIAN_POINT('Ctrl Pts',(-4.67287117856765,6.3788402829317,96.0522410609095));
#50841=CARTESIAN_POINT('Ctrl Pts',(-4.85040866823104,6.24998459623601,96.0604954703667));
#50842=CARTESIAN_POINT('Ctrl Pts',(-5.02238441735062,6.11375856238643,96.0688516744936));
#50843=CARTESIAN_POINT('Ctrl Pts',(-5.18810922960627,5.97050501405808,96.0773930934946));
#50844=CARTESIAN_POINT('Ctrl Pts',(-5.31644066140156,5.85957453408643,96.0840072662008));
#50845=CARTESIAN_POINT('Ctrl Pts',(-5.44102482967134,5.7444298897345,96.0907325012597));
#50846=CARTESIAN_POINT('Ctrl Pts',(-5.56156121099912,5.62522120200396,96.0976075340458));
#50847=CARTESIAN_POINT('Ctrl Pts',(-5.71925048114818,5.46926886000907,96.1066016559065));
#50848=CARTESIAN_POINT('Ctrl Pts',(-5.87001100066274,5.30636278252122,96.1158521513142));
#50849=CARTESIAN_POINT('Ctrl Pts',(-6.01376735822492,5.13738654839755,96.1254457483515));
#50850=CARTESIAN_POINT('Ctrl Pts',(-6.15752371578701,4.96841031427398,96.1350393453888));
#50851=CARTESIAN_POINT('Ctrl Pts',(-6.29427647074201,4.79336454690273,96.1449760440555));
#50852=CARTESIAN_POINT('Ctrl Pts',(-6.4239862901908,4.61308959593157,96.155342572434));
#50853=CARTESIAN_POINT('Ctrl Pts',(-6.55088879474878,4.43671634304658,96.1654847376177));
#50854=CARTESIAN_POINT('Ctrl Pts',(-6.66981469275507,4.25476027087685,96.1752518688182));
#50855=CARTESIAN_POINT('Ctrl Pts',(-6.78067563690051,4.06803364556051,96.1846930936941));
#50856=CARTESIAN_POINT('Ctrl Pts',(-6.89419944722437,3.87682186977934,96.1943610956247));
#50857=CARTESIAN_POINT('Ctrl Pts',(-6.99926676695183,3.68060738080236,96.2036873467384));
#50858=CARTESIAN_POINT('Ctrl Pts',(-7.09577185797243,3.48020914404722,96.2127246005285));
#50859=CARTESIAN_POINT('Ctrl Pts',(-7.11542939169053,3.43938917222604,96.2145654373095));
#50860=CARTESIAN_POINT('Ctrl Pts',(-7.13473161541277,3.39839544573362,96.2163942832001));
#50861=CARTESIAN_POINT('Ctrl Pts',(-7.15367754904318,3.3572346392387,96.2182115840493));
#50862=CARTESIAN_POINT('Ctrl Pts',(-7.25200300283662,3.14361861713775,96.2276429973625));
#50863=CARTESIAN_POINT('Ctrl Pts',(-7.34116641750469,2.9258357364677,96.2370648513991));
#50864=CARTESIAN_POINT('Ctrl Pts',(-7.4209725176741,2.7046873025448,96.2464754577597));
#50865=CARTESIAN_POINT('Ctrl Pts',(-7.50120798246339,2.48234906843032,96.2559366941024));
#50866=CARTESIAN_POINT('Ctrl Pts',(-7.57198539139196,2.25660814656931,96.2653865614164));
#50867=CARTESIAN_POINT('Ctrl Pts',(-7.63305716512908,2.0282612805973,96.2748233439042));
#50868=CARTESIAN_POINT('Ctrl Pts',(-7.69358059489057,1.8019646682965,96.2841753965322));
#50869=CARTESIAN_POINT('Ctrl Pts',(-7.74457199343469,1.57310788518565,96.2935145982482));
#50870=CARTESIAN_POINT('Ctrl Pts',(-7.78574009386206,1.34246146366351,96.3028392790578));
#50871=CARTESIAN_POINT('Ctrl Pts',(-7.82577159118107,1.1181829201079,96.3119065163351));
#50872=CARTESIAN_POINT('Ctrl Pts',(-7.8565146589521,0.892211509128002,96.320960023448));
#50873=CARTESIAN_POINT('Ctrl Pts',(-7.87765371442561,0.66526191660585,96.3299982649382));
#50874=CARTESIAN_POINT('Ctrl Pts',(-7.89824468402497,0.44419659199532,96.3388021661338));
#50875=CARTESIAN_POINT('Ctrl Pts',(-7.90972315218024,0.222202594470807,
96.3475915830478));
#50876=CARTESIAN_POINT('Ctrl Pts',(-7.91175229129129,-4.45848290304383E-5,
96.3563650965844));
#50877=CARTESIAN_POINT('',(-7.91868362782468,0.00154658286907643,98.357726602302));
#50878=CARTESIAN_POINT('Ctrl Pts',(-7.911,-4.14168699336415E-12,96.3576684917632));
#50879=CARTESIAN_POINT('Ctrl Pts',(-7.91099999999885,-2.20167589667079,
96.4462559274959));
#50880=CARTESIAN_POINT('Ctrl Pts',(-6.94214576672153,-4.38610418339023,
96.5348433632286));
#50881=CARTESIAN_POINT('Ctrl Pts',(-3.67820201487944,-7.341806841078,96.7120182346941));
#50882=CARTESIAN_POINT('Ctrl Pts',(-1.40868175871382,-8.08992666571396,
96.8006056704268));
#50883=CARTESIAN_POINT('Ctrl Pts',(2.97309270521593,-7.6545422802513,96.9777805418923));
#50884=CARTESIAN_POINT('Ctrl Pts',(5.0510207267586,-6.47444880834021,97.066367977625));
#50885=CARTESIAN_POINT('Ctrl Pts',(7.66951518847978,-2.9342519536742,97.2435428490904));
#50886=CARTESIAN_POINT('Ctrl Pts',(8.1895687224709,-0.601881960096264,97.3321302848231));
#50887=CARTESIAN_POINT('Ctrl Pts',(7.32306689761219,3.71537198232687,97.5093051562886));
#50888=CARTESIAN_POINT('Ctrl Pts',(5.94329958850025,5.66643518936691,97.5978925920213));
#50889=CARTESIAN_POINT('Ctrl Pts',(2.16154501637625,7.92205913233055,97.7750674634867));
#50890=CARTESIAN_POINT('Ctrl Pts',(-0.210816529302517,8.20894963712994,
97.8636548992195));
#50891=CARTESIAN_POINT('Ctrl Pts',(-4.42123908576597,6.91982244717725,98.0408297706849));
#50892=CARTESIAN_POINT('Ctrl Pts',(-6.22631625634301,5.35390358803384,98.1294172064176));
#50893=CARTESIAN_POINT('Ctrl Pts',(-7.65294787893378,2.31382788822453,98.2645379548953));
#50894=CARTESIAN_POINT('Ctrl Pts',(-7.91076398318387,1.15808663968023,98.3110712676403));
#50895=CARTESIAN_POINT('Ctrl Pts',(-7.91099983803092,0.00158839793129274,
98.3576045803853));
#50896=CARTESIAN_POINT('',(-7.90591968225023,0.00541017765921074,100.357667186137));
#50897=CARTESIAN_POINT('Ctrl Pts',(-7.92261381100118,0.00152519487455055,
98.3577890153166));
#50898=CARTESIAN_POINT('Ctrl Pts',(-7.90753284617846,-2.42511318705542,
98.4557766957155));
#50899=CARTESIAN_POINT('Ctrl Pts',(-5.41078064749634,-7.50661730602548,
98.6598415288631));
#50900=CARTESIAN_POINT('Ctrl Pts',(1.74919137803737,-8.55146619143505,98.9169449383855));
#50901=CARTESIAN_POINT('Ctrl Pts',(6.19343569208429,-5.41096699287904,99.1290992438833));
#50902=CARTESIAN_POINT('Ctrl Pts',(8.70888107749104,-0.585350218599905,
99.3412535493814));
#50903=CARTESIAN_POINT('Ctrl Pts',(6.64946598043916,6.58836944045884,99.6064464312537));
#50904=CARTESIAN_POINT('Ctrl Pts',(-1.95996707955373,9.15241355656713,99.9246778895003));
#50905=CARTESIAN_POINT('Ctrl Pts',(-7.30433020370274,4.54693693773015,100.175084447898));
#50906=CARTESIAN_POINT('Ctrl Pts',(-7.90728284534243,0.958428727150744,
100.319413853548));
#50907=CARTESIAN_POINT('Ctrl Pts',(-7.90172002473078,0.00543421965308875,
100.357666106448));
#50908=CARTESIAN_POINT('',(-7.90607670224956,-0.00557672470292666,102.357669804003));
#50909=CARTESIAN_POINT('Ctrl Pts',(-7.91099816987171,0.00538110458176591,
100.357668491763));
#50910=CARTESIAN_POINT('Ctrl Pts',(-7.91113279599411,-0.192538670395385,
100.365603511931));
#50911=CARTESIAN_POINT('Ctrl Pts',(-7.90383567542204,-0.390497577918663,
100.3735385321));
#50912=CARTESIAN_POINT('Ctrl Pts',(-7.88912477896871,-0.587904092401064,
100.381473552268));
#50913=CARTESIAN_POINT('Ctrl Pts',(-7.8744106177791,-0.78535441660042,100.389410333427));
#50914=CARTESIAN_POINT('Ctrl Pts',(-7.85227941295536,-0.982251765136944,
100.397347114585));
#50915=CARTESIAN_POINT('Ctrl Pts',(-7.8228011557655,-1.17800809732108,100.405283895744));
#50916=CARTESIAN_POINT('Ctrl Pts',(-7.79331752937729,-1.37380008475337,
100.413222122516));
#50917=CARTESIAN_POINT('Ctrl Pts',(-7.75648423295182,-1.56845030693343,
100.421160349288));
#50918=CARTESIAN_POINT('Ctrl Pts',(-7.71242270003436,-1.76137931632989,
100.429098576059));
#50919=CARTESIAN_POINT('Ctrl Pts',(-7.66834613799111,-1.95437413265946,
100.437039510513));
#50920=CARTESIAN_POINT('Ctrl Pts',(-7.61703649998356,-2.1456462362215,100.444980444966));
#50921=CARTESIAN_POINT('Ctrl Pts',(-7.5586656439331,-2.33462945308789,100.45292137942));
#50922=CARTESIAN_POINT('Ctrl Pts',(-7.50026559888049,-2.52370717313441,
100.460866284827));
#50923=CARTESIAN_POINT('Ctrl Pts',(-7.43479739679541,-2.71049340213586,
100.468811190233));
#50924=CARTESIAN_POINT('Ctrl Pts',(-7.36248186594788,-2.89443980306875,
100.47675609564));
#50925=CARTESIAN_POINT('Ctrl Pts',(-7.29007834870731,-3.07861001180806,
100.484710667623));
#50926=CARTESIAN_POINT('Ctrl Pts',(-7.2108109822883,-3.25993317470558,100.492665239606));
#50927=CARTESIAN_POINT('Ctrl Pts',(-7.12494814906543,-3.4378823239211,100.500619811589));
#50928=CARTESIAN_POINT('Ctrl Pts',(-7.03902685184802,-3.61595263869448,
100.508579799839));
#50929=CARTESIAN_POINT('Ctrl Pts',(-6.94650129016071,-3.79064406045562,
100.516539788089));
#50930=CARTESIAN_POINT('Ctrl Pts',(-6.84768462299399,-3.96145633624955,
100.524499776339));
#50931=CARTESIAN_POINT('Ctrl Pts',(-6.74872617033783,-4.13251369926226,
100.532471185849));
#50932=CARTESIAN_POINT('Ctrl Pts',(-6.64345875685786,-4.29968051032878,
100.540442595359));
#50933=CARTESIAN_POINT('Ctrl Pts',(-6.53223824768452,-4.46248635577606,
100.548414004869));
#50934=CARTESIAN_POINT('Ctrl Pts',(-6.47304832652731,-4.54912923511173,
100.55265627191));
#50935=CARTESIAN_POINT('Ctrl Pts',(-6.41217304298212,-4.63453756222787,
100.556898538952));
#50936=CARTESIAN_POINT('Ctrl Pts',(-6.34967046958094,-4.71864450109687,
100.561140805994));
#50937=CARTESIAN_POINT('Ctrl Pts',(-6.23417869960183,-4.87405664989205,
100.568979634104));
#50938=CARTESIAN_POINT('Ctrl Pts',(-6.11280331819254,-5.02546089097958,
100.576818462214));
#50939=CARTESIAN_POINT('Ctrl Pts',(-5.98585330647374,-5.17237674511219,
100.584657290325));
#50940=CARTESIAN_POINT('Ctrl Pts',(-5.85904560375187,-5.31912790884777,
100.59248733123));
#50941=CARTESIAN_POINT('Ctrl Pts',(-5.72667594144932,-5.4614004408611,100.600317372136));
#50942=CARTESIAN_POINT('Ctrl Pts',(-5.58909635740859,-5.59874297566891,
100.608147413041));
#50943=CARTESIAN_POINT('Ctrl Pts',(-5.4516442211758,-5.73595828226101,100.615970200534));
#50944=CARTESIAN_POINT('Ctrl Pts',(-5.30899202155895,-5.86825243977816,
100.623792988026));
#50945=CARTESIAN_POINT('Ctrl Pts',(-5.16153193549735,-5.99520717563964,
100.631615775518));
#50946=CARTESIAN_POINT('Ctrl Pts',(-5.01417976576146,-6.12206900169079,
100.639432838028));
#50947=CARTESIAN_POINT('Ctrl Pts',(-4.86202698290902,-6.24359896041867,
100.647249900537));
#50948=CARTESIAN_POINT('Ctrl Pts',(-4.70550261323149,-6.35941555151664,
100.655066963047));
#50949=CARTESIAN_POINT('Ctrl Pts',(-4.54906235703669,-6.47516990478636,
100.662879824802));
#50950=CARTESIAN_POINT('Ctrl Pts',(-4.38825547572164,-6.58521679778036,
100.670692686558));
#50951=CARTESIAN_POINT('Ctrl Pts',(-4.22354421412487,-6.68921484715003,
100.678505548314));
#50952=CARTESIAN_POINT('Ctrl Pts',(-4.058889445049,-6.79317722736192,100.686315730421));
#50953=CARTESIAN_POINT('Ctrl Pts',(-3.89033326087425,-6.89109470995801,
100.694125912528));
#50954=CARTESIAN_POINT('Ctrl Pts',(-3.71836718741699,-6.98266900687271,
100.701936094636));
#50955=CARTESIAN_POINT('Ctrl Pts',(-3.54639335817967,-7.07424743384685,
100.709746628987));
#50956=CARTESIAN_POINT('Ctrl Pts',(-3.37100963855793,-7.15948193008002,
100.717557163339));
#50957=CARTESIAN_POINT('Ctrl Pts',(-3.19273293070338,-7.23811974432602,
100.72536769769));
#50958=CARTESIAN_POINT('Ctrl Pts',(-3.01444193380339,-7.31676386146663,
100.733178858063));
#50959=CARTESIAN_POINT('Ctrl Pts',(-2.83325780852366,-7.38881010053658,
100.740990018436));
#50960=CARTESIAN_POINT('Ctrl Pts',(-2.64971816473443,-7.45405357154592,
100.74880117881));
#50961=CARTESIAN_POINT('Ctrl Pts',(-2.46613148511572,-7.51931376254399,
100.756614340954));
#50962=CARTESIAN_POINT('Ctrl Pts',(-2.28018841600672,-7.57776759459709,
100.764427503099));
#50963=CARTESIAN_POINT('Ctrl Pts',(-2.0924426186994,-7.62925978633907,100.772240665243));
#50964=CARTESIAN_POINT('Ctrl Pts',(-1.90461563898359,-7.6807742436135,100.780057205846));
#50965=CARTESIAN_POINT('Ctrl Pts',(-1.714984717257,-7.7253209710461,100.787873746449));
#50966=CARTESIAN_POINT('Ctrl Pts',(-1.5241147617666,-7.76279557846045,100.795690287051));
#50967=CARTESIAN_POINT('Ctrl Pts',(-1.33302205756247,-7.80031391942405,
100.803515949699));
#50968=CARTESIAN_POINT('Ctrl Pts',(-1.14068777687912,-7.83074358833103,
100.811341612347));
#50969=CARTESIAN_POINT('Ctrl Pts',(-0.94768412697614,-7.85403181782946,
100.819167274995));
#50970=CARTESIAN_POINT('Ctrl Pts',(-0.754554671097795,-7.87733522734353,
100.826998038661));
#50971=CARTESIAN_POINT('Ctrl Pts',(-0.560755325868441,-7.893487891755,100.834828802327));
#50972=CARTESIAN_POINT('Ctrl Pts',(-0.366859452539099,-7.90248917380358,
100.842659565993));
#50973=CARTESIAN_POINT('Ctrl Pts',(-0.172683420055691,-7.91150346175847,
100.85050164429));
#50974=CARTESIAN_POINT('Ctrl Pts',(0.0215890686840955,-7.91334572567888,
100.858343722586));
#50975=CARTESIAN_POINT('Ctrl Pts',(0.215387419524853,-7.90806735299532,
100.866185800883));
#50976=CARTESIAN_POINT('Ctrl Pts',(0.324011466864043,-7.90510882315353,
100.870581288669));
#50977=CARTESIAN_POINT('Ctrl Pts',(0.432486683125326,-7.89991420106491,
100.874976776455));
#50978=CARTESIAN_POINT('Ctrl Pts',(0.540713937046143,-7.89249956846905,
100.879372264241));
#50979=CARTESIAN_POINT('Ctrl Pts',(0.735637389148293,-7.87914539260949,
100.88728878824));
#50980=CARTESIAN_POINT('Ctrl Pts',(0.930340983616197,-7.85854695445958,
100.895205312238));
#50981=CARTESIAN_POINT('Ctrl Pts',(1.12424456805213,-7.83070847057948,100.903121836237));
#50982=CARTESIAN_POINT('Ctrl Pts',(1.31792476374908,-7.80290205832833,100.911029239917));
#50983=CARTESIAN_POINT('Ctrl Pts',(1.51080644751213,-7.76787226248475,100.918936643598));
#50984=CARTESIAN_POINT('Ctrl Pts',(1.7023110689238,-7.72567524716251,100.926844047279));
#50985=CARTESIAN_POINT('Ctrl Pts',(1.89363055212579,-7.68351902605094,100.934743806431));
#50986=CARTESIAN_POINT('Ctrl Pts',(2.08357529084069,-7.63420946189932,100.942643565583));
#50987=CARTESIAN_POINT('Ctrl Pts',(2.27157316497154,-7.57785433722378,100.950543324735));
#50988=CARTESIAN_POINT('Ctrl Pts',(2.45942411575497,-7.5215432549801,100.958436910099));
#50989=CARTESIAN_POINT('Ctrl Pts',(2.64533090474981,-7.45819768074241,100.966330495463));
#50990=CARTESIAN_POINT('Ctrl Pts',(2.82873261822868,-7.3879762299678,100.974224080826));
#50991=CARTESIAN_POINT('Ctrl Pts',(3.01202496498791,-7.31779665388221,100.982112959061));
#50992=CARTESIAN_POINT('Ctrl Pts',(3.19281489196223,-7.24074949421967,100.990001837296));
#50993=CARTESIAN_POINT('Ctrl Pts',(3.37055737228734,-7.15704296480882,100.997890715531));
#50994=CARTESIAN_POINT('Ctrl Pts',(3.54822677111899,-7.07337085259622,101.005776350135));
#50995=CARTESIAN_POINT('Ctrl Pts',(3.72285090922833,-6.98304497413313,101.013661984738));
#50996=CARTESIAN_POINT('Ctrl Pts',(3.89390518922201,-6.88632146921344,101.021547619342));
#50997=CARTESIAN_POINT('Ctrl Pts',(4.06494425281458,-6.78960656848446,101.029432552467));
#50998=CARTESIAN_POINT('Ctrl Pts',(4.23241378798273,-6.68649533906992,101.037317485592));
#50999=CARTESIAN_POINT('Ctrl Pts',(4.39581378675215,-6.57728987898509,101.045202418717));
#51000=CARTESIAN_POINT('Ctrl Pts',(4.55921321900226,-6.46808479752328,101.053087324504));
#51001=CARTESIAN_POINT('Ctrl Pts',(4.71854285604712,-6.35278571856391,101.060972230292));
#51002=CARTESIAN_POINT('Ctrl Pts',(4.87333159259317,-6.23173813543487,101.068857136079));
#51003=CARTESIAN_POINT('Ctrl Pts',(5.02814576234542,-6.11067066307997,101.076743337428));
#51004=CARTESIAN_POINT('Ctrl Pts',(5.17841727340561,-5.98385301687583,101.084629538778));
#51005=CARTESIAN_POINT('Ctrl Pts',(5.3237078468869,-5.85167119385521,101.092515740127));
#51006=CARTESIAN_POINT('Ctrl Pts',(5.46904666934658,-5.71944547508988,101.100404560374));
#51007=CARTESIAN_POINT('Ctrl Pts',(5.6094010036736,-5.58185226199119,101.108293380622));
#51008=CARTESIAN_POINT('Ctrl Pts',(5.74436902526336,-5.4393148007442,101.116182200869));
#51009=CARTESIAN_POINT('Ctrl Pts',(5.87946768344214,-5.29663937638916,101.124078656766));
#51010=CARTESIAN_POINT('Ctrl Pts',(6.00916937827817,-5.14901039541447,101.131975112663));
#51011=CARTESIAN_POINT('Ctrl Pts',(6.13311153906114,-4.99688541487946,101.13987156856));
#51012=CARTESIAN_POINT('Ctrl Pts',(6.25712220280107,-4.84467635471466,101.147772388837));
#51013=CARTESIAN_POINT('Ctrl Pts',(6.37536677842443,-4.68796661503222,101.155673209113));
#51014=CARTESIAN_POINT('Ctrl Pts',(6.48752557431558,-4.52724341322635,101.163574029389));
#51015=CARTESIAN_POINT('Ctrl Pts',(6.599820658331,-4.36632491096699,101.171484450232));
#51016=CARTESIAN_POINT('Ctrl Pts',(6.70601500494907,-4.20138349406655,101.179394871075));
#51017=CARTESIAN_POINT('Ctrl Pts',(6.80583392484042,-4.03293262868241,101.187305291918));
#51018=CARTESIAN_POINT('Ctrl Pts',(6.8491513933011,-3.95983160678803,101.190738102108));
#51019=CARTESIAN_POINT('Ctrl Pts',(6.89126883213213,-3.88606996347512,101.194170912298));
#51020=CARTESIAN_POINT('Ctrl Pts',(6.93216659895858,-3.81169086420752,101.197603722488));
#51021=CARTESIAN_POINT('Ctrl Pts',(7.03122517263022,-3.63153707938851,101.205918339825));
#51022=CARTESIAN_POINT('Ctrl Pts',(7.12334236935668,-3.44736477383205,101.214232957163));
#51023=CARTESIAN_POINT('Ctrl Pts',(7.2081979740973,-3.25972436966987,101.2225475745));
#51024=CARTESIAN_POINT('Ctrl Pts',(7.29294870156444,-3.07231587964045,101.230851915388));
#51025=CARTESIAN_POINT('Ctrl Pts',(7.37045561683469,-2.88144810591812,101.239156256275));
#51026=CARTESIAN_POINT('Ctrl Pts',(7.4404442012699,-2.68769624172621,101.247460597162));
#51027=CARTESIAN_POINT('Ctrl Pts',(7.5103509097929,-2.49417103750678,101.255755223244));
#51028=CARTESIAN_POINT('Ctrl Pts',(7.57275673067613,-2.29776874706939,101.264049849326));
#51029=CARTESIAN_POINT('Ctrl Pts',(7.62743476114083,-2.09908550672442,101.272344475407));
#51030=CARTESIAN_POINT('Ctrl Pts',(7.68203046317551,-1.90070142271537,101.280626612313));
#51031=CARTESIAN_POINT('Ctrl Pts',(7.72892151793529,-1.70004352459353,101.288908749219));
#51032=CARTESIAN_POINT('Ctrl Pts',(7.76793043876415,-1.49772417304435,101.297190886125));
#51033=CARTESIAN_POINT('Ctrl Pts',(7.8069033857533,-1.29559139943092,101.305465385283));
#51034=CARTESIAN_POINT('Ctrl Pts',(7.83800863871172,-1.09180051476274,101.313739884442));
#51035=CARTESIAN_POINT('Ctrl Pts',(7.86111906100353,-0.886976949377467,
101.322014383601));
#51036=CARTESIAN_POINT('Ctrl Pts',(7.88420290265242,-0.682388963506358,
101.330279365776));
#51037=CARTESIAN_POINT('Ctrl Pts',(7.89931022953192,-0.476770957721406,
101.338544347952));
#51038=CARTESIAN_POINT('Ctrl Pts',(7.90636527173355,-0.27075669876413,101.346809330127));
#51039=CARTESIAN_POINT('Ctrl Pts',(7.90918505298297,-0.188416277839943,
101.350112703955));
#51040=CARTESIAN_POINT('Ctrl Pts',(7.91071908446983,-0.106012650500569,
101.353416077783));
#51041=CARTESIAN_POINT('Ctrl Pts',(7.91096483829011,-0.0235865923251115,
101.356719451611));
#51042=CARTESIAN_POINT('Ctrl Pts',(7.91157979232759,0.18266955949944,101.364985541109));
#51043=CARTESIAN_POINT('Ctrl Pts',(7.90412375114978,0.388832937379216,101.373251630607));
#51044=CARTESIAN_POINT('Ctrl Pts',(7.88864808877916,0.594266212568875,101.381517720104));
#51045=CARTESIAN_POINT('Ctrl Pts',(7.87315850912396,0.799884234187099,101.389791243308));
#51046=CARTESIAN_POINT('Ctrl Pts',(7.84963493235122,1.00477054946824,101.398064766511));
#51047=CARTESIAN_POINT('Ctrl Pts',(7.81818042396406,1.20829460743029,101.406338289714));
#51048=CARTESIAN_POINT('Ctrl Pts',(7.78669558257738,1.41201493281061,101.414619791449));
#51049=CARTESIAN_POINT('Ctrl Pts',(7.74726458536066,1.61437008822508,101.422901293183));
#51050=CARTESIAN_POINT('Ctrl Pts',(7.7000414184488,1.81474051979148,101.431182794918));
#51051=CARTESIAN_POINT('Ctrl Pts',(7.6527396259826,2.01544456380459,101.439478085174));
#51052=CARTESIAN_POINT('Ctrl Pts',(7.59761979330777,2.21415699101003,101.44777337543));
#51053=CARTESIAN_POINT('Ctrl Pts',(7.53488611335355,2.41027223748517,101.456068665686));
#51054=CARTESIAN_POINT('Ctrl Pts',(7.47209553986051,2.60656534201677,101.46437147899));
#51055=CARTESIAN_POINT('Ctrl Pts',(7.40167743164466,2.80025628697147,101.472674292293));
#51056=CARTESIAN_POINT('Ctrl Pts',(7.32388430308222,2.99075905332841,101.480977105596));
#51057=CARTESIAN_POINT('Ctrl Pts',(7.24597187725304,3.18155395936084,101.489292651424));
#51058=CARTESIAN_POINT('Ctrl Pts',(7.16066194149775,3.36915064474596,101.497608197252));
#51059=CARTESIAN_POINT('Ctrl Pts',(7.06825399608287,3.55298556806223,101.50592374308));
#51060=CARTESIAN_POINT('Ctrl Pts',(7.03153980602914,3.62602420432716,101.509227555631));
#51061=CARTESIAN_POINT('Ctrl Pts',(6.99370567780142,3.69846933964838,101.512531368183));
#51062=CARTESIAN_POINT('Ctrl Pts',(6.95477231411373,3.77028686691572,101.515835180734));
#51063=CARTESIAN_POINT('Ctrl Pts',(6.86156141221415,3.94222619747257,101.523744883839));
#51064=CARTESIAN_POINT('Ctrl Pts',(6.76185245423408,4.11092474515443,101.531654586944));
#51065=CARTESIAN_POINT('Ctrl Pts',(6.65589624332205,4.27585853345635,101.539564290049));
#51066=CARTESIAN_POINT('Ctrl Pts',(6.55004753015076,4.44062498839043,101.547465968374));
#51067=CARTESIAN_POINT('Ctrl Pts',(6.43796437391843,4.60163400460239,101.5553676467));
#51068=CARTESIAN_POINT('Ctrl Pts',(6.31994388496384,4.75838526087455,101.563269325025));
#51069=CARTESIAN_POINT('Ctrl Pts',(6.20202126999436,4.91500652386962,101.571164450516));
#51070=CARTESIAN_POINT('Ctrl Pts',(6.07817133745655,5.06737678737977,101.579059576007));
#51071=CARTESIAN_POINT('Ctrl Pts',(5.94873514026518,5.21502360790191,101.586954701498));
#51072=CARTESIAN_POINT('Ctrl Pts',(5.81938231227119,5.36257532985664,101.594844741778));
#51073=CARTESIAN_POINT('Ctrl Pts',(5.68445061487505,5.50540941223202,101.602734782059));
#51074=CARTESIAN_POINT('Ctrl Pts',(5.54432228911601,5.64308526910691,101.610624822339));
#51075=CARTESIAN_POINT('Ctrl Pts',(5.40425827243544,5.78069794241462,101.618511241644));
#51076=CARTESIAN_POINT('Ctrl Pts',(5.25900262512153,5.9131568664827,101.62639766095));
#51077=CARTESIAN_POINT('Ctrl Pts',(5.1089756570331,6.04005701428747,101.634284080255));
#51078=CARTESIAN_POINT('Ctrl Pts',(4.95898976509124,6.16692241787832,101.642168340323));
#51079=CARTESIAN_POINT('Ctrl Pts',(4.80423541898661,6.28823185636755,101.650052600392));
#51080=CARTESIAN_POINT('Ctrl Pts',(4.64516754150017,6.40361925096998,101.657936860461));
#51081=CARTESIAN_POINT('Ctrl Pts',(4.48608109292573,6.51902011698783,101.665822041012));
#51082=CARTESIAN_POINT('Ctrl Pts',(4.32268038165523,6.62849734967503,101.673707221564));
#51083=CARTESIAN_POINT('Ctrl Pts',(4.15545148456132,6.73172666999018,101.681592402116));
#51084=CARTESIAN_POINT('Ctrl Pts',(3.98820172908867,6.83496886604808,101.689478566182));
#51085=CARTESIAN_POINT('Ctrl Pts',(3.81712312939198,6.93196141514126,101.697364730249));
#51086=CARTESIAN_POINT('Ctrl Pts',(3.64272864653235,7.02242472424822,101.705250894315));
#51087=CARTESIAN_POINT('Ctrl Pts',(3.46828315116926,7.11291449497134,101.71313936518));
#51088=CARTESIAN_POINT('Ctrl Pts',(3.29052014573448,7.19687106100321,101.721027836045));
#51089=CARTESIAN_POINT('Ctrl Pts',(3.10997517984555,7.2740618213447,101.72891630691));
#51090=CARTESIAN_POINT('Ctrl Pts',(2.92934710937687,7.35128811247858,101.736808408827));
#51091=CARTESIAN_POINT('Ctrl Pts',(2.74593484329511,7.42174225660399,101.744700510744));
#51092=CARTESIAN_POINT('Ctrl Pts',(2.5602920231717,7.48524052760387,101.75259261266));
#51093=CARTESIAN_POINT('Ctrl Pts',(2.37443398701087,7.54881241225742,101.760493863904));
#51094=CARTESIAN_POINT('Ctrl Pts',(2.18634055780104,7.60541220488174,101.768395115148));
#51095=CARTESIAN_POINT('Ctrl Pts',(1.99657971976665,7.65490629744196,101.776296366391));
#51096=CARTESIAN_POINT('Ctrl Pts',(1.80669314065104,7.70443318623546,101.784202853235));
#51097=CARTESIAN_POINT('Ctrl Pts',(1.61513728549257,7.7468449141241,101.792109340079));
#51098=CARTESIAN_POINT('Ctrl Pts',(1.42248858888792,7.78205931707563,101.800015826923));
#51099=CARTESIAN_POINT('Ctrl Pts',(1.22957448673385,7.81732223371103,101.807933206265));
#51100=CARTESIAN_POINT('Ctrl Pts',(1.0355648757293,7.84536797080917,101.815850585606));
#51101=CARTESIAN_POINT('Ctrl Pts',(0.841040736337092,7.86616625045654,101.823767964948));
#51102=CARTESIAN_POINT('Ctrl Pts',(0.756697141615612,7.87518416296326,101.827200856293));
#51103=CARTESIAN_POINT('Ctrl Pts',(0.67225681227205,7.88284021999969,101.830633747637));
#51104=CARTESIAN_POINT('Ctrl Pts',(0.587766981559898,7.88913499538371,101.834066638982));
#51105=CARTESIAN_POINT('Ctrl Pts',(0.394769987910758,7.90351391784779,101.841908265642));
#51106=CARTESIAN_POINT('Ctrl Pts',(0.200941043716103,7.91082909852056,101.849749892303));
#51107=CARTESIAN_POINT('Ctrl Pts',(0.00684493132486958,7.91099703873761,
101.857591518963));
#51108=CARTESIAN_POINT('Ctrl Pts',(-0.187022647517414,7.9111647812177,101.865423912699));
#51109=CARTESIAN_POINT('Ctrl Pts',(-0.381156420501285,7.90420203919917,
101.873256306434));
#51110=CARTESIAN_POINT('Ctrl Pts',(-0.574985141527442,7.89007687459525,
101.88108870017));
#51111=CARTESIAN_POINT('Ctrl Pts',(-0.768623376083116,7.8759655915912,101.888913396569));
#51112=CARTESIAN_POINT('Ctrl Pts',(-0.961956807702577,7.85470592869529,
101.896738092967));
#51113=CARTESIAN_POINT('Ctrl Pts',(-1.15441264185323,7.82631793708443,101.904562789365));
#51114=CARTESIAN_POINT('Ctrl Pts',(-1.34671678119287,7.79795232105413,101.912381318293));
#51115=CARTESIAN_POINT('Ctrl Pts',(-1.53814435460433,7.76246961773916,101.92019984722));
#51116=CARTESIAN_POINT('Ctrl Pts',(-1.72812595435393,7.71994181881498,101.928018376147));
#51117=CARTESIAN_POINT('Ctrl Pts',(-1.91799475532786,7.6774392701448,101.935832262938));
#51118=CARTESIAN_POINT('Ctrl Pts',(-2.10641895060174,7.62790003471959,101.943646149728));
#51119=CARTESIAN_POINT('Ctrl Pts',(-2.2928374276349,7.57144751883262,101.951460036519));
#51120=CARTESIAN_POINT('Ctrl Pts',(-2.47918146423998,7.51501754550427,101.959270803077));
#51121=CARTESIAN_POINT('Ctrl Pts',(-2.6635210421948,7.45167989363244,101.967081569635));
#51122=CARTESIAN_POINT('Ctrl Pts',(-2.84530817926851,7.38160838604892,101.974892336192));
#51123=CARTESIAN_POINT('Ctrl Pts',(-3.02708809118582,7.31153966346773,101.98270279231));
#51124=CARTESIAN_POINT('Ctrl Pts',(-3.20631543293658,7.23473773639045,101.990513248428));
#51125=CARTESIAN_POINT('Ctrl Pts',(-3.38245980761755,7.15142549774882,101.998323704546));
#51126=CARTESIAN_POINT('Ctrl Pts',(-3.55860904001995,7.06811096151665,102.006134376061));
#51127=CARTESIAN_POINT('Ctrl Pts',(-3.73167481745588,6.9782859058432,102.013945047576));
#51128=CARTESIAN_POINT('Ctrl Pts',(-3.90114910004849,6.88222033207241,102.021755719091));
#51129=CARTESIAN_POINT('Ctrl Pts',(-4.07065790324607,6.78613519048477,102.029567981579));
#51130=CARTESIAN_POINT('Ctrl Pts',(-4.23657344812533,6.68380717213187,102.037380244068));
#51131=CARTESIAN_POINT('Ctrl Pts',(-4.39841443514638,6.57555103825496,102.045192506556));
#51132=CARTESIAN_POINT('Ctrl Pts',(-4.56031689252224,6.46725378659275,102.053007736294));
#51133=CARTESIAN_POINT('Ctrl Pts',(-4.71814141707677,6.35302412981759,102.060822966032));
#51134=CARTESIAN_POINT('Ctrl Pts',(-4.87143758129479,6.23321882269095,102.06863819577));
#51135=CARTESIAN_POINT('Ctrl Pts',(-5.02490046253155,6.11328322147813,102.076461924949));
#51136=CARTESIAN_POINT('Ctrl Pts',(-5.17382486982215,5.98776007550052,102.084285654129));
#51137=CARTESIAN_POINT('Ctrl Pts',(-5.31779443444756,5.85704561643142,102.092109383308));
#51138=CARTESIAN_POINT('Ctrl Pts',(-5.46185134880608,5.72625184981463,102.099937859329));
#51139=CARTESIAN_POINT('Ctrl Pts',(-5.60094717857692,5.59026073830054,102.10776633535));
#51140=CARTESIAN_POINT('Ctrl Pts',(-5.73470400011519,5.44950374172391,102.11559481137));
#51141=CARTESIAN_POINT('Ctrl Pts',(-5.86864490852806,5.30855302406986,102.123434061568));
#51142=CARTESIAN_POINT('Ctrl Pts',(-5.997231900249,5.16282358326201,102.131273311766));
#51143=CARTESIAN_POINT('Ctrl Pts',(-6.12012802892761,5.0127790605147,102.139112561964));
#51144=CARTESIAN_POINT('Ctrl Pts',(-6.18903135503916,4.9286546312648,102.143507740385));
#51145=CARTESIAN_POINT('Ctrl Pts',(-6.2561465794987,4.84317430749099,102.147902918807));
#51146=CARTESIAN_POINT('Ctrl Pts',(-6.3214204938421,4.75642343994236,102.152298097228));
#51147=CARTESIAN_POINT('Ctrl Pts',(-6.43967391169762,4.5992613225368,102.160260617565));
#51148=CARTESIAN_POINT('Ctrl Pts',(-6.55222125606194,4.43747613818277,102.168223137902));
#51149=CARTESIAN_POINT('Ctrl Pts',(-6.65868367227015,4.27151644649098,102.176185658238));
#51150=CARTESIAN_POINT('Ctrl Pts',(-6.76497769988389,4.10581924855255,102.184135584482));
#51151=CARTESIAN_POINT('Ctrl Pts',(-6.86520580707316,3.93596099116097,102.192085510725));
#51152=CARTESIAN_POINT('Ctrl Pts',(-6.95903009909599,3.76242223572476,102.200035436969));
#51153=CARTESIAN_POINT('Ctrl Pts',(-7.05276659930876,3.58904586127887,102.207977924431));
#51154=CARTESIAN_POINT('Ctrl Pts',(-7.14011106066552,3.41199614529247,102.215920411892));
#51155=CARTESIAN_POINT('Ctrl Pts',(-7.22076887284424,3.23178246250637,102.223862899354));
#51156=CARTESIAN_POINT('Ctrl Pts',(-7.30136417999953,3.05170843464222,102.231799231859));
#51157=CARTESIAN_POINT('Ctrl Pts',(-7.37528302387227,2.86847563305343,102.239735564364));
#51158=CARTESIAN_POINT('Ctrl Pts',(-7.44227658919542,2.68261815581602,102.247671896869));
#51159=CARTESIAN_POINT('Ctrl Pts',(-7.50922900592288,2.49687483542564,102.255603354742));
#51160=CARTESIAN_POINT('Ctrl Pts',(-7.5692645055819,2.30851037000006,102.263534812616));
#51161=CARTESIAN_POINT('Ctrl Pts',(-7.62218218110039,2.1180792709707,102.271466270489));
#51162=CARTESIAN_POINT('Ctrl Pts',(-7.67507592790131,1.9277342825261,102.279394141856));
#51163=CARTESIAN_POINT('Ctrl Pts',(-7.72085817505793,1.73532484938847,102.287322013222));
#51164=CARTESIAN_POINT('Ctrl Pts',(-7.7593776195998,1.54142140780961,102.295249884589));
#51165=CARTESIAN_POINT('Ctrl Pts',(-7.79788659221713,1.34757068096308,102.303175600678));
#51166=CARTESIAN_POINT('Ctrl Pts',(-7.82913663230724,1.15222708782594,102.311101316768));
#51167=CARTESIAN_POINT('Ctrl Pts',(-7.85302730058534,0.955972393043547,
102.319027032857));
#51168=CARTESIAN_POINT('Ctrl Pts',(-7.87691833251812,0.759714710946676,
102.326952869589));
#51169=CARTESIAN_POINT('Ctrl Pts',(-7.89344972305619,0.562546235659305,
102.334878706321));
#51170=CARTESIAN_POINT('Ctrl Pts',(-7.90257271029148,0.365055555438395,
102.342804543052));
#51171=CARTESIAN_POINT('Ctrl Pts',(-7.90827573021412,0.241598922781995,
102.347759192623));
#51172=CARTESIAN_POINT('Ctrl Pts',(-7.91108470261973,0.11801649464083,102.352713842193));
#51173=CARTESIAN_POINT('Ctrl Pts',(-7.91099805494791,-0.00554748685628613,
102.357668491763));
#51174=CARTESIAN_POINT('',(-7.91810557688692,-0.00176888807660425,104.357636950005));
#51175=CARTESIAN_POINT('Ctrl Pts',(-7.90203417854292,-0.00560074141040939,
102.35767088191));
#51176=CARTESIAN_POINT('Ctrl Pts',(-7.90771100978507,-0.942735975233794,
102.395290439766));
#51177=CARTESIAN_POINT('Ctrl Pts',(-7.317879724775,-4.51501751106402,102.538987150367));
#51178=CARTESIAN_POINT('Ctrl Pts',(-2.01450770818587,-9.14056363453498,
102.788761013724));
#51179=CARTESIAN_POINT('Ctrl Pts',(6.61006158010275,-6.62790280679132,103.106992471968));
#51180=CARTESIAN_POINT('Ctrl Pts',(8.71221666557344,0.533409104126239,103.372185353842));
#51181=CARTESIAN_POINT('Ctrl Pts',(6.22559096011058,5.37393958538891,103.584339659338));
#51182=CARTESIAN_POINT('Ctrl Pts',(1.80015232899122,8.54088380044195,103.796493964838));
#51183=CARTESIAN_POINT('Ctrl Pts',(-5.38372996403238,7.53625788284238,104.054236257431));
#51184=CARTESIAN_POINT('Ctrl Pts',(-7.90872346788403,2.44045610435053,104.258939973652));
#51185=CARTESIAN_POINT('Ctrl Pts',(-7.92290895871525,-0.0017445537039696,
104.357566537123));
#51186=CARTESIAN_POINT('',(-7.911,-3.28903571045203E-12,106.357668491763));
#51187=CARTESIAN_POINT('Ctrl Pts',(-7.91099978297005,-0.00180488667992536,
104.357741113999));
#51188=CARTESIAN_POINT('Ctrl Pts',(-7.91047045206602,-2.20286967811119,
104.44630434232));
#51189=CARTESIAN_POINT('Ctrl Pts',(-6.94169981391732,-4.38650802119732,
104.534867570641));
#51190=CARTESIAN_POINT('Ctrl Pts',(-3.6782020148806,-7.34180684107737,104.712018234694));
#51191=CARTESIAN_POINT('Ctrl Pts',(-1.40868175871529,-8.08992666571367,
104.800605670427));
#51192=CARTESIAN_POINT('Ctrl Pts',(2.97309270521425,-7.65454228025191,104.977780541892));
#51193=CARTESIAN_POINT('Ctrl Pts',(5.05102072675703,-6.47444880834138,105.066367977625));
#51194=CARTESIAN_POINT('Ctrl Pts',(7.66951518847893,-2.93425195367629,105.24354284909));
#51195=CARTESIAN_POINT('Ctrl Pts',(8.18956872247068,-0.601881960098685,
105.332130284823));
#51196=CARTESIAN_POINT('Ctrl Pts',(7.32306689761338,3.71537198232442,105.509305156288));
#51197=CARTESIAN_POINT('Ctrl Pts',(5.94329958850222,5.66643518936479,105.597892592021));
#51198=CARTESIAN_POINT('Ctrl Pts',(2.16154501637932,7.92205913232967,105.775067463487));
#51199=CARTESIAN_POINT('Ctrl Pts',(-0.210816529299153,8.20894963712998,
105.863654899219));
#51200=CARTESIAN_POINT('Ctrl Pts',(-4.42123908576287,6.91982244717918,106.040829770685));
#51201=CARTESIAN_POINT('Ctrl Pts',(-6.22631625634048,5.35390358803672,106.129417206417));
#51202=CARTESIAN_POINT('Ctrl Pts',(-7.65317280859501,2.31334857514568,106.264559258688));
#51203=CARTESIAN_POINT('Ctrl Pts',(-7.91100000000048,1.15702837836374,106.311113875226));
#51204=CARTESIAN_POINT('Ctrl Pts',(-7.911,-3.28903571045203E-12,106.357668491763));
#51205=CARTESIAN_POINT('',(-7.91099991715881,-0.000809541038039417,108.357668491763));
#51206=CARTESIAN_POINT('Ctrl Pts',(-7.911,-3.28903571045203E-12,106.357668491763));
#51207=CARTESIAN_POINT('Ctrl Pts',(-7.91099999999908,-2.20167589667009,
106.446255927496));
#51208=CARTESIAN_POINT('Ctrl Pts',(-6.94214576672186,-4.38610418338977,
106.534843363229));
#51209=CARTESIAN_POINT('Ctrl Pts',(-3.6782020148797,-7.34180684107791,106.712018234694));
#51210=CARTESIAN_POINT('Ctrl Pts',(-1.40868175871392,-8.08992666571399,
106.800605670427));
#51211=CARTESIAN_POINT('Ctrl Pts',(2.97309270521612,-7.65454228025126,106.977780541892));
#51212=CARTESIAN_POINT('Ctrl Pts',(5.05102072675892,-6.47444880834001,107.066367977625));
#51213=CARTESIAN_POINT('Ctrl Pts',(7.66951518848005,-2.9342519536736,107.24354284909));
#51214=CARTESIAN_POINT('Ctrl Pts',(8.18956872247099,-0.601881960095431,
107.332130284823));
#51215=CARTESIAN_POINT('Ctrl Pts',(7.32306689761171,3.71537198232789,107.509305156289));
#51216=CARTESIAN_POINT('Ctrl Pts',(5.94329958849938,5.66643518936789,107.597892592021));
#51217=CARTESIAN_POINT('Ctrl Pts',(2.16154501637473,7.92205913233101,107.775067463487));
#51218=CARTESIAN_POINT('Ctrl Pts',(-0.210816529304289,8.20894963712993,
107.86365489922));
#51219=CARTESIAN_POINT('Ctrl Pts',(-4.42123908576773,6.91982244717618,108.040829770685));
#51220=CARTESIAN_POINT('Ctrl Pts',(-6.2263162563445,5.35390358803217,108.129417206418));
#51221=CARTESIAN_POINT('Ctrl Pts',(-7.65317280859598,2.31334857514152,108.264559258688));
#51222=CARTESIAN_POINT('Ctrl Pts',(-7.91100000000052,1.15702837836152,108.311113875226));
#51223=CARTESIAN_POINT('Ctrl Pts',(-7.911,-3.56825680114525E-12,108.357668491763));
#51224=CARTESIAN_POINT('',(-7.91099996833566,-0.000689401199207026,110.357696230784));
#51225=CARTESIAN_POINT('Ctrl Pts',(-7.91099983431761,-0.00161908207251058,
108.357668491763));
#51226=CARTESIAN_POINT('Ctrl Pts',(-7.91095706826763,-0.210578356008037,
108.366032203258));
#51227=CARTESIAN_POINT('Ctrl Pts',(-7.90263095137406,-0.419335154028208,
108.374395914752));
#51228=CARTESIAN_POINT('Ctrl Pts',(-7.88609496611805,-0.627237742301582,
108.382759626247));
#51229=CARTESIAN_POINT('Ctrl Pts',(-7.86953193721219,-0.835480343263119,
108.391137016109));
#51230=CARTESIAN_POINT('Ctrl Pts',(-7.84473223822582,-1.04286566971612,
108.399514405971));
#51231=CARTESIAN_POINT('Ctrl Pts',(-7.81182074813354,-1.24875041502709,
108.407891795833));
#51232=CARTESIAN_POINT('Ctrl Pts',(-7.7788550691014,-1.45497415064365,108.416282979111));
#51233=CARTESIAN_POINT('Ctrl Pts',(-7.73775095957343,-1.65969209823175,
108.424674162389));
#51234=CARTESIAN_POINT('Ctrl Pts',(-7.68868381084718,-1.86227341086545,
108.433065345667));
#51235=CARTESIAN_POINT('Ctrl Pts',(-7.63949205421211,-2.06536918652358,
108.441477838677));
#51236=CARTESIAN_POINT('Ctrl Pts',(-7.58229687058085,-2.26631720498226,
108.449890331688));
#51237=CARTESIAN_POINT('Ctrl Pts',(-7.51732357991094,-2.46450140899026,
108.458302824698));
#51238=CARTESIAN_POINT('Ctrl Pts',(-7.45226006582057,-2.66296081618687,
108.466726999491));
#51239=CARTESIAN_POINT('Ctrl Pts',(-7.37939696543437,-2.85864848567774,
108.475151174285));
#51240=CARTESIAN_POINT('Ctrl Pts',(-7.29900733791689,-3.05096917077759,
108.483575349078));
#51241=CARTESIAN_POINT('Ctrl Pts',(-7.21844862570473,-3.24369436682402,
108.492017242564));
#51242=CARTESIAN_POINT('Ctrl Pts',(-7.13033184281655,-3.43303816640151,
108.500459136049));
#51243=CARTESIAN_POINT('Ctrl Pts',(-7.03497657739299,-3.61842860307233,
108.508901029534));
#51244=CARTESIAN_POINT('Ctrl Pts',(-7.00475651897568,-3.6771826718835,108.511576440411));
#51245=CARTESIAN_POINT('Ctrl Pts',(-6.97380976383304,-3.73553988732904,
108.514251851287));
#51246=CARTESIAN_POINT('Ctrl Pts',(-6.94214738164216,-3.79348266525088,
108.516927262164));
#51247=CARTESIAN_POINT('Ctrl Pts',(-6.84934497044179,-3.96331289060716,
108.524768888825));
#51248=CARTESIAN_POINT('Ctrl Pts',(-6.75016062405178,-4.13000313299525,
108.532610515485));
#51249=CARTESIAN_POINT('Ctrl Pts',(-6.64483114589177,-4.29303389720914,
108.540452142145));
#51250=CARTESIAN_POINT('Ctrl Pts',(-6.53962568525626,-4.4558727049817,108.548284535881));
#51251=CARTESIAN_POINT('Ctrl Pts',(-6.42828968841049,-4.61506032195092,
108.556116929617));
#51252=CARTESIAN_POINT('Ctrl Pts',(-6.31110675512517,-4.77009984438623,
108.563949323353));
#51253=CARTESIAN_POINT('Ctrl Pts',(-6.19403898415056,-4.92498700069487,
108.571774019751));
#51254=CARTESIAN_POINT('Ctrl Pts',(-6.07113592995873,-5.07573390221857,
108.57959871615));
#51255=CARTESIAN_POINT('Ctrl Pts',(-5.9427256775954,-5.2218705959501,108.587423412548));
#51256=CARTESIAN_POINT('Ctrl Pts',(-5.81441663894217,-5.36789210388703,
108.595241941475));
#51257=CARTESIAN_POINT('Ctrl Pts',(-5.68060927852424,-5.50931037850196,
108.603060470402));
#51258=CARTESIAN_POINT('Ctrl Pts',(-5.5416734439547,-5.64568653403351,108.61087899933));
#51259=CARTESIAN_POINT('Ctrl Pts',(-5.40282010049028,-5.78198171823165,
108.61869288612));
#51260=CARTESIAN_POINT('Ctrl Pts',(-5.2588445985855,-5.91324050103304,108.626506772911));
#51261=CARTESIAN_POINT('Ctrl Pts',(-5.11015543976854,-6.03905889865333,
108.634320659702));
#51262=CARTESIAN_POINT('Ctrl Pts',(-4.96152565534921,-6.16482705460416,
108.64213142626));
#51263=CARTESIAN_POINT('Ctrl Pts',(-4.80818623225492,-6.28515892681596,
108.649942192818));
#51264=CARTESIAN_POINT('Ctrl Pts',(-4.65058086069437,-6.39968895010869,
108.657752959375));
#51265=CARTESIAN_POINT('Ctrl Pts',(-4.49298175318107,-6.51421442138982,
108.665563415493));
#51266=CARTESIAN_POINT('Ctrl Pts',(-4.3311173141357,-6.6229382890854,108.673373871611));
#51267=CARTESIAN_POINT('Ctrl Pts',(-4.16546287131606,-6.72553641486591,
108.681184327729));
#51268=CARTESIAN_POINT('Ctrl Pts',(-3.99980386006779,-6.82813737010397,
108.688994999244));
#51269=CARTESIAN_POINT('Ctrl Pts',(-3.83035493565669,-6.92461206088938,
108.696805670759));
#51270=CARTESIAN_POINT('Ctrl Pts',(-3.65761882368748,-7.01468071551422,
108.704616342274));
#51271=CARTESIAN_POINT('Ctrl Pts',(-3.48484752670273,-7.10476771643026,
108.712428604763));
#51272=CARTESIAN_POINT('Ctrl Pts',(-3.30878802036883,-7.18844591910283,
108.720240867251));
#51273=CARTESIAN_POINT('Ctrl Pts',(-3.12996607474961,-7.26548232197399,
108.72805312974));
#51274=CARTESIAN_POINT('Ctrl Pts',(-2.9510762090793,-7.34254798476848,108.735868359478));
#51275=CARTESIAN_POINT('Ctrl Pts',(-2.76942213703738,-7.41296668362044,
108.743683589216));
#51276=CARTESIAN_POINT('Ctrl Pts',(-2.58554810570294,-7.47655415235494,
108.751498818953));
#51277=CARTESIAN_POINT('Ctrl Pts',(-2.40147410243307,-7.54021077554862,
108.759322548133));
#51278=CARTESIAN_POINT('Ctrl Pts',(-2.21517565043103,-7.59702121512676,
108.767146277312));
#51279=CARTESIAN_POINT('Ctrl Pts',(-2.02721162948329,-7.64685124801625,
108.774970006492));
#51280=CARTESIAN_POINT('Ctrl Pts',(-1.83913356632677,-7.69671151396303,
108.782798482513));
#51281=CARTESIAN_POINT('Ctrl Pts',(-1.64938826247017,-7.73958285562081,
108.790626958534));
#51282=CARTESIAN_POINT('Ctrl Pts',(-1.45854328020047,-7.77538246646312,
108.798455434554));
#51283=CARTESIAN_POINT('Ctrl Pts',(-1.267435641748,-7.81123134760332,108.806294684752));
#51284=CARTESIAN_POINT('Ctrl Pts',(-1.0752256487331,-7.83998900646917,108.81413393495));
#51285=CARTESIAN_POINT('Ctrl Pts',(-0.882485612244638,-7.86162452322554,
108.821973185148));
#51286=CARTESIAN_POINT('Ctrl Pts',(-0.774423383347515,-7.873754759406,108.826368363569));
#51287=CARTESIAN_POINT('Ctrl Pts',(-0.666194552038647,-7.88364713922093,
108.83076354199));
#51288=CARTESIAN_POINT('Ctrl Pts',(-0.557899681538563,-7.89130337430637,
108.835158720411));
#51289=CARTESIAN_POINT('Ctrl Pts',(-0.363004324027375,-7.90508209408578,
108.843068604469));
#51290=CARTESIAN_POINT('Ctrl Pts',(-0.167335115482649,-7.9116549857076,
108.850978488527));
#51291=CARTESIAN_POINT('Ctrl Pts',(0.0285325814148896,-7.91094854564216,
108.858888372584));
#51292=CARTESIAN_POINT('Ctrl Pts',(0.224187337279239,-7.91024287359554,
108.866789657272));
#51293=CARTESIAN_POINT('Ctrl Pts',(0.420039809847823,-7.90227363419173,
108.874690941959));
#51294=CARTESIAN_POINT('Ctrl Pts',(0.615509318319252,-7.88701903630657,
108.882592226646));
#51295=CARTESIAN_POINT('Ctrl Pts',(0.810802641600462,-7.87177818805556,
108.890486389561));
#51296=CARTESIAN_POINT('Ctrl Pts',(1.00571334666963,-7.8492650891588,108.898380552476));
#51297=CARTESIAN_POINT('Ctrl Pts',(1.19966026904507,-7.8195099743446,108.906274715391));
#51298=CARTESIAN_POINT('Ctrl Pts',(1.39346840735018,-7.78977615162361,108.91416322942));
#51299=CARTESIAN_POINT('Ctrl Pts',(1.58631379741495,-7.75281068976761,108.922051743449));
#51300=CARTESIAN_POINT('Ctrl Pts',(1.77761963412016,-7.70869570267179,108.929940257478));
#51301=CARTESIAN_POINT('Ctrl Pts',(1.9688241067963,-7.6646040900475,108.937824591752));
#51302=CARTESIAN_POINT('Ctrl Pts',(2.15849031622885,-7.61337057795531,108.945708926025));
#51303=CARTESIAN_POINT('Ctrl Pts',(2.34605062434113,-7.55512855403723,108.953593260299));
#51304=CARTESIAN_POINT('Ctrl Pts',(2.53354638182123,-7.49690657465576,108.961474881106));
#51305=CARTESIAN_POINT('Ctrl Pts',(2.7189373534025,-7.43168099287984,108.969356501912));
#51306=CARTESIAN_POINT('Ctrl Pts',(2.90166979678511,-7.35963541151497,108.977238122718));
#51307=CARTESIAN_POINT('Ctrl Pts',(3.08440463348052,-7.2875888865431,108.985119846753));
#51308=CARTESIAN_POINT('Ctrl Pts',(3.26448054836888,-7.20872230206148,108.993001570788));
#51309=CARTESIAN_POINT('Ctrl Pts',(3.44136202810132,-7.1232680976882,109.000883294823));
#51310=CARTESIAN_POINT('Ctrl Pts',(3.61825416320654,-7.03780874553796,109.008765493654));
#51311=CARTESIAN_POINT('Ctrl Pts',(3.79195116863494,-6.94576113234965,109.016647692486));
#51312=CARTESIAN_POINT('Ctrl Pts',(3.96194044342778,-6.84740453914703,109.024529891317));
#51313=CARTESIAN_POINT('Ctrl Pts',(4.13196856255395,-6.7490254704306,109.032413891314));
#51314=CARTESIAN_POINT('Ctrl Pts',(4.29828696405931,-6.64433472178238,109.04029789131));
#51315=CARTESIAN_POINT('Ctrl Pts',(4.46041023448753,-6.53365606227316,109.048181891307));
#51316=CARTESIAN_POINT('Ctrl Pts',(4.62259783267329,-6.42293348735345,109.05606901954));
#51317=CARTESIAN_POINT('Ctrl Pts',(4.78058669824597,-6.3062184617961,109.063956147774));
#51318=CARTESIAN_POINT('Ctrl Pts',(4.93392263410113,-6.18387648976794,109.071843276008));
#51319=CARTESIAN_POINT('Ctrl Pts',(5.08742216188307,-6.0614039928317,109.079738818906));
#51320=CARTESIAN_POINT('Ctrl Pts',(5.23625857463332,-5.93329277354653,109.087634361805));
#51321=CARTESIAN_POINT('Ctrl Pts',(5.38001201481399,-5.79994756187132,109.095529904703));
#51322=CARTESIAN_POINT('Ctrl Pts',(5.5238529958589,-5.6665211475824,109.103430255714));
#51323=CARTESIAN_POINT('Ctrl Pts',(5.66260458993656,-5.52785462983011,109.111330606724));
#51324=CARTESIAN_POINT('Ctrl Pts',(5.79588554515911,-5.38438777832872,109.119230957735));
#51325=CARTESIAN_POINT('Ctrl Pts',(5.92934003778859,-5.24073412695522,109.127141595335));
#51326=CARTESIAN_POINT('Ctrl Pts',(6.05730943919919,-5.09226791789037,109.135052232934));
#51327=CARTESIAN_POINT('Ctrl Pts',(6.17945362544743,-4.93946089071921,109.142962870534));
#51328=CARTESIAN_POINT('Ctrl Pts',(6.23312123649674,-4.87232066610667,109.146438639909));
#51329=CARTESIAN_POINT('Ctrl Pts',(6.28566483662988,-4.80434279559942,109.149914409283));
#51330=CARTESIAN_POINT('Ctrl Pts',(6.33705831246445,-4.73556891454715,109.153390178658));
#51331=CARTESIAN_POINT('Ctrl Pts',(6.45401528938204,-4.57905906406232,109.161300044101));
#51332=CARTESIAN_POINT('Ctrl Pts',(6.56532854390461,-4.41800259386137,109.169209909545));
#51333=CARTESIAN_POINT('Ctrl Pts',(6.67062519711001,-4.25284381087304,109.177119774988));
#51334=CARTESIAN_POINT('Ctrl Pts',(6.77580741471002,-4.08786452119945,109.18502104405));
#51335=CARTESIAN_POINT('Ctrl Pts',(6.87498587143819,-3.91879208730285,109.192922313111));
#51336=CARTESIAN_POINT('Ctrl Pts',(6.96782831829315,-3.74610324561298,109.200823582173));
#51337=CARTESIAN_POINT('Ctrl Pts',(7.06058711703034,-3.57356999112546,109.20871773244));
#51338=CARTESIAN_POINT('Ctrl Pts',(7.14702111541331,-3.3974271214705,109.216611882707));
#51339=CARTESIAN_POINT('Ctrl Pts',(7.2268415715172,-3.21817990488269,109.224506032975));
#51340=CARTESIAN_POINT('Ctrl Pts',(7.30660493982616,-3.03906088636392,109.232394537325));
#51341=CARTESIAN_POINT('Ctrl Pts',(7.37976404985226,-2.85684225819138,109.240283041676));
#51342=CARTESIAN_POINT('Ctrl Pts',(7.44607616145086,-2.67205366672774,109.248171546027));
#51343=CARTESIAN_POINT('Ctrl Pts',(7.51235316222157,-2.4873629168239,109.256055873585));
#51344=CARTESIAN_POINT('Ctrl Pts',(7.57179027224848,-2.30010523898282,109.263940201144));
#51345=CARTESIAN_POINT('Ctrl Pts',(7.62419284282803,-2.1108302857809,109.271824528702));
#51346=CARTESIAN_POINT('Ctrl Pts',(7.67657739821851,-1.92162040236524,109.279706145751));
#51347=CARTESIAN_POINT('Ctrl Pts',(7.7219321420792,-1.73039495782352,109.2875877628));
#51348=CARTESIAN_POINT('Ctrl Pts',(7.76011218289167,-1.53771906047116,109.29546937985));
#51349=CARTESIAN_POINT('Ctrl Pts',(7.79829274520056,-1.3450405313827,109.303351104553));
#51350=CARTESIAN_POINT('Ctrl Pts',(7.8292983332167,-1.15091184659485,109.311232829256));
#51351=CARTESIAN_POINT('Ctrl Pts',(7.85303499544822,-0.955909179925386,
109.319114553959));
#51352=CARTESIAN_POINT('Ctrl Pts',(7.87677309588481,-0.760894698038554,
109.326996756216));
#51353=CARTESIAN_POINT('Ctrl Pts',(7.89324135062022,-0.565006471327188,
109.334878958473));
#51354=CARTESIAN_POINT('Ctrl Pts',(7.90239760140287,-0.368826719940726,
109.34276116073));
#51355=CARTESIAN_POINT('Ctrl Pts',(7.91155594768836,-0.172602070785931,
109.350645166911));
#51356=CARTESIAN_POINT('Ctrl Pts',(7.91339893936832,0.0239138912713034,
109.358529173092));
#51357=CARTESIAN_POINT('Ctrl Pts',(7.90793654266766,0.220137768548511,109.366413179273));
#51358=CARTESIAN_POINT('Ctrl Pts',(7.90247197666961,0.416439572780986,109.374300316452));
#51359=CARTESIAN_POINT('Ctrl Pts',(7.88969625097962,0.612448716436179,109.382187453631));
#51360=CARTESIAN_POINT('Ctrl Pts',(7.86967131823589,0.807585501934868,109.390074590809));
#51361=CARTESIAN_POINT('Ctrl Pts',(7.84962501071162,1.002930578069,109.397970146784));
#51362=CARTESIAN_POINT('Ctrl Pts',(7.82231407557405,1.19740109275375,109.405865702759));
#51363=CARTESIAN_POINT('Ctrl Pts',(7.78785202926404,1.39042503224301,109.413761258735));
#51364=CARTESIAN_POINT('Ctrl Pts',(7.75336898642348,1.58356657452943,109.421661625198));
#51365=CARTESIAN_POINT('Ctrl Pts',(7.71172621937584,1.77525944825649,109.429561991662));
#51366=CARTESIAN_POINT('Ctrl Pts',(7.66308759286952,1.96494517582788,109.437462358126));
#51367=CARTESIAN_POINT('Ctrl Pts',(7.614385615226,2.15487796643159,109.445373014707));
#51368=CARTESIAN_POINT('Ctrl Pts',(7.55866967518494,2.34279805922108,109.453283671289));
#51369=CARTESIAN_POINT('Ctrl Pts',(7.49615276674389,2.52816429403588,109.46119432787));
#51370=CARTESIAN_POINT('Ctrl Pts',(7.46868420297819,2.60961016792806,109.464670097548));
#51371=CARTESIAN_POINT('Ctrl Pts',(7.4399033076061,2.69056329321023,109.468145867227));
#51372=CARTESIAN_POINT('Ctrl Pts',(7.40983099053721,2.77097919365599,109.471621636905));
#51373=CARTESIAN_POINT('Ctrl Pts',(7.34200954487035,2.9523394330529,109.479460465015));
#51374=CARTESIAN_POINT('Ctrl Pts',(7.26742327569606,3.13148215794732,109.487299293126));
#51375=CARTESIAN_POINT('Ctrl Pts',(7.18623567320809,3.30786001050701,109.495138121236));
#51376=CARTESIAN_POINT('Ctrl Pts',(7.10513908076501,3.48404014622587,109.502968162142));
#51377=CARTESIAN_POINT('Ctrl Pts',(7.01745603542431,3.6574612649623,109.510798203047));
#51378=CARTESIAN_POINT('Ctrl Pts',(6.92339947281602,3.82759202891464,109.518628243953));
#51379=CARTESIAN_POINT('Ctrl Pts',(6.82943004016098,3.99756519104635,109.526451031445));
#51380=CARTESIAN_POINT('Ctrl Pts',(6.7290990170093,4.1642537628276,109.534273818938));
#51381=CARTESIAN_POINT('Ctrl Pts',(6.6226670857949,4.32714705905969,109.54209660643));
#51382=CARTESIAN_POINT('Ctrl Pts',(6.51631304510166,4.48992114441593,109.54991366894));
#51383=CARTESIAN_POINT('Ctrl Pts',(6.40386718056499,4.64890519313521,109.557730731449));
#51384=CARTESIAN_POINT('Ctrl Pts',(6.28563578209234,4.80361362048203,109.565547793959));
#51385=CARTESIAN_POINT('Ctrl Pts',(6.167467919124,4.95823891020145,109.573360655714));
#51386=CARTESIAN_POINT('Ctrl Pts',(6.04352092852737,5.10859287675396,109.58117351747));
#51387=CARTESIAN_POINT('Ctrl Pts',(5.91414414780228,5.25421925684644,109.588986379226));
#51388=CARTESIAN_POINT('Ctrl Pts',(5.78481174060952,5.39979569013358,109.596796561333));
#51389=CARTESIAN_POINT('Ctrl Pts',(5.65005348715701,5.54064750498899,109.60460674344));
#51390=CARTESIAN_POINT('Ctrl Pts',(5.51025881626388,5.67635171371421,109.612416925548));
#51391=CARTESIAN_POINT('Ctrl Pts',(5.37045784054122,5.81206204278647,109.620227459899));
#51392=CARTESIAN_POINT('Ctrl Pts',(5.22562023953531,5.94262405024515,109.628037994251));
#51393=CARTESIAN_POINT('Ctrl Pts',(5.07617245976413,6.06765145329989,109.635848528602));
#51394=CARTESIAN_POINT('Ctrl Pts',(4.92671270161279,6.1926888774186,109.643659688975));
#51395=CARTESIAN_POINT('Ctrl Pts',(4.77264229809379,6.31219058693558,109.651470849348));
#51396=CARTESIAN_POINT('Ctrl Pts',(4.61442087334313,6.42581053281648,109.659282009722));
#51397=CARTESIAN_POINT('Ctrl Pts',(4.45615890108023,6.53945959615827,109.667095171866));
#51398=CARTESIAN_POINT('Ctrl Pts',(4.29374407420746,6.64722368778318,109.674908334011));
#51399=CARTESIAN_POINT('Ctrl Pts',(4.12766520607387,6.74879996344292,109.682721496155));
#51400=CARTESIAN_POINT('Ctrl Pts',(3.96151452444149,6.85042016129356,109.690538036758));
#51401=CARTESIAN_POINT('Ctrl Pts',(3.79169694533208,6.94584702976316,109.698354577361));
#51402=CARTESIAN_POINT('Ctrl Pts',(3.61872621155272,7.03482349500123,109.706171117964));
#51403=CARTESIAN_POINT('Ctrl Pts',(3.44555361777809,7.12390379739405,109.713996780612));
#51404=CARTESIAN_POINT('Ctrl Pts',(3.26922083265525,7.20651850048568,109.721822443259));
#51405=CARTESIAN_POINT('Ctrl Pts',(3.09026293866372,7.28245809942779,109.729648105907));
#51406=CARTESIAN_POINT('Ctrl Pts',(2.91118839417133,7.35844719823859,109.737478869574));
#51407=CARTESIAN_POINT('Ctrl Pts',(2.72948565840863,7.42775239714644,109.74530963324));
#51408=CARTESIAN_POINT('Ctrl Pts',(2.54570539070657,7.49021395313428,109.753140396906));
#51409=CARTESIAN_POINT('Ctrl Pts',(2.36165957983734,7.55276575950434,109.760982475202));
#51410=CARTESIAN_POINT('Ctrl Pts',(2.1755305771564,7.60845407227149,109.768824553498));
#51411=CARTESIAN_POINT('Ctrl Pts',(1.98788082254989,7.65716989724914,109.776666631795));
#51412=CARTESIAN_POINT('Ctrl Pts',(1.88270306568575,7.68447513516794,109.781062119581));
#51413=CARTESIAN_POINT('Ctrl Pts',(1.7770476874526,7.70959082129426,109.785457607366));
#51414=CARTESIAN_POINT('Ctrl Pts',(1.67101438797397,7.7325048926712,109.789853095152));
#51415=CARTESIAN_POINT('Ctrl Pts',(1.48004237283508,7.77377444108104,109.797769619151));
#51416=CARTESIAN_POINT('Ctrl Pts',(1.28727100405664,7.80802330576419,109.805686143149));
#51417=CARTESIAN_POINT('Ctrl Pts',(1.0932588124498,7.83509452202083,109.813602667147));
#51418=CARTESIAN_POINT('Ctrl Pts',(0.899470134704176,7.86213455058755,109.821510070828));
#51419=CARTESIAN_POINT('Ctrl Pts',(0.704443819299248,7.88201335405967,109.829417474509));
#51420=CARTESIAN_POINT('Ctrl Pts',(0.508751275535268,7.89462431909469,109.837324878189));
#51421=CARTESIAN_POINT('Ctrl Pts',(0.313247918679629,7.90722309240568,109.845224637341));
#51422=CARTESIAN_POINT('Ctrl Pts',(0.117079957929666,7.91256800186929,109.853124396493));
#51423=CARTESIAN_POINT('Ctrl Pts',(-0.0791730489321256,7.91060380933863,
109.861024155646));
#51424=CARTESIAN_POINT('Ctrl Pts',(-0.275272680928759,7.90864115185586,
109.868917741009));
#51425=CARTESIAN_POINT('Ctrl Pts',(-0.4714568836888,7.89938077620507,109.876811326373));
#51426=CARTESIAN_POINT('Ctrl Pts',(-0.667142757361975,7.88281939037674,
109.884704911737));
#51427=CARTESIAN_POINT('Ctrl Pts',(-0.862711938983061,7.86626788048917,
109.892593789972));
#51428=CARTESIAN_POINT('Ctrl Pts',(-1.05778304128565,7.84242406465922,109.900482668206));
#51429=CARTESIAN_POINT('Ctrl Pts',(-1.25177466161008,7.81133670997167,109.908371546441));
#51430=CARTESIAN_POINT('Ctrl Pts',(-1.44568651936325,7.78026213731737,109.916257181045));
#51431=CARTESIAN_POINT('Ctrl Pts',(-1.63851943999301,7.74195001584696,109.924142815649));
#51432=CARTESIAN_POINT('Ctrl Pts',(-1.82969834633736,7.69650082579157,109.932028450253));
#51433=CARTESIAN_POINT('Ctrl Pts',(-2.02086024606327,7.65105567873993,109.939913383378));
#51434=CARTESIAN_POINT('Ctrl Pts',(-2.21036808805915,7.59847480139269,109.947798316502));
#51435=CARTESIAN_POINT('Ctrl Pts',(-2.39765766330912,7.53890965124102,109.955683249627));
#51436=CARTESIAN_POINT('Ctrl Pts',(-2.58494658921295,7.47934470760593,109.963568155415));
#51437=CARTESIAN_POINT('Ctrl Pts',(-2.77001693501704,7.41279564334951,109.971453061202));
#51438=CARTESIAN_POINT('Ctrl Pts',(-2.95232021497289,7.33946362810406,109.979337966989));
#51439=CARTESIAN_POINT('Ctrl Pts',(-3.13465344902654,7.26611956373719,109.987224168339));
#51440=CARTESIAN_POINT('Ctrl Pts',(-3.31421839151424,7.18599045632738,109.995110369688));
#51441=CARTESIAN_POINT('Ctrl Pts',(-3.49048685207083,7.09932549863159,110.002996571037));
#51442=CARTESIAN_POINT('Ctrl Pts',(-3.666813848932,7.01263176070851,110.010885391285));
#51443=CARTESIAN_POINT('Ctrl Pts',(-3.8398418735395,6.91939799989301,110.018774211532));
#51444=CARTESIAN_POINT('Ctrl Pts',(-4.00906741953157,6.81991931225366,110.026663031779));
#51445=CARTESIAN_POINT('Ctrl Pts',(-4.17845676023396,6.72034433842579,110.034559487676));
#51446=CARTESIAN_POINT('Ctrl Pts',(-4.3440359736098,6.61451253902403,110.042455943574));
#51447=CARTESIAN_POINT('Ctrl Pts',(-4.5053297424175,6.50276286758853,110.050352399471));
#51448=CARTESIAN_POINT('Ctrl Pts',(-4.66671265845338,6.39095143199729,110.058253219747));
#51449=CARTESIAN_POINT('Ctrl Pts',(-4.82380513221666,6.27321580925561,110.066154040023));
#51450=CARTESIAN_POINT('Ctrl Pts',(-4.97616480907838,6.14993534867562,110.0740548603));
#51451=CARTESIAN_POINT('Ctrl Pts',(-5.12870962357899,6.02650508564224,110.081965281142));
#51452=CARTESIAN_POINT('Ctrl Pts',(-5.27650989459288,5.89751675225094,110.089875701985));
#51453=CARTESIAN_POINT('Ctrl Pts',(-5.41915921673199,5.76338740531198,110.097786122828));
#51454=CARTESIAN_POINT('Ctrl Pts',(-5.48106338800262,5.70518056674579,110.101218933018));
#51455=CARTESIAN_POINT('Ctrl Pts',(-5.54199802297115,5.64600600346155,110.104651743209));
#51456=CARTESIAN_POINT('Ctrl Pts',(-5.60193227078134,5.58589973357727,110.108084553399));
#51457=CARTESIAN_POINT('Ctrl Pts',(-5.74709914815854,5.44031620114478,110.116399170736));
#51458=CARTESIAN_POINT('Ctrl Pts',(-5.88671264835898,5.28894550837697,110.124713788074));
#51459=CARTESIAN_POINT('Ctrl Pts',(-6.02031237203694,5.13222758099239,110.133028405411));
#51460=CARTESIAN_POINT('Ctrl Pts',(-6.15374697315395,4.97570334910959,110.141332746299));
#51461=CARTESIAN_POINT('Ctrl Pts',(-6.28118243254853,4.81384528582643,110.149637087186));
#51462=CARTESIAN_POINT('Ctrl Pts',(-6.40219537707625,4.64712979738499,110.157941428073));
#51463=CARTESIAN_POINT('Ctrl Pts',(-6.52306675501411,4.48060934050211,110.166236054155));
#51464=CARTESIAN_POINT('Ctrl Pts',(-6.63753043204616,4.3092430287315,110.174530680237));
#51465=CARTESIAN_POINT('Ctrl Pts',(-6.7452029677036,4.13354060394749,110.182825306319));
#51466=CARTESIAN_POINT('Ctrl Pts',(-6.85271338137667,3.95810273340278,110.191107443224));
#51467=CARTESIAN_POINT('Ctrl Pts',(-6.95345290714794,3.77834202845535,110.19938958013));
#51468=CARTESIAN_POINT('Ctrl Pts',(-7.04708107639469,3.59479753292447,110.207671717036));
#51469=CARTESIAN_POINT('Ctrl Pts',(-7.1406229021927,3.41142230124729,110.215946216195));
#51470=CARTESIAN_POINT('Ctrl Pts',(-7.22706631643813,3.22427049770358,110.224220715354));
#51471=CARTESIAN_POINT('Ctrl Pts',(-7.30611559512506,3.03390769646514,110.232495214513));
#51472=CARTESIAN_POINT('Ctrl Pts',(-7.38507395463228,2.84376384257224,110.240760196688));
#51473=CARTESIAN_POINT('Ctrl Pts',(-7.45665503644043,2.65041663065321,110.249025178864));
#51474=CARTESIAN_POINT('Ctrl Pts',(-7.52061015159196,2.45445390011138,110.257290161039));
#51475=CARTESIAN_POINT('Ctrl Pts',(-7.54617193128604,2.37613090539093,110.260593534867));
#51476=CARTESIAN_POINT('Ctrl Pts',(-7.57051601546906,2.29739034014392,110.263896908695));
#51477=CARTESIAN_POINT('Ctrl Pts',(-7.59362865868611,2.21827067644617,110.267200282522));
#51478=CARTESIAN_POINT('Ctrl Pts',(-7.64735406795353,2.03435677818093,110.274878985005));
#51479=CARTESIAN_POINT('Ctrl Pts',(-7.69438959007227,1.84850444935335,110.282557687488));
#51480=CARTESIAN_POINT('Ctrl Pts',(-7.7346069444322,1.66125748008586,110.290236389971));
#51481=CARTESIAN_POINT('Ctrl Pts',(-7.77483067255035,1.4739808353977,110.297916309397));
#51482=CARTESIAN_POINT('Ctrl Pts',(-7.80823401252635,1.28530946842787,110.305596228822));
#51483=CARTESIAN_POINT('Ctrl Pts',(-7.83474004329294,1.09579626483312,110.313276148247));
#51484=CARTESIAN_POINT('Ctrl Pts',(-7.86126910490242,0.906118394983401,
110.320962740682));
#51485=CARTESIAN_POINT('Ctrl Pts',(-7.88088884210709,0.715597589647698,
110.328649333118));
#51486=CARTESIAN_POINT('Ctrl Pts',(-7.89357427237069,0.524791583933543,
110.336335925553));
#51487=CARTESIAN_POINT('Ctrl Pts',(-7.90521327432692,0.349725273401021,
110.343388446637));
#51488=CARTESIAN_POINT('Ctrl Pts',(-7.91101540931456,0.174419123218421,
110.350440967722));
#51489=CARTESIAN_POINT('Ctrl Pts',(-7.91099996925002,-0.000697514249990952,
110.357493488806));
#51490=CARTESIAN_POINT('',(-7.91099998544305,0.000479916693955615,112.357717318707));
#51491=CARTESIAN_POINT('Ctrl Pts',(-7.91099996833566,-0.000689401199207026,
110.357696230784));
#51492=CARTESIAN_POINT('Ctrl Pts',(-7.9107977438684,-2.20213188969668,110.446274420177));
#51493=CARTESIAN_POINT('Ctrl Pts',(-6.9419754291647,-4.38625843456785,110.534852609569));
#51494=CARTESIAN_POINT('Ctrl Pts',(-3.67820201488108,-7.34180684107713,
110.712018234694));
#51495=CARTESIAN_POINT('Ctrl Pts',(-1.40868175871581,-8.08992666571357,
110.800605670427));
#51496=CARTESIAN_POINT('Ctrl Pts',(2.97309270521375,-7.6545422802521,110.977780541892));
#51497=CARTESIAN_POINT('Ctrl Pts',(5.05102072675661,-6.47444880834171,111.066367977625));
#51498=CARTESIAN_POINT('Ctrl Pts',(7.66951518847874,-2.93425195367679,111.24354284909));
#51499=CARTESIAN_POINT('Ctrl Pts',(8.18956872247064,-0.601881960099215,
111.332130284823));
#51500=CARTESIAN_POINT('Ctrl Pts',(7.32306689761362,3.71537198232395,111.509305156288));
#51501=CARTESIAN_POINT('Ctrl Pts',(5.94329958850258,5.66643518936441,111.597892592021));
#51502=CARTESIAN_POINT('Ctrl Pts',(2.16154501637983,7.92205913232953,111.775067463487));
#51503=CARTESIAN_POINT('Ctrl Pts',(-0.210816529298622,8.20894963713,111.863654899219));
#51504=CARTESIAN_POINT('Ctrl Pts',(-4.42123908576242,6.91982244717947,112.040829770685));
#51505=CARTESIAN_POINT('Ctrl Pts',(-6.22631625634013,5.35390358803712,112.129417206417));
#51506=CARTESIAN_POINT('Ctrl Pts',(-7.65310523772621,2.31349256505397,112.264552858839));
#51507=CARTESIAN_POINT('Ctrl Pts',(-7.91092910873721,1.15734629425771,112.311101075528));
#51508=CARTESIAN_POINT('Ctrl Pts',(-7.91099998538287,0.000477168944170301,
112.357649292217));
#51509=CARTESIAN_POINT('',(-7.91099861424721,0.00331099508029248,114.357668491763));
#51510=CARTESIAN_POINT('Ctrl Pts',(-7.91099998544305,0.000479916693955615,
112.357717318707));
#51511=CARTESIAN_POINT('Ctrl Pts',(-7.91101205913391,-0.198544141936758,
112.365761839543));
#51512=CARTESIAN_POINT('Ctrl Pts',(-7.90350929980243,-0.397800859065147,
112.373806360379));
#51513=CARTESIAN_POINT('Ctrl Pts',(-7.88846502048386,-0.596691394778329,
112.381850881216));
#51514=CARTESIAN_POINT('Ctrl Pts',(-7.87343761463156,-0.795358857476649,
112.389886379423));
#51515=CARTESIAN_POINT('Ctrl Pts',(-7.85088556931378,-0.993660631931276,
112.39792187763));
#51516=CARTESIAN_POINT('Ctrl Pts',(-7.82083419264467,-1.19099686446272,
112.405957375838));
#51517=CARTESIAN_POINT('Ctrl Pts',(-7.79082085321744,-1.38808332054989,
112.41398270319));
#51518=CARTESIAN_POINT('Ctrl Pts',(-7.75332716275793,-1.58420634900734,
112.422008030543));
#51519=CARTESIAN_POINT('Ctrl Pts',(-7.70843027685618,-1.77877026814792,
112.430033357895));
#51520=CARTESIAN_POINT('Ctrl Pts',(-7.66356643316235,-1.97319099647826,
112.438052778946));
#51521=CARTESIAN_POINT('Ctrl Pts',(-7.61131032372251,-2.16605458308518,
112.446072199997));
#51522=CARTESIAN_POINT('Ctrl Pts',(-7.55179050507049,-2.35677346546655,
112.454091621048));
#51523=CARTESIAN_POINT('Ctrl Pts',(-7.49231445891098,-2.54735208799767,
112.462105144399));
#51524=CARTESIAN_POINT('Ctrl Pts',(-7.42558545338359,-2.73578883877218,
112.47011866775));
#51525=CARTESIAN_POINT('Ctrl Pts',(-7.35178247536766,-2.92150910230946,
112.478132191101));
#51526=CARTESIAN_POINT('Ctrl Pts',(-7.30055048825237,-3.05043097517122,
112.483694957484));
#51527=CARTESIAN_POINT('Ctrl Pts',(-7.24591078874864,-3.17804408040484,
112.489257723867));
#51528=CARTESIAN_POINT('Ctrl Pts',(-7.18793731267412,-3.30416073898761,
112.49482049025));
#51529=CARTESIAN_POINT('Ctrl Pts',(-7.10179061717378,-3.49156598221443,
112.503086579748));
#51530=CARTESIAN_POINT('Ctrl Pts',(-7.00835969554944,-3.67549421227672,
112.511352669245));
#51531=CARTESIAN_POINT('Ctrl Pts',(-6.90795907835648,-3.85538874456938,
112.519618758743));
#51532=CARTESIAN_POINT('Ctrl Pts',(-6.80746817074922,-4.03544505626445,
112.527892281946));
#51533=CARTESIAN_POINT('Ctrl Pts',(-6.69999519769422,-4.21146017185755,
112.53616580515));
#51534=CARTESIAN_POINT('Ctrl Pts',(-6.58589874287142,-4.38290528629637,
112.544439328353));
#51535=CARTESIAN_POINT('Ctrl Pts',(-6.4716922596982,-4.55451573298111,112.552720830088));
#51536=CARTESIAN_POINT('Ctrl Pts',(-6.3508497054498,-4.72154713585784,112.561002331822));
#51537=CARTESIAN_POINT('Ctrl Pts',(-6.22377124380185,-4.88350207380167,
112.569283833557));
#51538=CARTESIAN_POINT('Ctrl Pts',(-6.09648119925438,-5.04572666322629,
112.577579123813));
#51539=CARTESIAN_POINT('Ctrl Pts',(-5.96293467128937,-5.20285765809875,
112.58587441407));
#51540=CARTESIAN_POINT('Ctrl Pts',(-5.82357149775722,-5.3544314367176,112.594169704326));
#51541=CARTESIAN_POINT('Ctrl Pts',(-5.68408193495291,-5.50614267847735,
112.602472517629));
#51542=CARTESIAN_POINT('Ctrl Pts',(-5.53876540024198,-5.65228643257972,
112.610775330933));
#51543=CARTESIAN_POINT('Ctrl Pts',(-5.38809735982587,-5.79243712447857,
112.619078144236));
#51544=CARTESIAN_POINT('Ctrl Pts',(-5.23719826705766,-5.93280274017227,
112.627393690064));
#51545=CARTESIAN_POINT('Ctrl Pts',(-5.08093148405528,-6.0671567279693,112.635709235892));
#51546=CARTESIAN_POINT('Ctrl Pts',(-4.91980566072326,-6.19511366003202,
112.64402478172));
#51547=CARTESIAN_POINT('Ctrl Pts',(-4.8557894760444,-6.24595165995329,112.647328594271));
#51548=CARTESIAN_POINT('Ctrl Pts',(-4.79100660653029,-6.29578035355523,
112.650632406822));
#51549=CARTESIAN_POINT('Ctrl Pts',(-4.7254901745442,-6.34457749659394,112.653936219373));
#51550=CARTESIAN_POINT('Ctrl Pts',(-4.5686363829092,-6.46140340842323,112.661845922478));
#51551=CARTESIAN_POINT('Ctrl Pts',(-4.40724891346103,-6.57255718027244,
112.669755625583));
#51552=CARTESIAN_POINT('Ctrl Pts',(-4.24177559867099,-6.67766881258118,
112.677665328688));
#51553=CARTESIAN_POINT('Ctrl Pts',(-4.07647016462471,-6.78267380401534,
112.685567007013));
#51554=CARTESIAN_POINT('Ctrl Pts',(-3.90708743087371,-6.88164868324912,
112.693468685339));
#51555=CARTESIAN_POINT('Ctrl Pts',(-3.73410730270417,-6.97426438069933,
112.701370363664));
#51556=CARTESIAN_POINT('Ctrl Pts',(-3.56127062635837,-7.06680327227104,
112.709265489155));
#51557=CARTESIAN_POINT('Ctrl Pts',(-3.38484280093639,-7.15299332627278,
112.717160614646));
#51558=CARTESIAN_POINT('Ctrl Pts',(-3.20533188400639,-7.23254924030055,
112.725055740136));
#51559=CARTESIAN_POINT('Ctrl Pts',(-3.02593658914555,-7.31205391276847,
112.732945780417));
#51560=CARTESIAN_POINT('Ctrl Pts',(-2.84346247326496,-7.38493281976084,
112.740835820698));
#51561=CARTESIAN_POINT('Ctrl Pts',(-2.65844157392847,-7.45094687929049,
112.748725860978));
#51562=CARTESIAN_POINT('Ctrl Pts',(-2.47350558621744,-7.51693064299347,
112.756612280283));
#51563=CARTESIAN_POINT('Ctrl Pts',(-2.28602546804307,-7.57605572168821,
112.764498699588));
#51564=CARTESIAN_POINT('Ctrl Pts',(-2.09655285072453,-7.62813130092284,
112.772385118893));
#51565=CARTESIAN_POINT('Ctrl Pts',(-1.9071321094482,-7.68019262229276,112.780269378962));
#51566=CARTESIAN_POINT('Ctrl Pts',(-1.71572028831223,-7.72520819996158,
112.78815363903));
#51567=CARTESIAN_POINT('Ctrl Pts',(-1.52288405188894,-7.76303710956623,
112.796037899099));
#51568=CARTESIAN_POINT('Ctrl Pts',(-1.33002530193706,-7.80087043567606,
112.80392307965));
#51569=CARTESIAN_POINT('Ctrl Pts',(-1.13574214129956,-7.83151534411266,
112.811808260202));
#51570=CARTESIAN_POINT('Ctrl Pts',(-0.940611930730435,-7.85488193391648,
112.819693440754));
#51571=CARTESIAN_POINT('Ctrl Pts',(-0.745457381665204,-7.87825143822367,
112.82757960482));
#51572=CARTESIAN_POINT('Ctrl Pts',(-0.549455914445102,-7.89434077323925,
112.835465768886));
#51573=CARTESIAN_POINT('Ctrl Pts',(-0.353190498390034,-7.90311188531752,
112.843351932953));
#51574=CARTESIAN_POINT('Ctrl Pts',(-0.156867672318178,-7.91188556305255,
112.851240403818));
#51575=CARTESIAN_POINT('Ctrl Pts',(0.0397189121080171,-7.91333673656131,
112.859128874683));
#51576=CARTESIAN_POINT('Ctrl Pts',(0.2359855440319,-7.90747948609467,112.867017345548));
#51577=CARTESIAN_POINT('Ctrl Pts',(0.432342517195068,-7.90161953954433,
112.874909447465));
#51578=CARTESIAN_POINT('Ctrl Pts',(0.628378900205937,-7.8884444756149,112.882801549381));
#51579=CARTESIAN_POINT('Ctrl Pts',(0.823515112172881,-7.86802032661475,
112.890693651298));
#51580=CARTESIAN_POINT('Ctrl Pts',(1.01887754588227,-7.84757249986393,112.898594902541));
#51581=CARTESIAN_POINT('Ctrl Pts',(1.21333738122448,-7.81985883761164,112.906496153785));
#51582=CARTESIAN_POINT('Ctrl Pts',(1.40632309181363,-7.784996876135,112.914397405029));
#51583=CARTESIAN_POINT('Ctrl Pts',(1.59943668037931,-7.750111814103,112.922303891873));
#51584=CARTESIAN_POINT('Ctrl Pts',(1.79107386132513,-7.70806908361338,112.930210378716));
#51585=CARTESIAN_POINT('Ctrl Pts',(1.98067706652023,-7.65903645102704,112.93811686556));
#51586=CARTESIAN_POINT('Ctrl Pts',(2.17054148159449,-7.6099362678525,112.946034244902));
#51587=CARTESIAN_POINT('Ctrl Pts',(2.35836599483712,-7.5538270461825,112.953951624243));
#51588=CARTESIAN_POINT('Ctrl Pts',(2.54361072498379,-7.49092554226428,112.961869003585));
#51589=CARTESIAN_POINT('Ctrl Pts',(2.62393086671046,-7.46365212020509,112.96530189493));
#51590=CARTESIAN_POINT('Ctrl Pts',(2.70376629238775,-7.43510235247908,112.968734786275));
#51591=CARTESIAN_POINT('Ctrl Pts',(2.78307438609223,-7.40529661536102,112.97216767762));
#51592=CARTESIAN_POINT('Ctrl Pts',(2.96423492963485,-7.33721247306506,112.98000930428));
#51593=CARTESIAN_POINT('Ctrl Pts',(3.14318093264782,-7.2623693071675,112.987850930941));
#51594=CARTESIAN_POINT('Ctrl Pts',(3.31936483863494,-7.18092877475011,112.995692557601));
#51595=CARTESIAN_POINT('Ctrl Pts',(3.4953413013473,-7.09958413242352,113.003524951337));
#51596=CARTESIAN_POINT('Ctrl Pts',(3.66856182698873,-7.01165773657921,113.011357345072));
#51597=CARTESIAN_POINT('Ctrl Pts',(3.83849466888646,-6.91736074503349,113.019189738808));
#51598=CARTESIAN_POINT('Ctrl Pts',(4.00826050814803,-6.82315642448646,113.027014435207));
#51599=CARTESIAN_POINT('Ctrl Pts',(4.17474479279578,-6.72259414520845,113.034839131605));
#51600=CARTESIAN_POINT('Ctrl Pts',(4.3374362261068,-6.61593288844864,113.042663828004));
#51601=CARTESIAN_POINT('Ctrl Pts',(4.49999942508129,-6.50935570271345,113.050482356931));
#51602=CARTESIAN_POINT('Ctrl Pts',(4.65877543429084,-6.39668930578726,113.058300885858));
#51603=CARTESIAN_POINT('Ctrl Pts',(4.81327786445093,-6.27823838346289,113.066119414785));
#51604=CARTESIAN_POINT('Ctrl Pts',(4.96768856106883,-6.15985778962894,113.073933301576));
#51605=CARTESIAN_POINT('Ctrl Pts',(5.11783045472054,-6.03569972512417,113.081747188367));
#51606=CARTESIAN_POINT('Ctrl Pts',(5.26324629612979,-5.90611203976661,113.089561075157));
#51607=CARTESIAN_POINT('Ctrl Pts',(5.40860407023905,-5.77657610122649,113.097371841715));
#51608=CARTESIAN_POINT('Ctrl Pts',(5.54923928989609,-5.6416150952412,113.105182608273));
#51609=CARTESIAN_POINT('Ctrl Pts',(5.68472781341491,-5.50161709748933,113.112993374831));
#51610=CARTESIAN_POINT('Ctrl Pts',(5.82021095192375,-5.36162466397712,113.120803830948));
#51611=CARTESIAN_POINT('Ctrl Pts',(5.95054755074093,-5.2165958839276,113.128614287066));
#51612=CARTESIAN_POINT('Ctrl Pts',(6.0753500520282,-5.06695596441502,113.136424743184));
#51613=CARTESIAN_POINT('Ctrl Pts',(6.20015599512677,-4.91731191812324,113.144235414699));
#51614=CARTESIAN_POINT('Ctrl Pts',(6.31942731061589,-4.76305674885004,113.152046086214));
#51615=CARTESIAN_POINT('Ctrl Pts',(6.43281652946883,-4.6046490092289,113.159856757729));
#51616=CARTESIAN_POINT('Ctrl Pts',(6.54622884483228,-4.4462090031713,113.167669020218));
#51617=CARTESIAN_POINT('Ctrl Pts',(6.65375647194648,-4.28361502794457,113.175481282706));
#51618=CARTESIAN_POINT('Ctrl Pts',(6.75509502054357,-4.11735500818516,113.183293545195));
#51619=CARTESIAN_POINT('Ctrl Pts',(6.85647205949167,-3.95103183963779,113.191108774933));
#51620=CARTESIAN_POINT('Ctrl Pts',(6.95165515441584,-3.78104015314079,113.198924004671));
#51621=CARTESIAN_POINT('Ctrl Pts',(7.04038557978585,-3.6078929984055,113.206739234409));
#51622=CARTESIAN_POINT('Ctrl Pts',(7.12921250380062,-3.4345575377345,113.214562963588));
#51623=CARTESIAN_POINT('Ctrl Pts',(7.21157258156766,-3.25806006791309,113.222386692768));
#51624=CARTESIAN_POINT('Ctrl Pts',(7.28725458589867,-3.07893514064504,113.230210421947));
#51625=CARTESIAN_POINT('Ctrl Pts',(7.36298250828826,-2.89970153405514,113.238038897968));
#51626=CARTESIAN_POINT('Ctrl Pts',(7.43202415801405,-2.71783762099379,113.245867373989));
#51627=CARTESIAN_POINT('Ctrl Pts',(7.49421800006026,-2.53389375617306,113.253695850009));
#51628=CARTESIAN_POINT('Ctrl Pts',(7.55649743826388,-2.34969673304131,113.261535100207));
#51629=CARTESIAN_POINT('Ctrl Pts',(7.61191014478525,-2.16341437661997,113.269374350405));
#51630=CARTESIAN_POINT('Ctrl Pts',(7.6603452936068,-1.97560901564964,113.277213600603));
#51631=CARTESIAN_POINT('Ctrl Pts',(7.68750109493618,-1.8703134772816,113.281608779024));
#51632=CARTESIAN_POINT('Ctrl Pts',(7.71246447789895,-1.76453933763496,113.286003957446));
#51633=CARTESIAN_POINT('Ctrl Pts',(7.73522304295573,-1.65838640724249,113.290399135867));
#51634=CARTESIAN_POINT('Ctrl Pts',(7.77618101864123,-1.46734584158682,113.298309019925));
#51635=CARTESIAN_POINT('Ctrl Pts',(7.81011274704514,-1.274529141365,113.306218903983));
#51636=CARTESIAN_POINT('Ctrl Pts',(7.836864811074,-1.08049568853837,113.31412878804));
#51637=CARTESIAN_POINT('Ctrl Pts',(7.86358779112303,-0.886673182613733,
113.322030072728));
#51638=CARTESIAN_POINT('Ctrl Pts',(7.88314660738071,-0.691636897541618,
113.329931357415));
#51639=CARTESIAN_POINT('Ctrl Pts',(7.8954382993942,-0.495958728584598,113.337832642102));
#51640=CARTESIAN_POINT('Ctrl Pts',(7.90771891236974,-0.300456932893186,
113.345726805017));
#51641=CARTESIAN_POINT('Ctrl Pts',(7.91274542803671,-0.104314747953952,
113.353620967932));
#51642=CARTESIAN_POINT('Ctrl Pts',(7.91046633049954,0.0918881604620854,
113.361515130847));
#51643=CARTESIAN_POINT('Ctrl Pts',(7.90818886383349,0.28795067047491,113.369403644876));
#51644=CARTESIAN_POINT('Ctrl Pts',(7.89861620330697,0.484073473865925,113.377292158905));
#51645=CARTESIAN_POINT('Ctrl Pts',(7.88174881111296,0.679673950155128,113.385180672934));
#51646=CARTESIAN_POINT('Ctrl Pts',(7.86489035616241,0.875170786885998,113.393065007208));
#51647=CARTESIAN_POINT('Ctrl Pts',(7.84074490086257,1.07014550511917,113.400949341482));
#51648=CARTESIAN_POINT('Ctrl Pts',(7.80936495986349,1.26401737474461,113.408833675755));
#51649=CARTESIAN_POINT('Ctrl Pts',(7.77799581856399,1.45782252155666,113.416715296562));
#51650=CARTESIAN_POINT('Ctrl Pts',(7.73939720886962,1.65052523609926,113.424596917368));
#51651=CARTESIAN_POINT('Ctrl Pts',(7.69367331250093,1.84155150905725,113.432478538175));
#51652=CARTESIAN_POINT('Ctrl Pts',(7.6479488172701,2.0325802839543,113.44036026221));
#51653=CARTESIAN_POINT('Ctrl Pts',(7.59509892087008,2.22193223594145,113.448241986244));
#51654=CARTESIAN_POINT('Ctrl Pts',(7.53527871465488,2.40904456008376,113.456123710279));
#51655=CARTESIAN_POINT('Ctrl Pts',(7.47545490485943,2.59616815590695,113.464005909111));
#51656=CARTESIAN_POINT('Ctrl Pts',(7.40866005309115,2.78105152607834,113.471888107942));
#51657=CARTESIAN_POINT('Ctrl Pts',(7.33509884102577,2.96314798691905,113.479770306774));
#51658=CARTESIAN_POINT('Ctrl Pts',(7.26152081945135,3.14528605871231,113.48765430677));
#51659=CARTESIAN_POINT('Ctrl Pts',(7.18117348582827,3.3246356322043,113.495538306767));
#51660=CARTESIAN_POINT('Ctrl Pts',(7.09430938119519,3.50067070771959,113.503422306763));
#51661=CARTESIAN_POINT('Ctrl Pts',(7.00741081036265,3.67677563095908,113.511309434997));
#51662=CARTESIAN_POINT('Ctrl Pts',(6.91399046878444,3.84956312649917,113.51919656323));
#51663=CARTESIAN_POINT('Ctrl Pts',(6.81434659574041,4.01853225358726,113.527083691464));
#51664=CARTESIAN_POINT('Ctrl Pts',(6.7145964140664,4.1876816514322,113.534979234363));
#51665=CARTESIAN_POINT('Ctrl Pts',(6.60860961377191,4.35300424647187,113.542874777261));
#51666=CARTESIAN_POINT('Ctrl Pts',(6.49672808557066,4.5140276009521,113.55077032016));
#51667=CARTESIAN_POINT('Ctrl Pts',(6.38477842539586,4.67514901307513,113.55867067117));
#51668=CARTESIAN_POINT('Ctrl Pts',(6.26692708755868,4.83196569004043,113.566571022181));
#51669=CARTESIAN_POINT('Ctrl Pts',(6.14355606739335,4.98403850775597,113.574471373191));
#51670=CARTESIAN_POINT('Ctrl Pts',(6.02002441297259,5.13630933067413,113.582382010791));
#51671=CARTESIAN_POINT('Ctrl Pts',(5.89095894738568,5.28382369785403,113.590292648391));
#51672=CARTESIAN_POINT('Ctrl Pts',(5.75677908451137,5.42617872651947,113.598203285991));
#51673=CARTESIAN_POINT('Ctrl Pts',(5.6978232478711,5.48872656071111,113.601679055365));
#51674=CARTESIAN_POINT('Ctrl Pts',(5.63788049907605,5.55027887715659,113.60515482474));
#51675=CARTESIAN_POINT('Ctrl Pts',(5.57698840264617,5.61080398488043,113.608630594114));
#51676=CARTESIAN_POINT('Ctrl Pts',(5.4384152588507,5.748541966451,113.616540459557));
#51677=CARTESIAN_POINT('Ctrl Pts',(5.29454938429741,5.88132915470733,113.624450325001));
#51678=CARTESIAN_POINT('Ctrl Pts',(5.14577844025169,6.00873407997399,113.632360190444));
#51679=CARTESIAN_POINT('Ctrl Pts',(4.99716917934169,6.1360005425324,113.640261459506));
#51680=CARTESIAN_POINT('Ctrl Pts',(4.84366572664063,6.25789617080285,113.648162728567));
#51681=CARTESIAN_POINT('Ctrl Pts',(4.68569354725228,6.37402517889899,113.656063997629));
#51682=CARTESIAN_POINT('Ctrl Pts',(4.52786369581773,6.49004955841963,113.663958147896));
#51683=CARTESIAN_POINT('Ctrl Pts',(4.36557341432979,6.60031746463485,113.671852298163));
#51684=CARTESIAN_POINT('Ctrl Pts',(4.19928251574874,6.70447219048054,113.679746448431));
#51685=CARTESIAN_POINT('Ctrl Pts',(4.0331105488446,6.80855242459933,113.687634952781));
#51686=CARTESIAN_POINT('Ctrl Pts',(3.8629439565525,6.9065280067639,113.695523457132));
#51687=CARTESIAN_POINT('Ctrl Pts',(3.68927313665149,6.99808436096491,113.703411961483));
#51688=CARTESIAN_POINT('Ctrl Pts',(3.51569427168885,7.08959223805898,113.711296289041));
#51689=CARTESIAN_POINT('Ctrl Pts',(3.33861518067781,7.17468749930346,113.7191806166));
#51690=CARTESIAN_POINT('Ctrl Pts',(3.15855281032658,7.2531003815181,113.727064944158));
#51691=CARTESIAN_POINT('Ctrl Pts',(2.9785523426212,7.3314863066019,113.734946561207));
#51692=CARTESIAN_POINT('Ctrl Pts',(2.79557095552454,7.40319429365219,113.742828178256));
#51693=CARTESIAN_POINT('Ctrl Pts',(2.61014787257316,7.46800167938531,113.750709795306));
#51694=CARTESIAN_POINT('Ctrl Pts',(2.42472225695041,7.53280995031464,113.758591520009));
#51695=CARTESIAN_POINT('Ctrl Pts',(2.23685520163579,7.5907173097183,113.766473244712));
#51696=CARTESIAN_POINT('Ctrl Pts',(2.04710402586936,7.64154998068255,113.774354969415));
#51697=CARTESIAN_POINT('Ctrl Pts',(1.85734135307399,7.69238573159973,113.782237171672));
#51698=CARTESIAN_POINT('Ctrl Pts',(1.6656946656146,7.73614585001636,113.790119373929));
#51699=CARTESIAN_POINT('Ctrl Pts',(1.47273452838523,7.77270699363497,113.798001576186));
#51700=CARTESIAN_POINT('Ctrl Pts',(1.27973023022795,7.80927650465034,113.805885582367));
#51701=CARTESIAN_POINT('Ctrl Pts',(1.08541222237756,7.83864369360576,113.813769588548));
#51702=CARTESIAN_POINT('Ctrl Pts',(0.890359541063216,7.86073666316572,113.821653594729));
#51703=CARTESIAN_POINT('Ctrl Pts',(0.695229397916131,7.88283840657027,113.829540731908));
#51704=CARTESIAN_POINT('Ctrl Pts',(0.499364342549996,7.89766013553226,113.837427869086));
#51705=CARTESIAN_POINT('Ctrl Pts',(0.303347033686154,7.90518194459519,113.845315006265));
#51706=CARTESIAN_POINT('Ctrl Pts',(0.107120494307821,7.91271178250001,113.85321056224));
#51707=CARTESIAN_POINT('Ctrl Pts',(-0.0892582782667623,7.91292612335113,
113.861106118215));
#51708=CARTESIAN_POINT('Ctrl Pts',(-0.28520700646409,7.9058571934651,113.86900167419));
#51709=CARTESIAN_POINT('Ctrl Pts',(-0.481275119430983,7.89878395672505,
113.876902040654));
#51710=CARTESIAN_POINT('Ctrl Pts',(-0.676912322465104,7.88441862783349,
113.884802407118));
#51711=CARTESIAN_POINT('Ctrl Pts',(-0.871542684049729,7.86284518160439,
113.892702773581));
#51712=CARTESIAN_POINT('Ctrl Pts',(-1.06642654898368,7.84124363626049,113.900613430163));
#51713=CARTESIAN_POINT('Ctrl Pts',(-1.26030061279475,7.81241527123588,113.908524086744));
#51714=CARTESIAN_POINT('Ctrl Pts',(-1.45259920484215,7.7764951327762,113.916434743326));
#51715=CARTESIAN_POINT('Ctrl Pts',(-1.53709100505145,7.76071260868223,113.919910513004));
#51716=CARTESIAN_POINT('Ctrl Pts',(-1.62127884796818,7.74356164554976,113.923386282682));
#51717=CARTESIAN_POINT('Ctrl Pts',(-1.70511576575961,7.72505671340723,113.926862052361));
#51718=CARTESIAN_POINT('Ctrl Pts',(-1.89419135151687,7.68332294054891,113.934700880471));
#51719=CARTESIAN_POINT('Ctrl Pts',(-2.08201942337306,7.63458032208507,113.942539708582));
#51720=CARTESIAN_POINT('Ctrl Pts',(-2.26803511231633,7.57891402044516,113.950378536692));
#51721=CARTESIAN_POINT('Ctrl Pts',(-2.45384228055332,7.52331011986722,113.958208577597));
#51722=CARTESIAN_POINT('Ctrl Pts',(-2.6378407778947,7.46079809030432,113.966038618503));
#51723=CARTESIAN_POINT('Ctrl Pts',(-2.8194746672902,7.39151429684803,113.973868659408));
#51724=CARTESIAN_POINT('Ctrl Pts',(-3.00094029886425,7.32229468491749,113.981691446901));
#51725=CARTESIAN_POINT('Ctrl Pts',(-3.18004535845198,7.24631592605009,113.989514234393));
#51726=CARTESIAN_POINT('Ctrl Pts',(-3.35624766588196,7.16376455540394,113.997337021886));
#51727=CARTESIAN_POINT('Ctrl Pts',(-3.5323210224481,7.08127359866901,114.005154084395));
#51728=CARTESIAN_POINT('Ctrl Pts',(-3.70549554087494,6.99221975896303,114.012971146905));
#51729=CARTESIAN_POINT('Ctrl Pts',(-3.87524750166329,6.89683824667887,114.020788209414));
#51730=CARTESIAN_POINT('Ctrl Pts',(-4.04490824068853,6.80150799076711,114.02860107117));
#51731=CARTESIAN_POINT('Ctrl Pts',(-4.21114977999066,6.69985700776171,114.036413932925));
#51732=CARTESIAN_POINT('Ctrl Pts',(-4.37347139883613,6.5921672402604,114.044226794681));
#51733=CARTESIAN_POINT('Ctrl Pts',(-4.53573734475922,6.48451440809837,114.052036976788));
#51734=CARTESIAN_POINT('Ctrl Pts',(-4.69408575621211,6.37082711236166,114.059847158895));
#51735=CARTESIAN_POINT('Ctrl Pts',(-4.84804324068267,6.25143165494682,114.067657341003));
#51736=CARTESIAN_POINT('Ctrl Pts',(-5.00200766873462,6.13203081272019,114.075467875354));
#51737=CARTESIAN_POINT('Ctrl Pts',(-5.15158049051273,6.00692150274678,114.083278409706));
#51738=CARTESIAN_POINT('Ctrl Pts',(-5.29631946797021,5.87647182356895,114.091088944057));
#51739=CARTESIAN_POINT('Ctrl Pts',(-5.44107004639379,5.7460116887258,114.09890010443));
#51740=CARTESIAN_POINT('Ctrl Pts',(-5.58098574665272,5.61021056708316,114.106711264803));
#51741=CARTESIAN_POINT('Ctrl Pts',(-5.71565951738365,5.46947504623083,114.114522425177));
#51742=CARTESIAN_POINT('Ctrl Pts',(-5.85036780105318,5.32870345899106,114.122335587321));
#51743=CARTESIAN_POINT('Ctrl Pts',(-5.97983123573259,5.18299520763568,114.130148749466));
#51744=CARTESIAN_POINT('Ctrl Pts',(-6.10368145743595,5.03279183616336,114.13796191161));
#51745=CARTESIAN_POINT('Ctrl Pts',(-6.22758523271817,4.88252351585212,114.145778452213));
#51746=CARTESIAN_POINT('Ctrl Pts',(-6.34587073633552,4.72775647467498,114.153594992816));
#51747=CARTESIAN_POINT('Ctrl Pts',(-6.45821142898739,4.56896335490849,114.161411533419));
#51748=CARTESIAN_POINT('Ctrl Pts',(-6.57068322527232,4.40998492068102,114.169237196066));
#51749=CARTESIAN_POINT('Ctrl Pts',(-6.67719615072514,4.24697131085798,114.177062858714));
#51750=CARTESIAN_POINT('Ctrl Pts',(-6.77746777470318,4.08042296372079,114.184888521362));
#51751=CARTESIAN_POINT('Ctrl Pts',(-6.8778047589454,3.91376605502315,114.192719285028));
#51752=CARTESIAN_POINT('Ctrl Pts',(-6.97189216478442,3.74357012427854,114.200550048695));
#51753=CARTESIAN_POINT('Ctrl Pts',(-7.05949464910017,3.57035800716483,114.208380812361));
#51754=CARTESIAN_POINT('Ctrl Pts',(-7.14722370979633,3.39689561675125,114.216222890657));
#51755=CARTESIAN_POINT('Ctrl Pts',(-7.2284489874672,3.22040865381887,114.224064968953));
#51756=CARTESIAN_POINT('Ctrl Pts',(-7.30298373583653,3.04143873094743,114.23190704725));
#51757=CARTESIAN_POINT('Ctrl Pts',(-7.3447604898661,2.94112602298145,114.236302535035));
#51758=CARTESIAN_POINT('Ctrl Pts',(-7.38443624370311,2.84003353465224,114.240698022821));
#51759=CARTESIAN_POINT('Ctrl Pts',(-7.42198508013926,2.73825829135789,114.245093510607));
#51760=CARTESIAN_POINT('Ctrl Pts',(-7.50212521020549,2.52104034243423,114.254474759037));
#51761=CARTESIAN_POINT('Ctrl Pts',(-7.57277029602603,2.30018099658234,114.263856007466));
#51762=CARTESIAN_POINT('Ctrl Pts',(-7.63362932991678,2.07644510002896,114.273237255896));
#51763=CARTESIAN_POINT('Ctrl Pts',(-7.69410323020584,1.85412506906133,114.282559137067));
#51764=CARTESIAN_POINT('Ctrl Pts',(-7.74491449709366,1.62896484033121,114.291881018238));
#51765=CARTESIAN_POINT('Ctrl Pts',(-7.78582391605684,1.40173711806362,114.301202899409));
#51766=CARTESIAN_POINT('Ctrl Pts',(-7.82712413812168,1.17233871479164,114.310613831468));
#51767=CARTESIAN_POINT('Ctrl Pts',(-7.8583322206228,0.940833134487127,114.320024763527));
#51768=CARTESIAN_POINT('Ctrl Pts',(-7.87925145285519,0.708037811617052,
114.329435695586));
#51769=CARTESIAN_POINT('Ctrl Pts',(-7.90017068508755,0.475242488747126,
114.338846627645));
#51770=CARTESIAN_POINT('Ctrl Pts',(-7.91080090790091,0.241157474615384,
114.348257559704));
#51771=CARTESIAN_POINT('Ctrl Pts',(-7.91099722849441,0.0066219901636414,
114.357668491763));
#51772=CARTESIAN_POINT('',(-7.91099829967312,-0.00366759908724605,116.357668491763));
#51773=CARTESIAN_POINT('Ctrl Pts',(-7.911,-3.05644398679306E-12,114.357668491763));
#51774=CARTESIAN_POINT('Ctrl Pts',(-7.91099999999915,-2.20167589667,114.446255927496));
#51775=CARTESIAN_POINT('Ctrl Pts',(-6.94214576672185,-4.38610418338986,
114.534843363229));
#51776=CARTESIAN_POINT('Ctrl Pts',(-3.67820201487939,-7.34180684107811,
114.712018234694));
#51777=CARTESIAN_POINT('Ctrl Pts',(-1.40868175871339,-8.08992666571412,
114.800605670427));
#51778=CARTESIAN_POINT('Ctrl Pts',(2.97309270521692,-7.654542280251,114.977780541892));
#51779=CARTESIAN_POINT('Ctrl Pts',(5.05102072675974,-6.47444880833942,115.066367977625));
#51780=CARTESIAN_POINT('Ctrl Pts',(7.66951518848055,-2.9342519536724,115.24354284909));
#51781=CARTESIAN_POINT('Ctrl Pts',(8.18956872247114,-0.601881960093957,
115.332130284823));
#51782=CARTESIAN_POINT('Ctrl Pts',(7.32306689761095,3.71537198232949,115.509305156289));
#51783=CARTESIAN_POINT('Ctrl Pts',(5.94329958849806,5.66643518936933,115.597892592021));
#51784=CARTESIAN_POINT('Ctrl Pts',(2.16154501637258,7.92205913233164,115.775067463487));
#51785=CARTESIAN_POINT('Ctrl Pts',(-0.210816529306704,8.20894963712991,
115.86365489922));
#51786=CARTESIAN_POINT('Ctrl Pts',(-4.42123908577003,6.91982244717475,116.040829770685));
#51787=CARTESIAN_POINT('Ctrl Pts',(-6.22631625634641,5.35390358803001,116.129417206418));
#51788=CARTESIAN_POINT('Ctrl Pts',(-7.65317280859632,2.31334857513979,116.264559258688));
#51789=CARTESIAN_POINT('Ctrl Pts',(-7.91100000000042,1.157028378361,116.311113875226));
#51790=CARTESIAN_POINT('Ctrl Pts',(-7.911,-2.88657986402541E-12,116.357668491763));
#51791=CARTESIAN_POINT('',(-7.91739038802327,-0.00251068180719704,118.357668491763));
#51792=CARTESIAN_POINT('Ctrl Pts',(-7.91099659934624,-0.00733519817160553,
116.357668491763));
#51793=CARTESIAN_POINT('Ctrl Pts',(-7.91079165791022,-0.228364128203642,
116.366524152405));
#51794=CARTESIAN_POINT('Ctrl Pts',(-7.9013198004979,-0.449004782483658,
116.375379813047));
#51795=CARTESIAN_POINT('Ctrl Pts',(-7.88270168216785,-0.668532115868853,
116.384235473689));
#51796=CARTESIAN_POINT('Ctrl Pts',(-7.86395074028927,-0.889625579563492,
116.393154311514));
#51797=CARTESIAN_POINT('Ctrl Pts',(-7.83592265161949,-1.1095896151356,116.402073149339));
#51798=CARTESIAN_POINT('Ctrl Pts',(-7.79879015635228,-1.32770218693152,
116.410991987165));
#51799=CARTESIAN_POINT('Ctrl Pts',(-7.76152078889647,-1.546618732305,116.419943700261));
#51800=CARTESIAN_POINT('Ctrl Pts',(-7.71507987912638,-1.76366999155661,
116.428895413357));
#51801=CARTESIAN_POINT('Ctrl Pts',(-7.65969030410487,-1.9781469725988,116.437847126454));
#51802=CARTESIAN_POINT('Ctrl Pts',(-7.60404426163348,-2.19361703517964,
116.446840288199));
#51803=CARTESIAN_POINT('Ctrl Pts',(-7.53936658935755,-2.40648877887871,
116.455833449944));
#51804=CARTESIAN_POINT('Ctrl Pts',(-7.46593033294524,-2.6160667544251,116.464826611689));
#51805=CARTESIAN_POINT('Ctrl Pts',(-7.44446218479463,-2.67733418890422,
116.467455647238));
#51806=CARTESIAN_POINT('Ctrl Pts',(-7.42224581913866,-2.73832029444676,
116.470084682787));
#51807=CARTESIAN_POINT('Ctrl Pts',(-7.39928879407273,-2.79900809965062,
116.472713718336));
#51808=CARTESIAN_POINT('Ctrl Pts',(-7.33016084335,-2.98175057588845,116.480630242334));
#51809=CARTESIAN_POINT('Ctrl Pts',(-7.25416142372823,-3.16218858067247,
116.488546766333));
#51810=CARTESIAN_POINT('Ctrl Pts',(-7.17146226843079,-3.33976794590186,
116.496463290331));
#51811=CARTESIAN_POINT('Ctrl Pts',(-7.08885838759699,-3.51714272888714,
116.504370694012));
#51812=CARTESIAN_POINT('Ctrl Pts',(-6.99957028891942,-3.69166512275979,
116.512278097693));
#51813=CARTESIAN_POINT('Ctrl Pts',(-6.90381897258189,-3.86279750877758,
116.520185501374));
#51814=CARTESIAN_POINT('Ctrl Pts',(-6.80816022438812,-4.03376445156269,
116.528085260526));
#51815=CARTESIAN_POINT('Ctrl Pts',(-6.70605087262423,-4.20134761648342,
116.535985019678));
#51816=CARTESIAN_POINT('Ctrl Pts',(-6.59775947367232,-4.36503046124162,
116.54388477883));
#51817=CARTESIAN_POINT('Ctrl Pts',(-6.48955270618156,-4.52858538523739,
116.551778364194));
#51818=CARTESIAN_POINT('Ctrl Pts',(-6.37517370628077,-4.68824577591688,
116.559671949558));
#51819=CARTESIAN_POINT('Ctrl Pts',(-6.25493645407182,-4.84352051255318,
116.567565534922));
#51820=CARTESIAN_POINT('Ctrl Pts',(-6.13477090214157,-4.99870265524137,
116.575454413156));
#51821=CARTESIAN_POINT('Ctrl Pts',(-6.00875426919875,-5.1495040833816,116.583343291391));
#51822=CARTESIAN_POINT('Ctrl Pts',(-5.87724342427105,-5.2954632216514,116.591232169626));
#51823=CARTESIAN_POINT('Ctrl Pts',(-5.74578665200444,-5.44136234662708,
116.59911780423));
#51824=CARTESIAN_POINT('Ctrl Pts',(-5.60884040019354,-5.58242289407251,
116.607003438833));
#51825=CARTESIAN_POINT('Ctrl Pts',(-5.46680151270793,-5.7182166993438,116.614889073437));
#51826=CARTESIAN_POINT('Ctrl Pts',(-5.32477526051347,-5.85399842486498,
116.622774006562));
#51827=CARTESIAN_POINT('Ctrl Pts',(-5.17765751971691,-5.98451409895819,
116.630658939687));
#51828=CARTESIAN_POINT('Ctrl Pts',(-5.02588202282583,-6.10937238123821,
116.638543872812));
#51829=CARTESIAN_POINT('Ctrl Pts',(-4.87410705215107,-6.23423023062577,
116.646428778599));
#51830=CARTESIAN_POINT('Ctrl Pts',(-4.71767462341049,-6.35343050784156,
116.654313684386));
#51831=CARTESIAN_POINT('Ctrl Pts',(-4.55705165747088,-6.46662208507208,
116.662198590174));
#51832=CARTESIAN_POINT('Ctrl Pts',(-4.39640229970778,-6.57983226071478,
116.670084791523));
#51833=CARTESIAN_POINT('Ctrl Pts',(-4.23156131455783,-6.68703157060123,
116.677970992873));
#51834=CARTESIAN_POINT('Ctrl Pts',(-4.06302490889848,-6.78791201988288,
116.685857194222));
#51835=CARTESIAN_POINT('Ctrl Pts',(-3.89443253464182,-6.8888259701593,116.693746014469));
#51836=CARTESIAN_POINT('Ctrl Pts',(-3.72214259028624,-6.98341670189376,
116.701634834717));
#51837=CARTESIAN_POINT('Ctrl Pts',(-3.54667640443721,-7.07142188546323,
116.709523654964));
#51838=CARTESIAN_POINT('Ctrl Pts',(-3.37104038351512,-7.15951224992786,
116.717420110861));
#51839=CARTESIAN_POINT('Ctrl Pts',(-3.19222228861093,-7.24100417960231,
116.725316566758));
#51840=CARTESIAN_POINT('Ctrl Pts',(-3.01076494796376,-7.31568284086405,
116.733213022655));
#51841=CARTESIAN_POINT('Ctrl Pts',(-2.82920731566157,-7.39040277709713,
116.741113842932));
#51842=CARTESIAN_POINT('Ctrl Pts',(-2.64500785192931,-7.45830181786224,
116.749014663208));
#51843=CARTESIAN_POINT('Ctrl Pts',(-2.45872538473524,-7.51921475171833,
116.756915483484));
#51844=CARTESIAN_POINT('Ctrl Pts',(-2.27221655911886,-7.58020170303733,
116.764825904327));
#51845=CARTESIAN_POINT('Ctrl Pts',(-2.08362000463707,-7.63418549598408,
116.77273632517));
#51846=CARTESIAN_POINT('Ctrl Pts',(-1.89350666932651,-7.68105158772001,
116.780646746013));
#51847=CARTESIAN_POINT('Ctrl Pts',(-1.81100499114681,-7.70138962035523,
116.784079556203));
#51848=CARTESIAN_POINT('Ctrl Pts',(-1.72821776810303,-7.72038789334774,
116.787512366392));
#51849=CARTESIAN_POINT('Ctrl Pts',(-1.6451920007676,-7.7380400800597,116.790945176582));
#51850=CARTESIAN_POINT('Ctrl Pts',(-1.44409510160924,-7.78079548148584,
116.799259793919));
#51851=CARTESIAN_POINT('Ctrl Pts',(-1.24115767201284,-7.8157442401945,116.807574411257));
#51852=CARTESIAN_POINT('Ctrl Pts',(-1.03699919790736,-7.84273891338603,
116.815889028594));
#51853=CARTESIAN_POINT('Ctrl Pts',(-0.833093053441164,-7.86970022251477,
116.824193369481));
#51854=CARTESIAN_POINT('Ctrl Pts',(-0.627969163730191,-7.88872701493928,
116.832497710369));
#51855=CARTESIAN_POINT('Ctrl Pts',(-0.422257519540355,-7.89972275381811,
116.840802051256));
#51856=CARTESIAN_POINT('Ctrl Pts',(-0.216786526432214,-7.91070562936845,
116.849096677337));
#51857=CARTESIAN_POINT('Ctrl Pts',(-0.0107294420360976,-7.91367617457794,
116.857391303419));
#51858=CARTESIAN_POINT('Ctrl Pts',(0.195277457471319,-7.9085894895742,116.865685929501));
#51859=CARTESIAN_POINT('Ctrl Pts',(0.400974173447822,-7.90351046356596,
116.873968066407));
#51860=CARTESIAN_POINT('Ctrl Pts',(0.606620563022363,-7.89039842520223,
116.882250203312));
#51861=CARTESIAN_POINT('Ctrl Pts',(0.811579102264985,-7.86926047102056,
116.890532340218));
#51862=CARTESIAN_POINT('Ctrl Pts',(1.01634862972473,-7.84814201015896,116.898806839377));
#51863=CARTESIAN_POINT('Ctrl Pts',(1.22043128110172,-7.81901242310457,116.907081338536));
#51864=CARTESIAN_POINT('Ctrl Pts',(1.42319157471596,-7.7819307849439,116.915355837695));
#51865=CARTESIAN_POINT('Ctrl Pts',(1.6257186619076,-7.74489179653493,116.92362081987));
#51866=CARTESIAN_POINT('Ctrl Pts',(1.82692613844127,-7.69991906017166,116.931885802045));
#51867=CARTESIAN_POINT('Ctrl Pts',(2.02618538996855,-7.64712323462085,116.940150784221));
#51868=CARTESIAN_POINT('Ctrl Pts',(2.10582594847745,-7.62602163456174,116.943454158049));
#51869=CARTESIAN_POINT('Ctrl Pts',(2.18515536128749,-7.60367090045974,116.946757531877));
#51870=CARTESIAN_POINT('Ctrl Pts',(2.26413386273611,-7.58008039875645,116.950060905705));
#51871=CARTESIAN_POINT('Ctrl Pts',(2.46176313369386,-7.52104947809277,116.958326995203));
#51872=CARTESIAN_POINT('Ctrl Pts',(2.65697061966016,-7.45431891274739,116.966593084701));
#51873=CARTESIAN_POINT('Ctrl Pts',(2.84916104808126,-7.38012210753294,116.974859174198));
#51874=CARTESIAN_POINT('Ctrl Pts',(3.04152431362093,-7.30585857702876,116.983132697402));
#51875=CARTESIAN_POINT('Ctrl Pts',(3.23086483097424,-7.22411550795258,116.991406220605));
#51876=CARTESIAN_POINT('Ctrl Pts',(3.41660875776642,-7.13517383084349,116.999679743808));
#51877=CARTESIAN_POINT('Ctrl Pts',(3.60253180579428,-7.04614638326868,117.007961245543));
#51878=CARTESIAN_POINT('Ctrl Pts',(3.7848510742948,-6.94990659525351,117.016242747277));
#51879=CARTESIAN_POINT('Ctrl Pts',(3.96301796747552,-6.84678096549512,117.024524249011));
#51880=CARTESIAN_POINT('Ctrl Pts',(4.14148150469202,-6.74348363378661,117.032819539268));
#51881=CARTESIAN_POINT('Ctrl Pts',(4.31577858984202,-6.6332776866314,117.041114829524));
#51882=CARTESIAN_POINT('Ctrl Pts',(4.48538853247721,-6.51653364241465,117.04941011978));
#51883=CARTESIAN_POINT('Ctrl Pts',(4.65515229535517,-6.39968372234567,117.057712933083));
#51884=CARTESIAN_POINT('Ctrl Pts',(4.82022019296743,-6.2762840412262,117.066015746387));
#51885=CARTESIAN_POINT('Ctrl Pts',(4.98010421305185,-6.14674572657298,117.07431855969));
#51886=CARTESIAN_POINT('Ctrl Pts',(5.14023341837178,-6.01700876241016,117.082634105518));
#51887=CARTESIAN_POINT('Ctrl Pts',(5.29516263203528,-5.88111453788343,117.090949651346));
#51888=CARTESIAN_POINT('Ctrl Pts',(5.44443894142245,-5.73951266338204,117.099265197174));
#51889=CARTESIAN_POINT('Ctrl Pts',(5.5037472483953,-5.683253452022,117.102569009725));
#51890=CARTESIAN_POINT('Ctrl Pts',(5.56216366462417,-5.62609366540991,117.105872822277));
#51891=CARTESIAN_POINT('Ctrl Pts',(5.61966152320723,-5.5680629813773,117.109176634828));
#51892=CARTESIAN_POINT('Ctrl Pts',(5.75731793786419,-5.42913092197752,117.117086337933));
#51893=CARTESIAN_POINT('Ctrl Pts',(5.88999360825696,-5.28491496316134,117.124996041038));
#51894=CARTESIAN_POINT('Ctrl Pts',(6.01725942153507,-5.13580666049136,117.132905744143));
#51895=CARTESIAN_POINT('Ctrl Pts',(6.14439611744201,-4.98684963546276,117.140807422468));
#51896=CARTESIAN_POINT('Ctrl Pts',(6.26613366716165,-4.83301041354343,117.148709100794));
#51897=CARTESIAN_POINT('Ctrl Pts',(6.38207898871818,-4.6747180430227,117.156610779119));
#51898=CARTESIAN_POINT('Ctrl Pts',(6.49792815721914,-4.5165569438193,117.16450590461));
#51899=CARTESIAN_POINT('Ctrl Pts',(6.60799446436491,-4.35395032949121,117.172401030101));
#51900=CARTESIAN_POINT('Ctrl Pts',(6.71192421772876,-4.18736125686167,117.180296155592));
#51901=CARTESIAN_POINT('Ctrl Pts',(6.81578703046658,-4.02087948340731,117.188186195872));
#51902=CARTESIAN_POINT('Ctrl Pts',(6.91352098273932,-3.85042065370394,117.196076236153));
#51903=CARTESIAN_POINT('Ctrl Pts',(7.00481478545324,-3.6764780458335,117.203966276433));
#51904=CARTESIAN_POINT('Ctrl Pts',(7.09606669071054,-3.50261526542835,117.211852695739));
#51905=CARTESIAN_POINT('Ctrl Pts',(7.18088417621274,-3.32527219735225,117.219739115044));
#51906=CARTESIAN_POINT('Ctrl Pts',(7.25900099785885,-3.14496828490913,117.227625534349));
#51907=CARTESIAN_POINT('Ctrl Pts',(7.33709643176276,-2.96471373819178,117.235509794417));
#51908=CARTESIAN_POINT('Ctrl Pts',(7.40849472158182,-2.78150027876586,117.243394054486));
#51909=CARTESIAN_POINT('Ctrl Pts',(7.47297691391634,-2.59586922707469,117.251278314554));
#51910=CARTESIAN_POINT('Ctrl Pts',(7.53746663451241,-2.4102165030573,117.259163495106));
#51911=CARTESIAN_POINT('Ctrl Pts',(7.595038524639,-2.22214594611724,117.267048675658));
#51912=CARTESIAN_POINT('Ctrl Pts',(7.64552265158189,-2.03221661841157,117.27493385621));
#51913=CARTESIAN_POINT('Ctrl Pts',(7.69601307538542,-1.84226360091309,117.282820020276));
#51914=CARTESIAN_POINT('Ctrl Pts',(7.73941388514382,-1.65045168374889,117.290706184342));
#51915=CARTESIAN_POINT('Ctrl Pts',(7.77560569765339,-1.45735274886356,117.298592348409));
#51916=CARTESIAN_POINT('Ctrl Pts',(7.81180809670744,-1.26419733019577,117.306480819274));
#51917=CARTESIAN_POINT('Ctrl Pts',(7.84079723278438,-1.06975448237004,117.314369290139));
#51918=CARTESIAN_POINT('Ctrl Pts',(7.86250523807596,-0.874604128293515,
117.322257761004));
#51919=CARTESIAN_POINT('Ctrl Pts',(7.8842232355301,-0.67936394679919,117.330149862921));
#51920=CARTESIAN_POINT('Ctrl Pts',(7.89865338549164,-0.483415952306765,
117.338041964837));
#51921=CARTESIAN_POINT('Ctrl Pts',(7.90577983826125,-0.287343259781535,
117.345934066754));
#51922=CARTESIAN_POINT('Ctrl Pts',(7.91291455273971,-0.0910432598497572,
117.353835317998));
#51923=CARTESIAN_POINT('Ctrl Pts',(7.9127286447279,0.105381382380236,117.361736569241));
#51924=CARTESIAN_POINT('Ctrl Pts',(7.90525838900726,0.301348308490955,117.369637820485));
#51925=CARTESIAN_POINT('Ctrl Pts',(7.89778318327669,0.497445088018359,117.377544307329));
#51926=CARTESIAN_POINT('Ctrl Pts',(7.88301403312867,0.693083204222326,117.385450794173));
#51927=CARTESIAN_POINT('Ctrl Pts',(7.86103890394467,0.887687079250537,117.393357281017));
#51928=CARTESIAN_POINT('Ctrl Pts',(7.83903350037349,1.08255905341074,117.401274660359));
#51929=CARTESIAN_POINT('Ctrl Pts',(7.80980233968711,1.27639360083801,117.4091920397));
#51930=CARTESIAN_POINT('Ctrl Pts',(7.77348437248839,1.46862578987253,117.417109419042));
#51931=CARTESIAN_POINT('Ctrl Pts',(7.75773728877846,1.55197561933596,117.420542310386));
#51932=CARTESIAN_POINT('Ctrl Pts',(7.7406585225722,1.63502440123127,117.423975201731));
#51933=CARTESIAN_POINT('Ctrl Pts',(7.72226227625815,1.7177270844579,117.427408093076));
#51934=CARTESIAN_POINT('Ctrl Pts',(7.68024041157919,1.90664176323575,117.435249719736));
#51935=CARTESIAN_POINT('Ctrl Pts',(7.6312158607668,2.0943110598549,117.443091346397));
#51936=CARTESIAN_POINT('Ctrl Pts',(7.57527194338821,2.28017016551734,117.450932973057));
#51937=CARTESIAN_POINT('Ctrl Pts',(7.5193938957573,2.46581043608624,117.458765366793));
#51938=CARTESIAN_POINT('Ctrl Pts',(7.45661280379767,2.6496444266374,117.466597760528));
#51939=CARTESIAN_POINT('Ctrl Pts',(7.38706321502987,2.83111604445183,117.474430154264));
#51940=CARTESIAN_POINT('Ctrl Pts',(7.31758197658512,3.01240931982136,117.482254850663));
#51941=CARTESIAN_POINT('Ctrl Pts',(7.24134561259178,3.1913445199734,117.490079547061));
#51942=CARTESIAN_POINT('Ctrl Pts',(7.15853888810705,3.36737909767508,117.49790424346));
#51943=CARTESIAN_POINT('Ctrl Pts',(7.07579743236562,3.54327492389571,117.505722772387));
#51944=CARTESIAN_POINT('Ctrl Pts',(6.9864960795171,3.71627436457766,117.513541301314));
#51945=CARTESIAN_POINT('Ctrl Pts',(6.89086833891235,3.88585312843593,117.521359830241));
#51946=CARTESIAN_POINT('Ctrl Pts',(6.79529737586998,4.05533120740108,117.529173717032));
#51947=CARTESIAN_POINT('Ctrl Pts',(6.69340767955163,4.22139234974059,117.536987603822));
#51948=CARTESIAN_POINT('Ctrl Pts',(6.58547958136801,4.38353506697334,117.544801490613));
#51949=CARTESIAN_POINT('Ctrl Pts',(6.47759458091849,4.54561303754762,117.552612257171));
#51950=CARTESIAN_POINT('Ctrl Pts',(6.3636761772956,4.70377540810573,117.560423023729));
#51951=CARTESIAN_POINT('Ctrl Pts',(6.24404917087586,4.85754783318543,117.568233790286));
#51952=CARTESIAN_POINT('Ctrl Pts',(6.12442691904792,5.01131414655898,117.576044246404));
#51953=CARTESIAN_POINT('Ctrl Pts',(5.99909672521037,5.16069057892542,117.583854702522));
#51954=CARTESIAN_POINT('Ctrl Pts',(5.86842528199299,5.30523380348741,117.59166515864));
#51955=CARTESIAN_POINT('Ctrl Pts',(5.73775023511026,5.44978101427163,117.599475830154));
#51956=CARTESIAN_POINT('Ctrl Pts',(5.60173388087419,5.58949449009391,117.607286501669));
#51957=CARTESIAN_POINT('Ctrl Pts',(5.46078154693117,5.72396592378885,117.615097173184));
#51958=CARTESIAN_POINT('Ctrl Pts',(5.31980050208339,5.8584647482791,117.622909435673));
#51959=CARTESIAN_POINT('Ctrl Pts',(5.17388172929063,5.98771916065832,117.630721698162));
#51960=CARTESIAN_POINT('Ctrl Pts',(5.02346567593081,6.11135939073665,117.63853396065));
#51961=CARTESIAN_POINT('Ctrl Pts',(4.87299249162997,6.23504658177781,117.646349190388));
#51962=CARTESIAN_POINT('Ctrl Pts',(4.71801889584076,6.35311511969274,117.654164420126));
#51963=CARTESIAN_POINT('Ctrl Pts',(4.55901661309642,6.46523692694327,117.661979649864));
#51964=CARTESIAN_POINT('Ctrl Pts',(4.39984140765079,6.57748067210216,117.669803379043));
#51965=CARTESIAN_POINT('Ctrl Pts',(4.23662905198565,6.68376456656124,117.677627108223));
#51966=CARTESIAN_POINT('Ctrl Pts',(4.06987921745359,6.78380454872775,117.685450837402));
#51967=CARTESIAN_POINT('Ctrl Pts',(3.90302821186046,6.88390522751309,117.693279313423));
#51968=CARTESIAN_POINT('Ctrl Pts',(3.73263575734608,6.97775427500677,117.701107789443));
#51969=CARTESIAN_POINT('Ctrl Pts',(3.55922413682134,7.06511461647073,117.708936265464));
#51970=CARTESIAN_POINT('Ctrl Pts',(3.38557385330543,7.15259519024866,117.716775515662));
#51971=CARTESIAN_POINT('Ctrl Pts',(3.2088964231017,7.23356907501793,117.72461476586));
#51972=CARTESIAN_POINT('Ctrl Pts',(3.02973309200395,7.30784772632929,117.732454016057));
#51973=CARTESIAN_POINT('Ctrl Pts',(2.92928282100942,7.34949302622195,117.736849194479));
#51974=CARTESIAN_POINT('Ctrl Pts',(2.82805139765376,7.3890346249793,117.7412443729));
#51975=CARTESIAN_POINT('Ctrl Pts',(2.72613590948133,7.42644625665845,117.745639551322));
#51976=CARTESIAN_POINT('Ctrl Pts',(2.54272135429595,7.49377496111977,117.75354943538));
#51977=CARTESIAN_POINT('Ctrl Pts',(2.3565634426319,7.55439570016004,117.761459319437));
#51978=CARTESIAN_POINT('Ctrl Pts',(2.16819453330328,7.60807817163794,117.769369203495));
#51979=CARTESIAN_POINT('Ctrl Pts',(1.98003041256838,7.66170228126686,117.777270488182));
#51980=CARTESIAN_POINT('Ctrl Pts',(1.78966041073773,7.70840305418294,117.78517177287));
#51981=CARTESIAN_POINT('Ctrl Pts',(1.59763634808956,7.74799839308599,117.793073057557));
#51982=CARTESIAN_POINT('Ctrl Pts',(1.40578536510107,7.78755804298378,117.800967220472));
#51983=CARTESIAN_POINT('Ctrl Pts',(1.2122836269496,7.82002494774707,117.808861383387));
#51984=CARTESIAN_POINT('Ctrl Pts',(1.01769785785694,7.84526685780117,117.816755546302));
#51985=CARTESIAN_POINT('Ctrl Pts',(0.823251329979141,7.87049070531021,117.824644060331));
#51986=CARTESIAN_POINT('Ctrl Pts',(0.627722657320462,7.88849981433292,117.83253257436));
#51987=CARTESIAN_POINT('Ctrl Pts',(0.431688774556004,7.89921298623618,117.840421088389));
#51988=CARTESIAN_POINT('Ctrl Pts',(0.235758760990982,7.90992048172997,117.848305422662));
#51989=CARTESIAN_POINT('Ctrl Pts',(0.039324414345863,7.91333972434937,117.856189756936));
#51990=CARTESIAN_POINT('Ctrl Pts',(-0.157031907085009,7.90944131909184,
117.86407409121));
#51991=CARTESIAN_POINT('Ctrl Pts',(-0.3533206506534,7.9055442555069,117.871955712016));
#51992=CARTESIAN_POINT('Ctrl Pts',(-0.549531078044028,7.89433457017896,
117.879837332823));
#51993=CARTESIAN_POINT('Ctrl Pts',(-0.745080244104152,7.875834967154,117.887718953629));
#51994=CARTESIAN_POINT('Ctrl Pts',(-0.940631971342325,7.85733512183306,
117.895600677664));
#51995=CARTESIAN_POINT('Ctrl Pts',(-1.13552207573532,7.83154519200619,117.903482401699));
#51996=CARTESIAN_POINT('Ctrl Pts',(-1.32917157076089,7.79853985919679,117.911364125734));
#51997=CARTESIAN_POINT('Ctrl Pts',(-1.52283273126742,7.7655325381401,117.919246324565));
#51998=CARTESIAN_POINT('Ctrl Pts',(-1.71525279311446,7.7253090053851,117.927128523397));
#51999=CARTESIAN_POINT('Ctrl Pts',(-1.90586178166159,7.67799530275981,117.935010722228));
#52000=CARTESIAN_POINT('Ctrl Pts',(-2.09651432636319,7.63067078845688,117.942894722225));
#52001=CARTESIAN_POINT('Ctrl Pts',(-2.2853546381759,7.5762529589668,117.950778722221));
#52002=CARTESIAN_POINT('Ctrl Pts',(-2.47182651465308,7.51491814203308,117.958662722218));
#52003=CARTESIAN_POINT('Ctrl Pts',(-2.65837238000031,7.45355898848688,117.966549850451));
#52004=CARTESIAN_POINT('Ctrl Pts',(-2.84254760993641,7.38527748649901,117.974436978685));
#52005=CARTESIAN_POINT('Ctrl Pts',(-3.02381440883524,7.31029872309746,117.982324106919));
#52006=CARTESIAN_POINT('Ctrl Pts',(-3.20527459870139,7.23523996592061,117.990219649817));
#52007=CARTESIAN_POINT('Ctrl Pts',(-3.38381984063555,7.15346980724472,117.998115192716));
#52008=CARTESIAN_POINT('Ctrl Pts',(-3.558934442781,7.06526054947637,118.006010735614));
#52009=CARTESIAN_POINT('Ctrl Pts',(-3.73415568365131,6.97699757532655,118.013911086625));
#52010=CARTESIAN_POINT('Ctrl Pts',(-3.90594181839956,6.88228785083727,118.021811437636));
#52011=CARTESIAN_POINT('Ctrl Pts',(-4.07380451921806,6.78144805621915,118.029711788646));
#52012=CARTESIAN_POINT('Ctrl Pts',(-4.24188578433035,6.68047696394891,118.037622426246));
#52013=CARTESIAN_POINT('Ctrl Pts',(-4.40603312355957,6.5733600467252,118.045533063846));
#52014=CARTESIAN_POINT('Ctrl Pts',(-4.56578884836695,6.46045611331955,118.053443701445));
#52015=CARTESIAN_POINT('Ctrl Pts',(-4.63598218597049,6.41084847688671,118.05691947082));
#52016=CARTESIAN_POINT('Ctrl Pts',(-4.7053281509237,6.36012414408697,118.060395240194));
#52017=CARTESIAN_POINT('Ctrl Pts',(-4.77379010025081,6.30831586707161,118.063871009569));
#52018=CARTESIAN_POINT('Ctrl Pts',(-4.92785616684936,6.19172705335163,118.071692845219));
#52019=CARTESIAN_POINT('Ctrl Pts',(-5.07788000157877,6.06931558110785,118.07951468087));
#52020=CARTESIAN_POINT('Ctrl Pts',(-5.22338588974355,5.94139384713958,118.08733651652));
#52021=CARTESIAN_POINT('Ctrl Pts',(-5.3687326525521,5.81361200848237,118.095149798205));
#52022=CARTESIAN_POINT('Ctrl Pts',(-5.50957104373117,5.68033213790914,118.102963079889));
#52023=CARTESIAN_POINT('Ctrl Pts',(-5.64545491891002,5.54190939645847,118.110776361574));
#52024=CARTESIAN_POINT('Ctrl Pts',(-5.78121693991536,5.40361078591541,118.118582636681));
#52025=CARTESIAN_POINT('Ctrl Pts',(-5.91203304661729,5.2601787392757,118.126388911787));
#52026=CARTESIAN_POINT('Ctrl Pts',(-6.03749063183514,5.11200820328987,118.134195186894));
#52027=CARTESIAN_POINT('Ctrl Pts',(-6.16286039290777,4.96394139120919,118.141995997369));
#52028=CARTESIAN_POINT('Ctrl Pts',(-6.282878876065,4.81114296519533,118.149796807844));
#52029=CARTESIAN_POINT('Ctrl Pts',(-6.39717067080784,4.65404430668167,118.15759761832));
#52030=CARTESIAN_POINT('Ctrl Pts',(-6.51140493154762,4.49702473096408,118.1653945019));
#52031=CARTESIAN_POINT('Ctrl Pts',(-6.61991803901518,4.33570952033906,118.173191385481));
#52032=CARTESIAN_POINT('Ctrl Pts',(-6.72237509636622,4.17056279940193,118.180988269061));
#52033=CARTESIAN_POINT('Ctrl Pts',(-6.82481259867789,4.00544759850562,118.188783664522));
#52034=CARTESIAN_POINT('Ctrl Pts',(-6.921196162118,3.83650264120311,118.196579059983));
#52035=CARTESIAN_POINT('Ctrl Pts',(-7.01123424735637,3.6642209715978,118.204374455444));
#52036=CARTESIAN_POINT('Ctrl Pts',(-7.10126646972894,3.49195052018206,118.212169343304));
#52037=CARTESIAN_POINT('Ctrl Pts',(-7.18495387231422,3.31634410237102,118.219964231165));
#52038=CARTESIAN_POINT('Ctrl Pts',(-7.26205090181683,3.13791932646799,118.227759119025));
#52039=CARTESIAN_POINT('Ctrl Pts',(-7.33915663979812,2.9594743966321,118.235554887356));
#52040=CARTESIAN_POINT('Ctrl Pts',(-7.40967038173992,2.77821079944886,118.243350655686));
#52041=CARTESIAN_POINT('Ctrl Pts',(-7.47339470106483,2.59466619088009,118.251146424017));
#52042=CARTESIAN_POINT('Ctrl Pts',(-7.5371375666491,2.41106816368006,118.258944461219));
#52043=CARTESIAN_POINT('Ctrl Pts',(-7.59408695844901,2.22518813702575,118.266742498422));
#52044=CARTESIAN_POINT('Ctrl Pts',(-7.64409526188591,2.03757910943684,118.274540535625));
#52045=CARTESIAN_POINT('Ctrl Pts',(-7.69415138836612,1.84979067094942,118.282346030106));
#52046=CARTESIAN_POINT('Ctrl Pts',(-7.73725307824949,1.66027027122004,118.290151524588));
#52047=CARTESIAN_POINT('Ctrl Pts',(-7.77330361370663,1.46958222945686,118.29795701907));
#52048=CARTESIAN_POINT('Ctrl Pts',(-7.80937339613195,1.27879238153119,118.305766680816));
#52049=CARTESIAN_POINT('Ctrl Pts',(-7.83838446918683,1.08683399817102,118.313576342562));
#52050=CARTESIAN_POINT('Ctrl Pts',(-7.8602919833563,0.894276767217355,118.321386004308));
#52051=CARTESIAN_POINT('Ctrl Pts',(-7.88222718161888,0.701476205492797,
118.329205534969));
#52052=CARTESIAN_POINT('Ctrl Pts',(-7.89704086536167,0.508075636413814,
118.33702506563));
#52053=CARTESIAN_POINT('Ctrl Pts',(-7.90474027759045,0.31464606121696,118.344844596291));
#52054=CARTESIAN_POINT('Ctrl Pts',(-7.90894924536154,0.208905671718469,
118.349119228115));
#52055=CARTESIAN_POINT('Ctrl Pts',(-7.91103310971454,0.103156567800752,
118.353393859939));
#52056=CARTESIAN_POINT('Ctrl Pts',(-7.91099960224048,-0.00250865522661604,
118.357668491763));
#52057=CARTESIAN_POINT('',(-7.9122673030836,0.00701237838125787,120.357668491763));
#52058=CARTESIAN_POINT('Ctrl Pts',(-7.92290232931793,-0.00251242969760849,
118.357668491763));
#52059=CARTESIAN_POINT('Ctrl Pts',(-7.92403808898173,-0.204144684807022,
118.365813150447));
#52060=CARTESIAN_POINT('Ctrl Pts',(-7.91699393318657,-0.405710916029759,
118.373957809132));
#52061=CARTESIAN_POINT('Ctrl Pts',(-7.69988300863637,-3.2236589545846,118.488179620565));
#52062=CARTESIAN_POINT('Ctrl Pts',(-4.43429229470843,-8.24372861963162,
118.700333926063));
#52063=CARTESIAN_POINT('Ctrl Pts',(3.02895942017901,-8.18612541628597,118.965526807936));
#52064=CARTESIAN_POINT('Ctrl Pts',(6.94408330637767,-4.40646303786943,119.177681113432));
#52065=CARTESIAN_POINT('Ctrl Pts',(8.69663683459128,0.745487939167516,119.389835418932));
#52066=CARTESIAN_POINT('Ctrl Pts',(5.57052227007294,7.52271834829018,119.655028300802));
#52067=CARTESIAN_POINT('Ctrl Pts',(-3.32864853973696,8.74804228169172,119.973259759051));
#52068=CARTESIAN_POINT('Ctrl Pts',(-7.61439352537567,3.73049070384629,120.207473156037));
#52069=CARTESIAN_POINT('Ctrl Pts',(-7.91716285885491,0.554684267022833,
120.335609400274));
#52070=CARTESIAN_POINT('Ctrl Pts',(-7.9122673030836,0.00701237838125787,
120.357668491763));
#52071=CARTESIAN_POINT('',(-7.90352584329644,7.42828143361043E-5,122.357668491763));
#52072=CARTESIAN_POINT('Ctrl Pts',(-7.9122673030836,0.00701237838125787,
120.357668491763));
#52073=CARTESIAN_POINT('Ctrl Pts',(-7.89362124484021,-2.07894525562691,
120.441686553023));
#52074=CARTESIAN_POINT('Ctrl Pts',(-5.97996265754411,-6.82958157585722,
120.631781767032));
#52075=CARTESIAN_POINT('Ctrl Pts',(2.05724953842661,-9.13179796347452,120.92795413379));
#52076=CARTESIAN_POINT('Ctrl Pts',(7.65449062796197,-4.19476074725102,121.193147015663));
#52077=CARTESIAN_POINT('Ctrl Pts',(8.13227400217734,1.22610318632951,121.40530132116));
#52078=CARTESIAN_POINT('Ctrl Pts',(6.07745315432454,6.26512630816728,121.61745562666));
#52079=CARTESIAN_POINT('Ctrl Pts',(-0.726601117103637,9.33241986440786,
121.88264850853));
#52080=CARTESIAN_POINT('Ctrl Pts',(-6.97710178777028,5.25280976497826,122.147065655691));
#52081=CARTESIAN_POINT('Ctrl Pts',(-7.89925698168475,1.30374424487291,122.305405650101));
#52082=CARTESIAN_POINT('Ctrl Pts',(-7.89821528668816,0.000127062427985106,
122.357668491763));
#52083=CARTESIAN_POINT('',(-7.911,-2.20379270388094E-12,124.357668491763));
#52084=CARTESIAN_POINT('Ctrl Pts',(-7.911,-2.37476704967321E-12,122.357668491763));
#52085=CARTESIAN_POINT('Ctrl Pts',(-7.91099999999934,-2.20167589666902,
122.446255927496));
#52086=CARTESIAN_POINT('Ctrl Pts',(-6.94214576672251,-4.38610418338868,
122.534843363229));
#52087=CARTESIAN_POINT('Ctrl Pts',(-3.67820201488108,-7.34180684107718,
122.712018234694));
#52088=CARTESIAN_POINT('Ctrl Pts',(-1.40868175871563,-8.08992666571365,
122.800605670427));
#52089=CARTESIAN_POINT('Ctrl Pts',(2.97309270521422,-7.65454228025196,122.977780541892));
#52090=CARTESIAN_POINT('Ctrl Pts',(5.05102072675715,-6.47444880834133,123.066367977625));
#52091=CARTESIAN_POINT('Ctrl Pts',(7.66951518847912,-2.93425195367592,123.24354284909));
#52092=CARTESIAN_POINT('Ctrl Pts',(8.18956872247076,-0.601881960098094,
123.332130284823));
#52093=CARTESIAN_POINT('Ctrl Pts',(7.32306689761302,3.71537198232523,123.509305156288));
#52094=CARTESIAN_POINT('Ctrl Pts',(5.94329958850151,5.66643518936559,123.597892592021));
#52095=CARTESIAN_POINT('Ctrl Pts',(2.16154501637802,7.92205913233007,123.775067463487));
#52096=CARTESIAN_POINT('Ctrl Pts',(-0.210816529300683,8.20894963712998,
123.863654899219));
#52097=CARTESIAN_POINT('Ctrl Pts',(-4.42123908576442,6.91982244717824,124.040829770685));
#52098=CARTESIAN_POINT('Ctrl Pts',(-6.22631625634181,5.35390358803523,124.129417206418));
#52099=CARTESIAN_POINT('Ctrl Pts',(-7.65317280859517,2.31334857514464,124.264559258688));
#52100=CARTESIAN_POINT('Ctrl Pts',(-7.91100000000032,1.15702837836378,124.311113875226));
#52101=CARTESIAN_POINT('Ctrl Pts',(-7.911,-2.20379270388094E-12,124.357668491763));
#52102=CARTESIAN_POINT('',(-7.91840974246489,0.00164577101414091,126.357721590925));
#52103=CARTESIAN_POINT('Ctrl Pts',(-7.911,-2.20379270388094E-12,124.357668491763));
#52104=CARTESIAN_POINT('Ctrl Pts',(-7.91099999999939,-2.20167589666915,
124.446255927496));
#52105=CARTESIAN_POINT('Ctrl Pts',(-6.94214576672232,-4.38610418338912,
124.534843363229));
#52106=CARTESIAN_POINT('Ctrl Pts',(-3.67820201488018,-7.34180684107772,
124.712018234694));
#52107=CARTESIAN_POINT('Ctrl Pts',(-1.40868175871426,-8.08992666571397,
124.800605670427));
#52108=CARTESIAN_POINT('Ctrl Pts',(2.97309270521609,-7.65454228025132,124.977780541892));
#52109=CARTESIAN_POINT('Ctrl Pts',(5.05102072675904,-6.47444880833996,125.066367977625));
#52110=CARTESIAN_POINT('Ctrl Pts',(7.66951518848024,-2.93425195367323,125.24354284909));
#52111=CARTESIAN_POINT('Ctrl Pts',(8.18956872247108,-0.60188196009484,125.332130284823));
#52112=CARTESIAN_POINT('Ctrl Pts',(7.32306689761135,3.7153719823287,125.509305156289));
#52113=CARTESIAN_POINT('Ctrl Pts',(5.94329958849867,5.66643518936869,125.597892592021));
#52114=CARTESIAN_POINT('Ctrl Pts',(2.16154501637343,7.9220591323314,125.775067463487));
#52115=CARTESIAN_POINT('Ctrl Pts',(-0.210816529305819,8.20894963712993,
125.86365489922));
#52116=CARTESIAN_POINT('Ctrl Pts',(-4.42123908576928,6.91982244717523,126.040829770685));
#52117=CARTESIAN_POINT('Ctrl Pts',(-6.22631625634583,5.35390358803068,126.129417206418));
#52118=CARTESIAN_POINT('Ctrl Pts',(-7.65293518925909,2.31385492924122,126.264536753016));
#52119=CARTESIAN_POINT('Ctrl Pts',(-7.91075066509672,1.15814634139517,126.311068863883));
#52120=CARTESIAN_POINT('Ctrl Pts',(-7.9109998192402,0.00167800926889546,
126.357600974748));
#52121=CARTESIAN_POINT('',(-7.90392088591637,0.0024881653853563,128.357668491763));
#52122=CARTESIAN_POINT('Ctrl Pts',(-7.92352486655139,0.00162351671157913,
126.357804853153));
#52123=CARTESIAN_POINT('Ctrl Pts',(-7.91094766732972,-2.45855671784116,
126.457243362846));
#52124=CARTESIAN_POINT('Ctrl Pts',(-5.34962893444157,-7.57264949493443,
126.662759025289));
#52125=CARTESIAN_POINT('Ctrl Pts',(3.35234681176765,-8.73179419511677,126.97435184048));
#52126=CARTESIAN_POINT('Ctrl Pts',(9.16409439033137,-1.90460464885401,127.292583298727));
#52127=CARTESIAN_POINT('Ctrl Pts',(6.54805283706349,6.68917138008194,127.610814756974));
#52128=CARTESIAN_POINT('Ctrl Pts',(-0.637984975502353,8.70518349440442,
127.876007638845));
#52129=CARTESIAN_POINT('Ctrl Pts',(-5.4483076350138,6.16061306886672,128.088161944344));
#52130=CARTESIAN_POINT('Ctrl Pts',(-7.54512756758505,3.15493213566288,128.231036036525));
#52131=CARTESIAN_POINT('Ctrl Pts',(-7.90452149261816,0.920835889764306,
128.320871552331));
#52132=CARTESIAN_POINT('Ctrl Pts',(-7.89890066374168,0.00425267191875162,
128.357668491763));
#52133=CARTESIAN_POINT('',(-7.9109995580894,-0.00186974719043329,130.357668491763));
#52134=CARTESIAN_POINT('Ctrl Pts',(-7.911,-1.86295423532101E-12,128.357668491763));
#52135=CARTESIAN_POINT('Ctrl Pts',(-7.91099999999948,-2.20167589666851,
128.446255927496));
#52136=CARTESIAN_POINT('Ctrl Pts',(-6.94214576672279,-4.38610418338823,
128.534843363229));
#52137=CARTESIAN_POINT('Ctrl Pts',(-3.67820201488156,-7.34180684107694,
128.712018234694));
#52138=CARTESIAN_POINT('Ctrl Pts',(-1.40868175871615,-8.08992666571356,
128.800605670427));
#52139=CARTESIAN_POINT('Ctrl Pts',(2.97309270521372,-7.65454228025215,128.977780541892));
#52140=CARTESIAN_POINT('Ctrl Pts',(5.05102072675673,-6.47444880834166,129.066367977625));
#52141=CARTESIAN_POINT('Ctrl Pts',(7.66951518847893,-2.93425195367641,129.24354284909));
#52142=CARTESIAN_POINT('Ctrl Pts',(8.18956872247072,-0.601881960098624,
129.332130284823));
#52143=CARTESIAN_POINT('Ctrl Pts',(7.32306689761326,3.71537198232476,129.509305156288));
#52144=CARTESIAN_POINT('Ctrl Pts',(5.94329958850188,5.6664351893652,129.597892592021));
#52145=CARTESIAN_POINT('Ctrl Pts',(2.16154501637854,7.92205913232993,129.775067463487));
#52146=CARTESIAN_POINT('Ctrl Pts',(-0.210816529300152,8.20894963713,129.863654899219));
#52147=CARTESIAN_POINT('Ctrl Pts',(-4.42123908576398,6.91982244717853,130.040829770685));
#52148=CARTESIAN_POINT('Ctrl Pts',(-6.22631625634147,5.35390358803564,130.129417206418));
#52149=CARTESIAN_POINT('Ctrl Pts',(-7.65317280859502,2.31334857514513,130.264559258688));
#52150=CARTESIAN_POINT('Ctrl Pts',(-7.91100000000025,1.15702837836429,130.311113875225));
#52151=CARTESIAN_POINT('Ctrl Pts',(-7.911,-1.69197988952874E-12,130.357668491763));
#52152=CARTESIAN_POINT('',(-7.91099991273041,-0.00117506573469943,132.357550177074));
#52153=CARTESIAN_POINT('Ctrl Pts',(-7.9109991161788,-0.00373949437917459,
130.357668491763));
#52154=CARTESIAN_POINT('Ctrl Pts',(-7.91089584571042,-0.222210897528256,
130.366434366415));
#52155=CARTESIAN_POINT('Ctrl Pts',(-7.90173845183842,-0.440413092802176,
130.375200241067));
#52156=CARTESIAN_POINT('Ctrl Pts',(-7.88361836605496,-0.657633985132213,
130.38396611572));
#52157=CARTESIAN_POINT('Ctrl Pts',(-7.86541916559622,-0.875803292418298,
130.392770263332));
#52158=CARTESIAN_POINT('Ctrl Pts',(-7.83817890181611,-1.0929825126435,130.401574410945));
#52159=CARTESIAN_POINT('Ctrl Pts',(-7.80204093071744,-1.30846410551064,
130.410378558558));
#52160=CARTESIAN_POINT('Ctrl Pts',(-7.76582530704639,-1.52440872105108,
130.419201624352));
#52161=CARTESIAN_POINT('Ctrl Pts',(-7.72067378382519,-1.7386482197866,130.428024690147));
#52162=CARTESIAN_POINT('Ctrl Pts',(-7.66678030483148,-1.95048731281392,
130.436847755941));
#52163=CARTESIAN_POINT('Ctrl Pts',(-7.6127392364279,-2.16290653552136,130.445694984048));
#52164=CARTESIAN_POINT('Ctrl Pts',(-7.54990835301261,-2.37291200415262,
130.454542212155));
#52165=CARTESIAN_POINT('Ctrl Pts',(-7.47853177456327,-2.57982237699567,
130.463389440262));
#52166=CARTESIAN_POINT('Ctrl Pts',(-7.4475829799364,-2.66953845437577,130.46722558724));
#52167=CARTESIAN_POINT('Ctrl Pts',(-7.41502813651028,-2.75867289557034,
130.471061734217));
#52168=CARTESIAN_POINT('Ctrl Pts',(-7.38088990741013,-2.84717143401856,
130.474897881195));
#52169=CARTESIAN_POINT('Ctrl Pts',(-7.31050072308688,-3.02964545506092,
130.4828075843));
#52170=CARTESIAN_POINT('Ctrl Pts',(-7.23325150427447,-3.20973885994879,
130.490717287405));
#52171=CARTESIAN_POINT('Ctrl Pts',(-7.14932378069951,-3.38689983299247,
130.498626990509));
#52172=CARTESIAN_POINT('Ctrl Pts',(-7.065481205891,-3.56388106759366,130.506528668835));
#52173=CARTESIAN_POINT('Ctrl Pts',(-6.97497376930275,-3.73793548763144,
130.51443034716));
#52174=CARTESIAN_POINT('Ctrl Pts',(-6.87803195930351,-3.90852879825639,
130.522332025486));
#52175=CARTESIAN_POINT('Ctrl Pts',(-6.78117054281328,-4.07898063643663,
130.530227150976));
#52176=CARTESIAN_POINT('Ctrl Pts',(-6.67788555241016,-4.24597678534226,
130.538122276467));
#52177=CARTESIAN_POINT('Ctrl Pts',(-6.56845463156288,-4.40900496179128,
130.546017401958));
#52178=CARTESIAN_POINT('Ctrl Pts',(-6.45909419461557,-4.57192813262039,
130.553907442239));
#52179=CARTESIAN_POINT('Ctrl Pts',(-6.34359590571145,-4.73088813800196,
130.561797482519));
#52180=CARTESIAN_POINT('Ctrl Pts',(-6.22228234214997,-4.8853990066901,130.5696875228));
#52181=CARTESIAN_POINT('Ctrl Pts',(-6.10102445301144,-5.03983896571901,
130.577573942105));
#52182=CARTESIAN_POINT('Ctrl Pts',(-5.97395681976943,-5.18983358636831,
130.58546036141));
#52183=CARTESIAN_POINT('Ctrl Pts',(-5.84144433471934,-5.33492728013938,
130.593346780715));
#52184=CARTESIAN_POINT('Ctrl Pts',(-5.70896813049634,-5.47998124845201,
130.601231040784));
#52185=CARTESIAN_POINT('Ctrl Pts',(-5.57105027794571,-5.62013671017715,
130.609115300852));
#52186=CARTESIAN_POINT('Ctrl Pts',(-5.42809499169923,-5.754972264146,130.616999560921));
#52187=CARTESIAN_POINT('Ctrl Pts',(-5.28512301549902,-5.88982356009414,
130.624884741472));
#52188=CARTESIAN_POINT('Ctrl Pts',(-5.13711267647559,-6.01935346576271,
130.632769922024));
#52189=CARTESIAN_POINT('Ctrl Pts',(-4.9845044470491,-6.14317803887758,130.640655102576));
#52190=CARTESIAN_POINT('Ctrl Pts',(-4.83187718287227,-6.26701805657131,
130.648541266642));
#52191=CARTESIAN_POINT('Ctrl Pts',(-4.67465115286065,-6.38515110588662,
130.656427430708));
#52192=CARTESIAN_POINT('Ctrl Pts',(-4.51329922275996,-6.49723411351587,
130.664313594775));
#52193=CARTESIAN_POINT('Ctrl Pts',(-4.35190009526084,-6.60934990678559,
130.67220206564));
#52194=CARTESIAN_POINT('Ctrl Pts',(-4.1863729457104,-6.71541193506504,130.680090536505));
#52195=CARTESIAN_POINT('Ctrl Pts',(-4.01721906877824,-6.81512083190346,
130.68797900737));
#52196=CARTESIAN_POINT('Ctrl Pts',(-3.84798733056831,-6.91487562459868,
130.695871109287));
#52197=CARTESIAN_POINT('Ctrl Pts',(-3.67512583497725,-7.00827128357385,
130.703763211203));
#52198=CARTESIAN_POINT('Ctrl Pts',(-3.49916008761638,-7.09505459325244,
130.71165531312));
#52199=CARTESIAN_POINT('Ctrl Pts',(-3.32299034286489,-7.18193851096975,
130.719556564363));
#52200=CARTESIAN_POINT('Ctrl Pts',(-3.14370946715935,-7.26219461505559,
130.727457815607));
#52201=CARTESIAN_POINT('Ctrl Pts',(-2.96186361816154,-7.33561755460377,
130.735359066851));
#52202=CARTESIAN_POINT('Ctrl Pts',(-2.7798972727856,-7.40908914633916,130.743265553695));
#52203=CARTESIAN_POINT('Ctrl Pts',(-2.59536288892839,-7.47571843030834,
130.751172040539));
#52204=CARTESIAN_POINT('Ctrl Pts',(-2.40882160273842,-7.53534999095468,
130.759078527382));
#52205=CARTESIAN_POINT('Ctrl Pts',(-2.22202332497055,-7.59506370397155,
130.766995906724));
#52206=CARTESIAN_POINT('Ctrl Pts',(-2.03321295306132,-7.64776034514328,
130.774913286066));
#52207=CARTESIAN_POINT('Ctrl Pts',(-1.84296278608913,-7.69333537349637,
130.782830665407));
#52208=CARTESIAN_POINT('Ctrl Pts',(-1.76047234027415,-7.71309622031564,
130.786263556752));
#52209=CARTESIAN_POINT('Ctrl Pts',(-1.67771129521446,-7.73151886537192,
130.789696448097));
#52210=CARTESIAN_POINT('Ctrl Pts',(-1.5947265676748,-7.74859781988665,130.793129339442));
#52211=CARTESIAN_POINT('Ctrl Pts',(-1.40516762552119,-7.78761064365418,
130.800970966102));
#52212=CARTESIAN_POINT('Ctrl Pts',(-1.21387764991051,-7.81972476370473,
130.808812592763));
#52213=CARTESIAN_POINT('Ctrl Pts',(-1.0214060498034,-7.84478493532009,130.816654219423));
#52214=CARTESIAN_POINT('Ctrl Pts',(-0.829161070503838,-7.86981560047151,
130.824486613159));
#52215=CARTESIAN_POINT('Ctrl Pts',(-0.635737581738321,-7.88780880983657,
130.832319006895));
#52216=CARTESIAN_POINT('Ctrl Pts',(-0.441698015690497,-7.89865962445117,
130.84015140063));
#52217=CARTESIAN_POINT('Ctrl Pts',(-0.24784914332251,-7.90949977535522,
130.847976097029));
#52218=CARTESIAN_POINT('Ctrl Pts',(-0.0533857477400354,-7.9132114901666,
130.855800793427));
#52219=CARTESIAN_POINT('Ctrl Pts',(0.141121535392811,-7.90974119123049,
130.863625489826));
#52220=CARTESIAN_POINT('Ctrl Pts',(0.335475506750435,-7.90627362760425,
130.871444018753));
#52221=CARTESIAN_POINT('Ctrl Pts',(0.529872946920586,-7.89563533112102,
130.87926254768));
#52222=CARTESIAN_POINT('Ctrl Pts',(0.723739917486823,-7.87782467003653,
130.887081076607));
#52223=CARTESIAN_POINT('Ctrl Pts',(0.91749178239512,-7.8600245837697,130.894894963398));
#52224=CARTESIAN_POINT('Ctrl Pts',(1.11071345589391,-7.83506064775668,130.902708850189));
#52225=CARTESIAN_POINT('Ctrl Pts',(1.30283263211802,-7.8029832841477,130.910522736979));
#52226=CARTESIAN_POINT('Ctrl Pts',(1.49487509151544,-7.7709187296377,130.918333503537));
#52227=CARTESIAN_POINT('Ctrl Pts',(1.68581558435728,-7.73174646473343,130.926144270095));
#52228=CARTESIAN_POINT('Ctrl Pts',(1.87508836052272,-7.6855685957665,130.933955036653));
#52229=CARTESIAN_POINT('Ctrl Pts',(2.06435361401569,-7.63939256214531,130.94176549277));
#52230=CARTESIAN_POINT('Ctrl Pts',(2.25195093909346,-7.58621155371739,130.949575948888));
#52231=CARTESIAN_POINT('Ctrl Pts',(2.43732573229109,-7.52617859705121,130.957386405006));
#52232=CARTESIAN_POINT('Ctrl Pts',(2.62270563776668,-7.46614398479229,130.965197076521));
#52233=CARTESIAN_POINT('Ctrl Pts',(2.80586255415591,-7.39925715556025,130.973007748036));
#52234=CARTESIAN_POINT('Ctrl Pts',(2.98625800853511,-7.3257207226634,130.980818419551));
#52235=CARTESIAN_POINT('Ctrl Pts',(3.16669020807862,-7.25216931096168,130.98863068204));
#52236=CARTESIAN_POINT('Ctrl Pts',(3.34435949920978,-7.17196573023374,130.996442944528));
#52237=CARTESIAN_POINT('Ctrl Pts',(3.51874818786322,-7.08536041358584,131.004255207017));
#52238=CARTESIAN_POINT('Ctrl Pts',(3.69320311273072,-6.99872220255507,131.012070436755));
#52239=CARTESIAN_POINT('Ctrl Pts',(3.8643746381874,-6.90567756858897,131.019885666492));
#52240=CARTESIAN_POINT('Ctrl Pts',(4.03177030139072,-6.80652255096711,131.02770089623));
#52241=CARTESIAN_POINT('Ctrl Pts',(4.19934801550418,-6.70725969744999,131.03552462541));
#52242=CARTESIAN_POINT('Ctrl Pts',(4.36314136278643,-6.60187336698383,131.043348354589));
#52243=CARTESIAN_POINT('Ctrl Pts',(4.52268659483622,-6.49070311791325,131.051172083769));
#52244=CARTESIAN_POINT('Ctrl Pts',(4.68232862674443,-6.37946541922833,131.059000559789));
#52245=CARTESIAN_POINT('Ctrl Pts',(4.83771712665129,-6.26243701939575,131.06682903581));
#52246=CARTESIAN_POINT('Ctrl Pts',(4.98842195556946,-6.13999734472195,131.074657511831));
#52247=CARTESIAN_POINT('Ctrl Pts',(5.13933419656986,-6.01738915873996,131.082496762028));
#52248=CARTESIAN_POINT('Ctrl Pts',(5.28554962778369,-5.88935505378018,131.090336012226));
#52249=CARTESIAN_POINT('Ctrl Pts',(5.42667462170755,-5.75631162725883,131.098175262424));
#52250=CARTESIAN_POINT('Ctrl Pts',(5.50579820016106,-5.68171908554531,131.102570440846));
#52251=CARTESIAN_POINT('Ctrl Pts',(5.58332234328611,-5.60555251584328,131.106965619267));
#52252=CARTESIAN_POINT('Ctrl Pts',(5.65918333546722,-5.52788973981665,131.111360797689));
#52253=CARTESIAN_POINT('Ctrl Pts',(5.79570831695938,-5.38812213653572,131.119270681746));
#52254=CARTESIAN_POINT('Ctrl Pts',(5.92723666008975,-5.24310511329249,131.127180565804));
#52255=CARTESIAN_POINT('Ctrl Pts',(6.05334027917667,-5.09323006200361,131.135090449862));
#52256=CARTESIAN_POINT('Ctrl Pts',(6.17930680248239,-4.94351795002915,131.142991734549));
#52257=CARTESIAN_POINT('Ctrl Pts',(6.29986012868711,-4.78895859143482,131.150893019237));
#52258=CARTESIAN_POINT('Ctrl Pts',(6.41460818253311,-4.62998087086537,131.158794303924));
#52259=CARTESIAN_POINT('Ctrl Pts',(6.52925280895531,-4.47114644384671,131.166688466839));
#52260=CARTESIAN_POINT('Ctrl Pts',(6.63810238601186,-4.3079018661502,131.174582629754));
#52261=CARTESIAN_POINT('Ctrl Pts',(6.7408042137958,-4.14071002984668,131.182476792669));
#52262=CARTESIAN_POINT('Ctrl Pts',(6.84343255045384,-3.97363783227359,131.190365306698));
#52263=CARTESIAN_POINT('Ctrl Pts',(6.9399217226487,-3.80262429629234,131.198253820727));
#52264=CARTESIAN_POINT('Ctrl Pts',(7.02996142529944,-3.62816253202662,131.206142334756));
#52265=CARTESIAN_POINT('Ctrl Pts',(7.11995342011652,-3.45379320690259,131.214026669029));
#52266=CARTESIAN_POINT('Ctrl Pts',(7.20350259688611,-3.27597959993413,131.221911003303));
#52267=CARTESIAN_POINT('Ctrl Pts',(7.2803436920171,-3.09524098029651,131.229795337577));
#52268=CARTESIAN_POINT('Ctrl Pts',(7.35715834156725,-2.91456456354353,131.237676958383));
#52269=CARTESIAN_POINT('Ctrl Pts',(7.42726937585404,-2.73096545751856,131.24555857919));
#52270=CARTESIAN_POINT('Ctrl Pts',(7.4904588226988,-2.54498479866848,131.253440199996));
#52271=CARTESIAN_POINT('Ctrl Pts',(7.55364909715867,-2.35900170396226,131.261321924031));
#52272=CARTESIAN_POINT('Ctrl Pts',(7.60991748396962,-2.17063731795321,131.269203648066));
#52273=CARTESIAN_POINT('Ctrl Pts',(7.65909505259427,-1.98045044758155,131.2770853721));
#52274=CARTESIAN_POINT('Ctrl Pts',(7.70827558368472,-1.79025212031777,131.284967570932));
#52275=CARTESIAN_POINT('Ctrl Pts',(7.7503643584307,-1.59823142396163,131.292849769763));
#52276=CARTESIAN_POINT('Ctrl Pts',(7.78524299391339,-1.40495997299656,131.300731968595));
#52277=CARTESIAN_POINT('Ctrl Pts',(7.82012959953032,-1.2116443574767,131.308615968591));
#52278=CARTESIAN_POINT('Ctrl Pts',(7.84780272151483,-1.01707775743535,131.316499968588));
#52279=CARTESIAN_POINT('Ctrl Pts',(7.86819549346673,-0.821839812001022,
131.324383968584));
#52280=CARTESIAN_POINT('Ctrl Pts',(7.88859635692385,-0.626524399469087,
131.332271096818));
#52281=CARTESIAN_POINT('Ctrl Pts',(7.90171107851393,-0.430537453695613,
131.340158225052));
#52282=CARTESIAN_POINT('Ctrl Pts',(7.90752481319848,-0.23446178505328,131.348045353285));
#52283=CARTESIAN_POINT('Ctrl Pts',(7.91334475047378,-0.0381769260717599,
131.355940896184));
#52284=CARTESIAN_POINT('Ctrl Pts',(7.91184813204109,0.158196499830445,131.363836439082));
#52285=CARTESIAN_POINT('Ctrl Pts',(7.90307223937577,0.354076516035831,131.371731981981));
#52286=CARTESIAN_POINT('Ctrl Pts',(7.89429100249589,0.550075816384149,131.379632332991));
#52287=CARTESIAN_POINT('Ctrl Pts',(7.87822168216327,0.745580765039928,131.387532684002));
#52288=CARTESIAN_POINT('Ctrl Pts',(7.85495325136521,0.940016180109228,131.395433035012));
#52289=CARTESIAN_POINT('Ctrl Pts',(7.83165452409203,1.13470475826316,131.403343672612));
#52290=CARTESIAN_POINT('Ctrl Pts',(7.80113801678985,1.32832068145589,131.411254310212));
#52291=CARTESIAN_POINT('Ctrl Pts',(7.76354368293116,1.52029947155803,131.419164947812));
#52292=CARTESIAN_POINT('Ctrl Pts',(7.74702551576303,1.60465095280951,131.422640717186));
#52293=CARTESIAN_POINT('Ctrl Pts',(7.72914159403645,1.68868657702022,131.42611648656));
#52294=CARTESIAN_POINT('Ctrl Pts',(7.70990679523191,1.77235950327152,131.429592255935));
#52295=CARTESIAN_POINT('Ctrl Pts',(7.66613384772448,1.96277535559263,131.437502121378));
#52296=CARTESIAN_POINT('Ctrl Pts',(7.61524342536188,2.15182559266713,131.445411986822));
#52297=CARTESIAN_POINT('Ctrl Pts',(7.55733337608319,2.33893848630933,131.453321852265));
#52298=CARTESIAN_POINT('Ctrl Pts',(7.49948626300756,2.52584802707557,131.461223121327));
#52299=CARTESIAN_POINT('Ctrl Pts',(7.43463481955377,2.71082409164834,131.469124390388));
#52300=CARTESIAN_POINT('Ctrl Pts',(7.36292790276842,2.89330497850368,131.47702565945));
#52301=CARTESIAN_POINT('Ctrl Pts',(7.29128559165454,3.07562145583268,131.484919809717));
#52302=CARTESIAN_POINT('Ctrl Pts',(7.2128002367439,3.25544691474066,131.492813959985));
#52303=CARTESIAN_POINT('Ctrl Pts',(7.12767059110865,3.4322343953531,131.500708110252));
#52304=CARTESIAN_POINT('Ctrl Pts',(7.04260183041424,3.60889543710611,131.508596614603));
#52305=CARTESIAN_POINT('Ctrl Pts',(6.95089839561357,3.78252251989815,131.516485118953));
#52306=CARTESIAN_POINT('Ctrl Pts',(6.8528073801641,3.95258801424693,131.524373623304));
#52307=CARTESIAN_POINT('Ctrl Pts',(6.75476830178432,4.12256346259718,131.532257950862));
#52308=CARTESIAN_POINT('Ctrl Pts',(6.65034855391276,4.28898078204876,131.540142278421));
#52309=CARTESIAN_POINT('Ctrl Pts',(6.53984158637937,4.45133609437245,131.548026605979));
#52310=CARTESIAN_POINT('Ctrl Pts',(6.42937260942353,4.61363559146366,131.555908223028));
#52311=CARTESIAN_POINT('Ctrl Pts',(6.3128207774534,4.77187557975789,131.563789840078));
#52312=CARTESIAN_POINT('Ctrl Pts',(6.1905235023506,4.92558014520573,131.571671457127));
#52313=CARTESIAN_POINT('Ctrl Pts',(6.06822455680444,5.07928681008522,131.57955318183));
#52314=CARTESIAN_POINT('Ctrl Pts',(5.94018021939878,5.22845765309482,131.587434906533));
#52315=CARTESIAN_POINT('Ctrl Pts',(5.80676927975302,5.37264846530243,131.595316631236));
#52316=CARTESIAN_POINT('Ctrl Pts',(5.67335025673447,5.51684801403565,131.603198833494));
#52317=CARTESIAN_POINT('Ctrl Pts',(5.53456421752344,5.65606667693122,131.611081035751));
#52318=CARTESIAN_POINT('Ctrl Pts',(5.39082805225096,5.78989584630537,131.618963238008));
#52319=CARTESIAN_POINT('Ctrl Pts',(5.24705899146809,5.92375564387126,131.626847244189));
#52320=CARTESIAN_POINT('Ctrl Pts',(5.09833779973761,6.05222325493353,131.634731250369));
#52321=CARTESIAN_POINT('Ctrl Pts',(4.94511596769183,6.17492907376913,131.64261525655));
#52322=CARTESIAN_POINT('Ctrl Pts',(4.79183328621712,6.29768362312115,131.650502393729));
#52323=CARTESIAN_POINT('Ctrl Pts',(4.63404667210869,6.4146716052893,131.658389530908));
#52324=CARTESIAN_POINT('Ctrl Pts',(4.47223840631225,6.52556546493142,131.666276668087));
#52325=CARTESIAN_POINT('Ctrl Pts',(4.31025742502092,6.6365776936059,131.674172224062));
#52326=CARTESIAN_POINT('Ctrl Pts',(4.14424650233152,6.7414826115451,131.682067780037));
#52327=CARTESIAN_POINT('Ctrl Pts',(3.9747153972542,6.83999696716529,131.689963336012));
#52328=CARTESIAN_POINT('Ctrl Pts',(3.80508100274972,6.93857134416831,131.697863702476));
#52329=CARTESIAN_POINT('Ctrl Pts',(3.6319224538412,7.03074723486181,131.70576406894));
#52330=CARTESIAN_POINT('Ctrl Pts',(3.45577173724022,7.11628854811915,131.713664435403));
#52331=CARTESIAN_POINT('Ctrl Pts',(3.27939158677093,7.20194127775207,131.721575091985));
#52332=CARTESIAN_POINT('Ctrl Pts',(3.10001179885957,7.28094203051928,131.729485748566));
#52333=CARTESIAN_POINT('Ctrl Pts',(2.91818291514442,7.35310339066161,131.737396405148));
#52334=CARTESIAN_POINT('Ctrl Pts',(2.83829127605092,7.38480951580077,131.740872174826));
#52335=CARTESIAN_POINT('Ctrl Pts',(2.75792701517316,7.41519592730195,131.744347944504));
#52336=CARTESIAN_POINT('Ctrl Pts',(2.67713758109783,7.44424981928157,131.747823714182));
#52337=CARTESIAN_POINT('Ctrl Pts',(2.49493491938076,7.50977443289615,131.755662542292));
#52338=CARTESIAN_POINT('Ctrl Pts',(2.31004995145518,7.56870469733447,131.763501370403));
#52339=CARTESIAN_POINT('Ctrl Pts',(2.12300593910925,7.62081142546559,131.771340198513));
#52340=CARTESIAN_POINT('Ctrl Pts',(1.93617160020406,7.67285974276154,131.779170239419));
#52341=CARTESIAN_POINT('Ctrl Pts',(1.74718337136202,7.71809966122804,131.787000280324));
#52342=CARTESIAN_POINT('Ctrl Pts',(1.55658426346542,7.75635007144029,131.79483032123));
#52343=CARTESIAN_POINT('Ctrl Pts',(1.36616171838287,7.79456504811804,131.802653108722));
#52344=CARTESIAN_POINT('Ctrl Pts',(1.17413160834321,7.82580334203642,131.810475896215));
#52345=CARTESIAN_POINT('Ctrl Pts',(0.981052061062631,7.84993362096042,131.818298683707));
#52346=CARTESIAN_POINT('Ctrl Pts',(0.788113815986769,7.87404624052246,131.826115746217));
#52347=CARTESIAN_POINT('Ctrl Pts',(0.594128010749377,7.89106116234817,131.833932808726));
#52348=CARTESIAN_POINT('Ctrl Pts',(0.399663113605735,7.90089807525847,131.841749871236));
#52349=CARTESIAN_POINT('Ctrl Pts',(0.205302718527595,7.91072970198225,131.849562732991));
#52350=CARTESIAN_POINT('Ctrl Pts',(0.010464094781512,7.91339098596106,131.857375594747));
#52351=CARTESIAN_POINT('Ctrl Pts',(-0.184278823972296,7.90885341342444,
131.865188456502));
#52352=CARTESIAN_POINT('Ctrl Pts',(-0.378954949974643,7.90431739718038,
131.87299863861));
#52353=CARTESIAN_POINT('Ctrl Pts',(-0.573535085160128,7.8925874520569,131.880808820717));
#52354=CARTESIAN_POINT('Ctrl Pts',(-0.76744475834389,7.87368716313332,131.888619002824));
#52355=CARTESIAN_POINT('Ctrl Pts',(-0.961363176978565,7.85478602179457,
131.896429537175));
#52356=CARTESIAN_POINT('Ctrl Pts',(-1.15461072218794,7.82871391549095,131.904240071527));
#52357=CARTESIAN_POINT('Ctrl Pts',(-1.34661698864132,7.79554640072796,131.912050605879));
#52358=CARTESIAN_POINT('Ctrl Pts',(-1.5386386445773,7.76237622755751,131.919861766252));
#52359=CARTESIAN_POINT('Ctrl Pts',(-1.72941847653137,7.72210957215602,131.927672926625));
#52360=CARTESIAN_POINT('Ctrl Pts',(-1.91839531990764,7.67487331469103,131.935484086998));
#52361=CARTESIAN_POINT('Ctrl Pts',(-2.10742059250838,7.62762495195814,131.943297249142));
#52362=CARTESIAN_POINT('Ctrl Pts',(-2.29464161464747,7.57340351430882,131.951110411287));
#52363=CARTESIAN_POINT('Ctrl Pts',(-2.47951130771365,7.51238608398957,131.958923573432));
#52364=CARTESIAN_POINT('Ctrl Pts',(-2.66446093954404,7.45134226936744,131.966740114034));
#52365=CARTESIAN_POINT('Ctrl Pts',(-2.84705688312377,7.38349671838267,131.974556654637));
#52366=CARTESIAN_POINT('Ctrl Pts',(-3.02677085724862,7.30907512464542,131.98237319524));
#52367=CARTESIAN_POINT('Ctrl Pts',(-3.20669456085284,7.23456667955348,131.990198857888));
#52368=CARTESIAN_POINT('Ctrl Pts',(-3.38372925235048,7.1534669984069,131.998024520535));
#52369=CARTESIAN_POINT('Ctrl Pts',(-3.55736914106945,7.06604881062725,132.005850183183));
#52370=CARTESIAN_POINT('Ctrl Pts',(-3.73112221384284,6.97857364086612,132.013680946849));
#52371=CARTESIAN_POINT('Ctrl Pts',(-3.90147576696341,6.88477192596603,132.021511710515));
#52372=CARTESIAN_POINT('Ctrl Pts',(-4.06795189917533,6.78496045279527,132.029342474182));
#52373=CARTESIAN_POINT('Ctrl Pts',(-4.23466857189771,6.68500476253833,132.037184552478));
#52374=CARTESIAN_POINT('Ctrl Pts',(-4.39749634006955,6.57902216146759,132.045026630774));
#52375=CARTESIAN_POINT('Ctrl Pts',(-4.55598839936478,6.46737123604743,132.052868709071));
#52376=CARTESIAN_POINT('Ctrl Pts',(-4.64482325723005,6.40479085104686,132.057264196857));
#52377=CARTESIAN_POINT('Ctrl Pts',(-4.73229662514873,6.34043040864525,132.061659684643));
#52378=CARTESIAN_POINT('Ctrl Pts',(-4.81833483756805,6.27435816582685,132.066055172429));
#52379=CARTESIAN_POINT('Ctrl Pts',(-4.97183518733137,6.15647900380008,132.073897140475));
#52380=CARTESIAN_POINT('Ctrl Pts',(-5.12124346991903,6.03278191119074,132.081739108521));
#52381=CARTESIAN_POINT('Ctrl Pts',(-5.26608374474064,5.90358221704233,132.089581076568));
#52382=CARTESIAN_POINT('Ctrl Pts',(-5.41075677738981,5.77453170541622,132.097413989758));
#52383=CARTESIAN_POINT('Ctrl Pts',(-5.5508720452749,5.63999147576539,132.105246902949));
#52384=CARTESIAN_POINT('Ctrl Pts',(-5.68598331006465,5.50031951777952,132.113079816139));
#52385=CARTESIAN_POINT('Ctrl Pts',(-5.82096490632567,5.3607816052955,132.120905211953));
#52386=CARTESIAN_POINT('Ctrl Pts',(-5.95095182064843,5.21612202379973,132.128730607766));
#52387=CARTESIAN_POINT('Ctrl Pts',(-6.07553145825877,5.06673844792763,132.13655600358));
#52388=CARTESIAN_POINT('Ctrl Pts',(-6.20001580688461,4.91746913317812,132.144375413873));
#52389=CARTESIAN_POINT('Ctrl Pts',(-6.31910089240349,4.76348329009855,132.152194824165));
#52390=CARTESIAN_POINT('Ctrl Pts',(-6.43241139925501,4.60521493426032,132.160014234458));
#52391=CARTESIAN_POINT('Ctrl Pts',(-6.54565730415862,4.44703681227915,132.167829186654));
#52392=CARTESIAN_POINT('Ctrl Pts',(-6.65313498475536,4.28458132700701,132.175644138851));
#52393=CARTESIAN_POINT('Ctrl Pts',(-6.75450970018044,4.1183151543038,132.183459091047));
#52394=CARTESIAN_POINT('Ctrl Pts',(-6.85585384782215,3.95209911627498,132.191271686781));
#52395=CARTESIAN_POINT('Ctrl Pts',(-6.9510985106699,3.78207497844818,132.199084282514));
#52396=CARTESIAN_POINT('Ctrl Pts',(-7.03995238370444,3.60873820540839,132.206896878248));
#52397=CARTESIAN_POINT('Ctrl Pts',(-7.12879453234187,3.43542430440661,132.214708443098));
#52398=CARTESIAN_POINT('Ctrl Pts',(-7.21124740971074,3.25879895178036,132.222520007948));
#52399=CARTESIAN_POINT('Ctrl Pts',(-7.28706571365825,3.07938212712005,132.230331572798));
#52400=CARTESIAN_POINT('Ctrl Pts',(-7.36288738445613,2.89995733512769,132.238143484535));
#52401=CARTESIAN_POINT('Ctrl Pts',(-7.43207375820792,2.71774114864288,132.245955396272));
#52402=CARTESIAN_POINT('Ctrl Pts',(-7.49442766561047,2.53327356693516,132.253767308009));
#52403=CARTESIAN_POINT('Ctrl Pts',(-7.55679533896533,2.34876526008225,132.261580944392));
#52404=CARTESIAN_POINT('Ctrl Pts',(-7.61232742948562,2.1620049016543,132.269394580775));
#52405=CARTESIAN_POINT('Ctrl Pts',(-7.66087657969628,1.9735478283186,132.277208217158));
#52406=CARTESIAN_POINT('Ctrl Pts',(-7.70946566857206,1.78493572191003,132.285028281381));
#52407=CARTESIAN_POINT('Ctrl Pts',(-7.75106025658121,1.59462445409737,132.292848345605));
#52408=CARTESIAN_POINT('Ctrl Pts',(-7.78556389772135,1.40318059938765,132.300668409828));
#52409=CARTESIAN_POINT('Ctrl Pts',(-7.82008381387908,1.21164644255335,132.308492162697));
#52410=CARTESIAN_POINT('Ctrl Pts',(-7.84750606669332,1.01897898190208,132.316315915566));
#52411=CARTESIAN_POINT('Ctrl Pts',(-7.86778606549067,0.82575022111459,132.324139668434));
#52412=CARTESIAN_POINT('Ctrl Pts',(-7.88808855803473,0.63230713887447,132.33197209909));
#52413=CARTESIAN_POINT('Ctrl Pts',(-7.90123295178609,0.43830186352041,132.339804529746));
#52414=CARTESIAN_POINT('Ctrl Pts',(-7.90722674356102,0.244307646039636,
132.347636960401));
#52415=CARTESIAN_POINT('Ctrl Pts',(-7.90975545013015,0.162463886606973,
132.350941365959));
#52416=CARTESIAN_POINT('Ctrl Pts',(-7.91101206252141,0.080622056533713,
132.354245771516));
#52417=CARTESIAN_POINT('Ctrl Pts',(-7.91099991273041,-0.00117506573469943,
132.357550177074));
#52418=CARTESIAN_POINT('',(-7.911,-1.35114142096882E-12,134.357668491763));
#52419=CARTESIAN_POINT('Ctrl Pts',(-7.91099990902224,-0.00116857302219743,
132.357715510959));
#52420=CARTESIAN_POINT('Ctrl Pts',(-7.91065715600478,-2.20244882135127,
132.446287273627));
#52421=CARTESIAN_POINT('Ctrl Pts',(-6.94185703501063,-4.38636564778651,
132.534859036294));
#52422=CARTESIAN_POINT('Ctrl Pts',(-3.67820201488134,-7.34180684107709,
132.712018234694));
#52423=CARTESIAN_POINT('Ctrl Pts',(-1.40868175871573,-8.08992666571367,
132.800605670427));
#52424=CARTESIAN_POINT('Ctrl Pts',(2.97309270521441,-7.65454228025193,132.977780541892));
#52425=CARTESIAN_POINT('Ctrl Pts',(5.05102072675747,-6.47444880834114,133.066367977625));
#52426=CARTESIAN_POINT('Ctrl Pts',(7.6695151884794,-2.93425195367532,133.24354284909));
#52427=CARTESIAN_POINT('Ctrl Pts',(8.18956872247086,-0.601881960097262,
133.332130284823));
#52428=CARTESIAN_POINT('Ctrl Pts',(7.32306689761255,3.71537198232625,133.509305156289));
#52429=CARTESIAN_POINT('Ctrl Pts',(5.94329958850064,5.66643518936656,133.597892592021));
#52430=CARTESIAN_POINT('Ctrl Pts',(2.1615450163765,7.92205913233052,133.775067463487));
#52431=CARTESIAN_POINT('Ctrl Pts',(-0.210816529302454,8.20894963712998,
133.863654899219));
#52432=CARTESIAN_POINT('Ctrl Pts',(-4.42123908576618,6.91982244717717,134.040829770685));
#52433=CARTESIAN_POINT('Ctrl Pts',(-6.2263162563433,5.35390358803356,134.129417206418));
#52434=CARTESIAN_POINT('Ctrl Pts',(-7.6531728085954,2.31334857514337,134.264559258688));
#52435=CARTESIAN_POINT('Ctrl Pts',(-7.9110000000002,1.15702837836358,134.311113875226));
#52436=CARTESIAN_POINT('Ctrl Pts',(-7.911,-1.35114142096882E-12,134.357668491763));
#52437=CARTESIAN_POINT('',(-7.911,-1.18072218668885E-12,136.357668491763));
#52438=CARTESIAN_POINT('Ctrl Pts',(-7.911,-1.35114142096882E-12,134.357668491763));
#52439=CARTESIAN_POINT('Ctrl Pts',(-7.91099999999962,-2.20167589666815,
134.446255927496));
#52440=CARTESIAN_POINT('Ctrl Pts',(-6.94214576672294,-4.38610418338807,
134.534843363229));
#52441=CARTESIAN_POINT('Ctrl Pts',(-3.6782020148815,-7.34180684107701,134.712018234694));
#52442=CARTESIAN_POINT('Ctrl Pts',(-1.4086817587159,-8.08992666571364,134.800605670427));
#52443=CARTESIAN_POINT('Ctrl Pts',(2.97309270521425,-7.65454228025199,134.977780541892));
#52444=CARTESIAN_POINT('Ctrl Pts',(5.05102072675733,-6.47444880834125,135.066367977625));
#52445=CARTESIAN_POINT('Ctrl Pts',(7.66951518847933,-2.93425195367548,135.24354284909));
#52446=CARTESIAN_POINT('Ctrl Pts',(8.18956872247085,-0.601881960097438,
135.332130284823));
#52447=CARTESIAN_POINT('Ctrl Pts',(7.32306689761262,3.7153719823261,135.509305156289));
#52448=CARTESIAN_POINT('Ctrl Pts',(5.94329958850076,5.66643518936643,135.597892592021));
#52449=CARTESIAN_POINT('Ctrl Pts',(2.16154501637667,7.92205913233048,135.775067463487));
#52450=CARTESIAN_POINT('Ctrl Pts',(-0.210816529302277,8.20894963712998,
135.863654899219));
#52451=CARTESIAN_POINT('Ctrl Pts',(-4.42123908576603,6.91982244717726,136.040829770685));
#52452=CARTESIAN_POINT('Ctrl Pts',(-6.22631625634319,5.3539035880337,136.129417206418));
#52453=CARTESIAN_POINT('Ctrl Pts',(-7.65317280859534,2.31334857514353,136.264559258688));
#52454=CARTESIAN_POINT('Ctrl Pts',(-7.91100000000017,1.15702837836375,136.311113875225));
#52455=CARTESIAN_POINT('Ctrl Pts',(-7.911,-1.18072218668885E-12,136.357668491763));
#52456=CARTESIAN_POINT('',(-7.91172576763303,-0.00412227042729108,138.357668491763));
#52457=CARTESIAN_POINT('Ctrl Pts',(-7.911,-1.18072218668885E-12,136.357668491763));
#52458=CARTESIAN_POINT('Ctrl Pts',(-7.91099999999967,-2.20167589666783,
136.446255927496));
#52459=CARTESIAN_POINT('Ctrl Pts',(-6.94214576672317,-4.38610418338763,
136.534843363229));
#52460=CARTESIAN_POINT('Ctrl Pts',(-3.67820201488219,-7.34180684107662,
136.712018234694));
#52461=CARTESIAN_POINT('Ctrl Pts',(-1.40868175871685,-8.08992666571343,
136.800605670427));
#52462=CARTESIAN_POINT('Ctrl Pts',(2.97309270521306,-7.65454228025241,136.977780541892));
#52463=CARTESIAN_POINT('Ctrl Pts',(5.05102072675617,-6.4744488083421,137.066367977625));
#52464=CARTESIAN_POINT('Ctrl Pts',(7.66951518847868,-2.93425195367707,137.24354284909));
#52465=CARTESIAN_POINT('Ctrl Pts',(8.18956872247067,-0.601881960099329,
137.332130284823));
#52466=CARTESIAN_POINT('Ctrl Pts',(7.32306689761358,3.71537198232413,137.509305156288));
#52467=CARTESIAN_POINT('Ctrl Pts',(5.94329958850237,5.66643518936469,137.597892592021));
#52468=CARTESIAN_POINT('Ctrl Pts',(2.16154501637922,7.92205913232974,137.775067463487));
#52469=CARTESIAN_POINT('Ctrl Pts',(-0.210816529299444,8.20894963713002,
137.863654899219));
#52470=CARTESIAN_POINT('Ctrl Pts',(-4.42123908576338,6.91982244717891,138.040829770685));
#52471=CARTESIAN_POINT('Ctrl Pts',(-6.226316256341,5.35390358803617,138.129417206417));
#52472=CARTESIAN_POINT('Ctrl Pts',(-7.65317280859482,2.31334857514579,138.264559258688));
#52473=CARTESIAN_POINT('Ctrl Pts',(-7.91100000000015,1.15702837836497,138.311113875225));
#52474=CARTESIAN_POINT('Ctrl Pts',(-7.911,-1.00974784089658E-12,138.357668491763));
#52475=CARTESIAN_POINT('',(-7.91692124670087,0.00260438373366838,140.357668491763));
#52476=CARTESIAN_POINT('Ctrl Pts',(-7.9121326383558,-0.00643324582964995,
138.357668491763));
#52477=CARTESIAN_POINT('Ctrl Pts',(-7.91784775911465,-0.610979849499266,
138.382007106964));
#52478=CARTESIAN_POINT('Ctrl Pts',(-7.57810911672367,-3.84456081973681,
138.512422874915));
#52479=CARTESIAN_POINT('Ctrl Pts',(-3.12943036986337,-8.82205618148566,
138.748915795611));
#52480=CARTESIAN_POINT('Ctrl Pts',(4.23830707040841,-7.63046510228338,139.014108677485));
#52481=CARTESIAN_POINT('Ctrl Pts',(7.53328766571923,-3.29951305733849,139.226262982982));
#52482=CARTESIAN_POINT('Ctrl Pts',(8.48220415360649,2.05899421969992,139.438417288479));
#52483=CARTESIAN_POINT('Ctrl Pts',(4.36206927714242,8.28217129323548,139.703610170354));
#52484=CARTESIAN_POINT('Ctrl Pts',(-4.61994212435092,8.14028744154645,140.021841628598));
#52485=CARTESIAN_POINT('Ctrl Pts',(-7.85289975606266,2.91743073677501,140.239861069069));
#52486=CARTESIAN_POINT('Ctrl Pts',(-7.92258005546765,0.147753258561319,
140.351803356791));
#52487=CARTESIAN_POINT('Ctrl Pts',(-7.92196407697051,0.00260604264433853,
140.357668491763));
#52488=CARTESIAN_POINT('',(-7.91099906863223,0.00271441514469461,142.357668491763));
#52489=CARTESIAN_POINT('Ctrl Pts',(-7.91099957194591,0.00260243571461738,
140.357668491763));
#52490=CARTESIAN_POINT('Ctrl Pts',(-7.91106335204651,-0.191279144422676,
140.365513763889));
#52491=CARTESIAN_POINT('Ctrl Pts',(-7.90399549224218,-0.385438385360763,
140.373359036015));
#52492=CARTESIAN_POINT('Ctrl Pts',(-7.88976095331893,-0.579303978481056,
140.381204308142));
#52493=CARTESIAN_POINT('Ctrl Pts',(-7.87554147399741,-0.772964469164422,
140.389041280268));
#52494=CARTESIAN_POINT('Ctrl Pts',(-7.85417043973893,-0.966331583624417,
140.396878252394));
#52495=CARTESIAN_POINT('Ctrl Pts',(-7.82566477298294,-1.15883211074506,
140.40471522452));
#52496=CARTESIAN_POINT('Ctrl Pts',(-7.79718373514862,-1.35116631723747,
140.412545425495));
#52497=CARTESIAN_POINT('Ctrl Pts',(-7.7615803929866,-1.54263508229892,140.420375626471));
#52498=CARTESIAN_POINT('Ctrl Pts',(-7.71892361913266,-1.7326682204034,140.428205827446));
#52499=CARTESIAN_POINT('Ctrl Pts',(-7.6762954307552,-1.92257401207944,140.436030781188));
#52500=CARTESIAN_POINT('Ctrl Pts',(-7.6266233024895,-2.1110457517298,140.44385573493));
#52501=CARTESIAN_POINT('Ctrl Pts',(-7.57002756976397,-2.29752118445368,
140.451680688673));
#52502=CARTESIAN_POINT('Ctrl Pts',(-7.51345879436308,-2.48390779636834,
140.459501915282));
#52503=CARTESIAN_POINT('Ctrl Pts',(-7.44997308640442,-2.66829966033515,
140.467323141892));
#52504=CARTESIAN_POINT('Ctrl Pts',(-7.37974128529881,-2.85014728778291,
140.475144368501));
#52505=CARTESIAN_POINT('Ctrl Pts',(-7.30951976620366,-3.0319682925444,140.482964450074));
#52506=CARTESIAN_POINT('Ctrl Pts',(-7.23255424131079,-3.21124547284067,
140.490784531648));
#52507=CARTESIAN_POINT('Ctrl Pts',(-7.14906472596667,-3.38744661123082,
140.498604613221));
#52508=CARTESIAN_POINT('Ctrl Pts',(-7.0655789087473,-3.56363994488298,140.506424348409));
#52509=CARTESIAN_POINT('Ctrl Pts',(-6.97556982626458,-3.73675719005832,
140.514244083596));
#52510=CARTESIAN_POINT('Ctrl Pts',(-6.87930476865276,-3.90628812301288,
140.522063818783));
#52511=CARTESIAN_POINT('Ctrl Pts',(-6.78302707565235,-4.07584130795863,
140.529884580359));
#52512=CARTESIAN_POINT('Ctrl Pts',(-6.68049194516839,-4.24180693729539,
140.537705341935));
#52513=CARTESIAN_POINT('Ctrl Pts',(-6.57201163539827,-4.40370117789455,
140.545526103511));
#52514=CARTESIAN_POINT('Ctrl Pts',(-6.46349804212243,-4.56564509025344,
140.553349264622));
#52515=CARTESIAN_POINT('Ctrl Pts',(-6.349035831643,-4.7235148338636,140.561172425734));
#52516=CARTESIAN_POINT('Ctrl Pts',(-6.22897950457071,-4.87685711618026,
140.568995586845));
#52517=CARTESIAN_POINT('Ctrl Pts',(-6.10880037454934,-5.03035624890994,
140.576826750095));
#52518=CARTESIAN_POINT('Ctrl Pts',(-5.98301591407282,-5.17931839233316,
140.584657913344));
#52519=CARTESIAN_POINT('Ctrl Pts',(-5.8520203963911,-5.32332398790666,140.592489076593));
#52520=CARTESIAN_POINT('Ctrl Pts',(-5.72095393456939,-5.46740757357718,
140.600324481019));
#52521=CARTESIAN_POINT('Ctrl Pts',(-5.58467103587247,-5.60652901054929,
140.608159885445));
#52522=CARTESIAN_POINT('Ctrl Pts',(-5.44360154106573,-5.74030689616042,
140.615995289871));
#52523=CARTESIAN_POINT('Ctrl Pts',(-5.30233550066011,-5.87427116830877,
140.623841611003));
#52524=CARTESIAN_POINT('Ctrl Pts',(-5.15626980297759,-6.00287678243778,
140.631687932136));
#52525=CARTESIAN_POINT('Ctrl Pts',(-5.00586695910596,-6.12578296936247,
140.639534253268));
#52526=CARTESIAN_POINT('Ctrl Pts',(-4.88593367134506,-6.22379004625401,
140.64579101721));
#52527=CARTESIAN_POINT('Ctrl Pts',(-4.76324318593414,-6.3181738247826,140.652047781151));
#52528=CARTESIAN_POINT('Ctrl Pts',(-4.63804215597438,-6.40878194038497,
140.658304545093));
#52529=CARTESIAN_POINT('Ctrl Pts',(-4.48118321702758,-6.52230091764837,
140.666143373203));
#52530=CARTESIAN_POINT('Ctrl Pts',(-4.31991715194024,-6.63022905894237,
140.673982201313));
#52531=CARTESIAN_POINT('Ctrl Pts',(-4.15468305701145,-6.73220095479792,
140.681821029424));
#52532=CARTESIAN_POINT('Ctrl Pts',(-3.98963418694379,-6.83405854173763,
140.689651070329));
#52533=CARTESIAN_POINT('Ctrl Pts',(-3.8206264402778,-6.92997299544976,140.697481111235));
#52534=CARTESIAN_POINT('Ctrl Pts',(-3.64813123004012,-7.01961961422455,
140.70531115214));
#52535=CARTESIAN_POINT('Ctrl Pts',(-3.47579581194466,-7.1091831882282,140.713133939633));
#52536=CARTESIAN_POINT('Ctrl Pts',(-3.29997967376778,-7.1924903291321,140.720956727125));
#52537=CARTESIAN_POINT('Ctrl Pts',(-3.12118256666135,-7.26925996134196,
140.728779514618));
#52538=CARTESIAN_POINT('Ctrl Pts',(-2.94251630938244,-7.34597341091388,
140.736596577127));
#52539=CARTESIAN_POINT('Ctrl Pts',(-2.76087374996427,-7.41615874276132,
140.744413639637));
#52540=CARTESIAN_POINT('Ctrl Pts',(-2.57677873425341,-7.47958102801884,
140.752230702146));
#52541=CARTESIAN_POINT('Ctrl Pts',(-2.39278264801264,-7.54296923123972,
140.760043563902));
#52542=CARTESIAN_POINT('Ctrl Pts',(-2.2063370624747,-7.59960151328478,140.767856425658));
#52543=CARTESIAN_POINT('Ctrl Pts',(-2.01798545004014,-7.64929119091608,
140.775669287413));
#52544=CARTESIAN_POINT('Ctrl Pts',(-1.82969843827413,-7.69896382602592,
140.783479469521));
#52545=CARTESIAN_POINT('Ctrl Pts',(-1.63950704182425,-7.74169851144335,
140.791289651628));
#52546=CARTESIAN_POINT('Ctrl Pts',(-1.44796970902329,-7.77735846684149,
140.799099833735));
#52547=CARTESIAN_POINT('Ctrl Pts',(-1.2564237377643,-7.81302003052676,140.806910368087));
#52548=CARTESIAN_POINT('Ctrl Pts',(-1.06353205301641,-7.84160615324437,
140.814720902438));
#52549=CARTESIAN_POINT('Ctrl Pts',(-0.869863621148918,-7.86303111278352,
140.82253143679));
#52550=CARTESIAN_POINT('Ctrl Pts',(-0.676179666574861,-7.88445778955329,
140.830342597163));
#52551=CARTESIAN_POINT('Ctrl Pts',(-0.481719190672601,-7.89872212023501,
140.838153757536));
#52552=CARTESIAN_POINT('Ctrl Pts',(-0.287056526486923,-7.90579025465521,
140.845964917909));
#52553=CARTESIAN_POINT('Ctrl Pts',(-0.0923439759677483,-7.91286020043103,
140.853778080054));
#52554=CARTESIAN_POINT('Ctrl Pts',(0.102570514381587,-7.91273026330336,
140.861591242198));
#52555=CARTESIAN_POINT('Ctrl Pts',(0.297112211024626,-7.90541873236706,
140.869404404343));
#52556=CARTESIAN_POINT('Ctrl Pts',(0.49173802866483,-7.89810403988091,140.877220944946));
#52557=CARTESIAN_POINT('Ctrl Pts',(0.685990380209172,-7.88360158077329,
140.885037485549));
#52558=CARTESIAN_POINT('Ctrl Pts',(0.879299099446526,-7.86198156279398,
140.892854026152));
#52559=CARTESIAN_POINT('Ctrl Pts',(1.07283341347798,-7.84033631386015,140.900679688799));
#52560=CARTESIAN_POINT('Ctrl Pts',(1.26542154598018,-7.81155695501726,140.908505351447));
#52561=CARTESIAN_POINT('Ctrl Pts',(1.45650188338359,-7.77576512400549,140.916331014095));
#52562=CARTESIAN_POINT('Ctrl Pts',(1.64770677308509,-7.73994996272925,140.924161777761));
#52563=CARTESIAN_POINT('Ctrl Pts',(1.83740156712912,-7.69711329745667,140.931992541428));
#52564=CARTESIAN_POINT('Ctrl Pts',(2.02503921798722,-7.64742683296896,140.939823305094));
#52565=CARTESIAN_POINT('Ctrl Pts',(2.21294798552638,-7.5976685767631,140.94766538339));
#52566=CARTESIAN_POINT('Ctrl Pts',(2.39879333790389,-7.5410408554811,140.955507461686));
#52567=CARTESIAN_POINT('Ctrl Pts',(2.58204650177999,-7.47776416201031,140.963349539983));
#52568=CARTESIAN_POINT('Ctrl Pts',(2.68475996791432,-7.44229755191511,140.967745027769));
#52569=CARTESIAN_POINT('Ctrl Pts',(2.78665946903391,-7.40474294752419,140.972140515554));
#52570=CARTESIAN_POINT('Ctrl Pts',(2.8876552895524,-7.36514547912803,140.97653600334));
#52571=CARTESIAN_POINT('Ctrl Pts',(3.0695545179995,-7.29382818190976,140.984452527339));
#52572=CARTESIAN_POINT('Ctrl Pts',(3.24906693009082,-7.21566758276959,140.992369051337));
#52573=CARTESIAN_POINT('Ctrl Pts',(3.42564045981255,-7.13084205687486,141.000285575336));
#52574=CARTESIAN_POINT('Ctrl Pts',(3.60201056607367,-7.04611425515234,141.008192979016));
#52575=CARTESIAN_POINT('Ctrl Pts',(3.77544822629118,-6.95473696833451,141.016100382697));
#52576=CARTESIAN_POINT('Ctrl Pts',(3.94541851420322,-6.8569376362763,141.024007786378));
#52577=CARTESIAN_POINT('Ctrl Pts',(4.11522448234757,-6.75923285229307,141.03190754553));
#52578=CARTESIAN_POINT('Ctrl Pts',(4.28156945919491,-6.65511856144155,141.039807304682));
#52579=CARTESIAN_POINT('Ctrl Pts',(4.44394016445202,-6.54486950326515,141.047707063834));
#52580=CARTESIAN_POINT('Ctrl Pts',(4.60618397440471,-6.43470660649191,141.055600649197));
#52581=CARTESIAN_POINT('Ctrl Pts',(4.76445941704984,-6.31841868697704,141.063494234561));
#52582=CARTESIAN_POINT('Ctrl Pts',(4.91827917727038,-6.19632559945236,141.071387819925));
#52583=CARTESIAN_POINT('Ctrl Pts',(5.07200721117977,-6.07430531888381,141.07927669816));
#52584=CARTESIAN_POINT('Ctrl Pts',(5.22128458791495,-5.94648698177163,141.087165576395));
#52585=CARTESIAN_POINT('Ctrl Pts',(5.36565405063375,-5.81323297390683,141.095054454629));
#52586=CARTESIAN_POINT('Ctrl Pts',(5.50996415367775,-5.68003375543047,141.102940089233));
#52587=CARTESIAN_POINT('Ctrl Pts',(5.64937011160394,-5.54140355372392,141.110825723837));
#52588=CARTESIAN_POINT('Ctrl Pts',(5.78344855584883,-5.39774432535018,141.118711358441));
#52589=CARTESIAN_POINT('Ctrl Pts',(5.91751507293542,-5.25409787640842,141.126596291566));
#52590=CARTESIAN_POINT('Ctrl Pts',(6.04625478081094,-5.10542353949511,141.134481224691));
#52591=CARTESIAN_POINT('Ctrl Pts',(6.16928157546607,-4.95215971497436,141.142366157815));
#52592=CARTESIAN_POINT('Ctrl Pts',(6.29230794357874,-4.79889642182996,141.150251063603));
#52593=CARTESIAN_POINT('Ctrl Pts',(6.40962122170412,-4.64104394125102,141.15813596939));
#52594=CARTESIAN_POINT('Ctrl Pts',(6.5208759140238,-4.47907337670464,141.166020875177));
#52595=CARTESIAN_POINT('Ctrl Pts',(6.63214888650748,-4.31707619891236,141.173907076527));
#52596=CARTESIAN_POINT('Ctrl Pts',(6.73736109447993,-4.15095987304952,141.181793277876));
#52597=CARTESIAN_POINT('Ctrl Pts',(6.83621052363777,-3.98122426855159,141.189679479225));
#52598=CARTESIAN_POINT('Ctrl Pts',(6.9350927793172,-3.81143229721845,141.197568299473));
#52599=CARTESIAN_POINT('Ctrl Pts',(7.02760787274722,-3.63801895014476,141.20545711972));
#52600=CARTESIAN_POINT('Ctrl Pts',(7.11349975321371,-3.46150866834513,141.213345939967));
#52601=CARTESIAN_POINT('Ctrl Pts',(7.19947476909308,-3.28482754088378,141.221242395864));
#52602=CARTESIAN_POINT('Ctrl Pts',(7.2788136162776,-3.10504380136803,141.229138851762));
#52603=CARTESIAN_POINT('Ctrl Pts',(7.35130799479212,-2.92270281857486,141.237035307659));
#52604=CARTESIAN_POINT('Ctrl Pts',(7.42384244102232,-2.74026105573773,141.244936127935));
#52605=CARTESIAN_POINT('Ctrl Pts',(7.48952476102888,-2.55525955570648,141.252836948211));
#52606=CARTESIAN_POINT('Ctrl Pts',(7.54819646556174,-2.36825908998178,141.260737768488));
#52607=CARTESIAN_POINT('Ctrl Pts',(7.60693946416074,-2.1810313933682,141.268648189331));
#52608=CARTESIAN_POINT('Ctrl Pts',(7.65865474031047,-1.99180021074833,141.276558610173));
#52609=CARTESIAN_POINT('Ctrl Pts',(7.70323461524538,-1.8011378244003,141.284469031016));
#52610=CARTESIAN_POINT('Ctrl Pts',(7.72258052009646,-1.71839787974242,141.287901841206));
#52611=CARTESIAN_POINT('Ctrl Pts',(7.74058333313737,-1.63538849833788,141.291334651397));
#52612=CARTESIAN_POINT('Ctrl Pts',(7.75723729255867,-1.55215675333939,141.294767461587));
#52613=CARTESIAN_POINT('Ctrl Pts',(7.79757488539591,-1.35056095525013,141.303082078924));
#52614=CARTESIAN_POINT('Ctrl Pts',(7.83008429766918,-1.14721849981829,141.311396696262));
#52615=CARTESIAN_POINT('Ctrl Pts',(7.85462553585582,-0.942750598770242,
141.319711313599));
#52616=CARTESIAN_POINT('Ctrl Pts',(7.87913644230235,-0.738535409797657,
141.328015654487));
#52617=CARTESIAN_POINT('Ctrl Pts',(7.89569878168113,-0.533197839257424,
141.336319995374));
#52618=CARTESIAN_POINT('Ctrl Pts',(7.90422358889733,-0.327368991688265,
141.344624336261));
#52619=CARTESIAN_POINT('Ctrl Pts',(7.91273842339619,-0.12178093231108,141.352918962343));
#52620=CARTESIAN_POINT('Ctrl Pts',(7.91323446755868,0.0842969658480649,
141.361213588425));
#52621=CARTESIAN_POINT('Ctrl Pts',(7.90567446500996,0.290227933337863,141.369508214507));
#52622=CARTESIAN_POINT('Ctrl Pts',(7.89812584551826,0.495848831627049,141.377790351412));
#52623=CARTESIAN_POINT('Ctrl Pts',(7.88254539712639,0.701322948546397,141.386072488318));
#52624=CARTESIAN_POINT('Ctrl Pts',(7.85894787110344,0.906012891342435,141.394354625224));
#52625=CARTESIAN_POINT('Ctrl Pts',(7.83537210660609,1.11051407005261,141.402629124383));
#52626=CARTESIAN_POINT('Ctrl Pts',(7.80379404133808,1.3142322264089,141.410903623542));
#52627=CARTESIAN_POINT('Ctrl Pts',(7.7642803768472,1.51653263390719,141.419178122701));
#52628=CARTESIAN_POINT('Ctrl Pts',(7.72481215932269,1.71860036392706,141.427443104876));
#52629=CARTESIAN_POINT('Ctrl Pts',(7.67742661142091,1.91925331177573,141.435708087052));
#52630=CARTESIAN_POINT('Ctrl Pts',(7.62224193218953,2.11786423719078,141.443973069227));
#52631=CARTESIAN_POINT('Ctrl Pts',(7.60018554765108,2.19724567068834,141.447276443055));
#52632=CARTESIAN_POINT('Ctrl Pts',(7.57688385529471,2.27630098160028,141.450579816883));
#52633=CARTESIAN_POINT('Ctrl Pts',(7.55234669838382,2.3549905196011,141.45388319071));
#52634=CARTESIAN_POINT('Ctrl Pts',(7.49094694600511,2.55189671234343,141.462149280208));
#52635=CARTESIAN_POINT('Ctrl Pts',(7.42187718430449,2.74628883910267,141.470415369705));
#52636=CARTESIAN_POINT('Ctrl Pts',(7.34537794916531,2.93757447291402,141.478681459203));
#52637=CARTESIAN_POINT('Ctrl Pts',(7.2688099181583,3.12903213016004,141.486954982406));
#52638=CARTESIAN_POINT('Ctrl Pts',(7.18479918430057,3.3173774445395,141.495228505609));
#52639=CARTESIAN_POINT('Ctrl Pts',(7.09363354844675,3.50203998839974,141.503502028812));
#52640=CARTESIAN_POINT('Ctrl Pts',(7.00237999746393,3.6868806106687,141.511783530547));
#52641=CARTESIAN_POINT('Ctrl Pts',(6.90395789939115,3.86803110907492,141.520065032281));
#52642=CARTESIAN_POINT('Ctrl Pts',(6.79870031680055,4.0449468479,141.528346534015));
#52643=CARTESIAN_POINT('Ctrl Pts',(6.69326748260403,4.22215714761635,141.536641824271));
#52644=CARTESIAN_POINT('Ctrl Pts',(6.58097656085844,4.39511833855824,141.544937114527));
#52645=CARTESIAN_POINT('Ctrl Pts',(6.46220429556927,4.56331421691802,141.553232404783));
#52646=CARTESIAN_POINT('Ctrl Pts',(6.3433243150223,4.73166263309758,141.561535218087));
#52647=CARTESIAN_POINT('Ctrl Pts',(6.21795143252452,4.89523687451447,141.56983803139));
#52648=CARTESIAN_POINT('Ctrl Pts',(6.08650260589297,5.05355390081654,141.578140844693));
#52649=CARTESIAN_POINT('Ctrl Pts',(5.95485219994399,5.21211370933978,141.58645639052));
#52650=CARTESIAN_POINT('Ctrl Pts',(5.81710741786874,5.36539996611454,141.594771936348));
#52651=CARTESIAN_POINT('Ctrl Pts',(5.67372327611372,5.51296518999399,141.603087482176));
#52652=CARTESIAN_POINT('Ctrl Pts',(5.6167559600581,5.57159367320464,141.606391294729));
#52653=CARTESIAN_POINT('Ctrl Pts',(5.5588988433002,5.62931951606852,141.609695107281));
#52654=CARTESIAN_POINT('Ctrl Pts',(5.50018192174204,5.68611640997105,141.612998919833));
#52655=CARTESIAN_POINT('Ctrl Pts',(5.35960693167085,5.82209463540498,141.620908622938));
#52656=CARTESIAN_POINT('Ctrl Pts',(5.21380823078182,5.9530290277964,141.628818326043));
#52657=CARTESIAN_POINT('Ctrl Pts',(5.06318249909811,6.0784952069428,141.636728029148));
#52658=CARTESIAN_POINT('Ctrl Pts',(4.91270958456158,6.20383409453449,141.644629707473));
#52659=CARTESIAN_POINT('Ctrl Pts',(4.75741965684749,6.32371560087875,141.652531385799));
#52660=CARTESIAN_POINT('Ctrl Pts',(4.59774645335204,6.43775182425424,141.660433064124));
#52661=CARTESIAN_POINT('Ctrl Pts',(4.43820566629358,6.55169347778295,141.668328189615));
#52662=CARTESIAN_POINT('Ctrl Pts',(4.2742891239056,6.65979930613653,141.676223315106));
#52663=CARTESIAN_POINT('Ctrl Pts',(4.10646409668552,6.76172120266969,141.684118440597));
#52664=CARTESIAN_POINT('Ctrl Pts',(3.93874716471385,6.86357745182648,141.692008480877));
#52665=CARTESIAN_POINT('Ctrl Pts',(3.7671270571935,6.95925752679173,141.699898521158));
#52666=CARTESIAN_POINT('Ctrl Pts',(3.59210075453213,7.04845608408606,141.707788561438));
#52667=CARTESIAN_POINT('Ctrl Pts',(3.41715477667467,7.13761370549523,141.715674980744));
#52668=CARTESIAN_POINT('Ctrl Pts',(3.23880602511844,7.22029558053709,141.723561400049));
#52669=CARTESIAN_POINT('Ctrl Pts',(3.05757710271658,7.29624172166351,141.731447819354));
#52670=CARTESIAN_POINT('Ctrl Pts',(2.87639779930157,7.37216706936177,141.739332079422));
#52671=CARTESIAN_POINT('Ctrl Pts',(2.69234021429555,7.44136022585706,141.747216339491));
#52672=CARTESIAN_POINT('Ctrl Pts',(2.50594825825776,7.50360875358883,141.755100599559));
#52673=CARTESIAN_POINT('Ctrl Pts',(2.319534541058,7.56586454880319,141.762985780111));
#52674=CARTESIAN_POINT('Ctrl Pts',(2.13078623299568,7.62117397950423,141.770870960663));
#52675=CARTESIAN_POINT('Ctrl Pts',(1.94026439643537,7.66937383832118,141.778756141215));
#52676=CARTESIAN_POINT('Ctrl Pts',(1.74971879617863,7.71757970908317,141.786642305281));
#52677=CARTESIAN_POINT('Ctrl Pts',(1.55739956075781,7.75867415568526,141.794528469347));
#52678=CARTESIAN_POINT('Ctrl Pts',(1.36387996441368,7.79254467055986,141.802414633414));
#52679=CARTESIAN_POINT('Ctrl Pts',(1.17030376123954,7.82642509297104,141.810303104279));
#52680=CARTESIAN_POINT('Ctrl Pts',(0.975526836956832,7.85307731329363,141.818191575144));
#52681=CARTESIAN_POINT('Ctrl Pts',(0.780129887603958,7.87244043219554,141.826080046009));
#52682=CARTESIAN_POINT('Ctrl Pts',(0.584642997325844,7.89181246391229,141.833972147926));
#52683=CARTESIAN_POINT('Ctrl Pts',(0.38853585590506,7.903888674302,141.841864249842));
#52684=CARTESIAN_POINT('Ctrl Pts',(0.192391726586302,7.90866021672073,141.849756351759));
#52685=CARTESIAN_POINT('Ctrl Pts',(-0.00397979295669995,7.91343729079674,
141.857657603003));
#52686=CARTESIAN_POINT('Ctrl Pts',(-0.200388041431948,7.91089277349285,
141.865558854246));
#52687=CARTESIAN_POINT('Ctrl Pts',(-0.396251137986991,7.90106992980343,
141.87346010549));
#52688=CARTESIAN_POINT('Ctrl Pts',(-0.592244019158217,7.8912405772105,141.881366592334));
#52689=CARTESIAN_POINT('Ctrl Pts',(-0.787690686038262,7.87412331358912,
141.889273079178));
#52690=CARTESIAN_POINT('Ctrl Pts',(-0.982016658540009,7.84981300938754,
141.897179566022));
#52691=CARTESIAN_POINT('Ctrl Pts',(-1.1766103473169,7.82546921370768,141.905096945364));
#52692=CARTESIAN_POINT('Ctrl Pts',(-1.37007991889728,7.79391263904577,141.913014324705));
#52693=CARTESIAN_POINT('Ctrl Pts',(-1.56186215083803,7.75528900955855,141.920931704047));
#52694=CARTESIAN_POINT('Ctrl Pts',(-1.64501688368922,7.73854221524266,141.924364595391));
#52695=CARTESIAN_POINT('Ctrl Pts',(-1.72785460013434,7.72046744935075,141.927797486736));
#52696=CARTESIAN_POINT('Ctrl Pts',(-1.81033042285988,7.70107945421082,141.93123037808));
#52697=CARTESIAN_POINT('Ctrl Pts',(-1.99872689261025,7.65679217438513,141.93907200474));
#52698=CARTESIAN_POINT('Ctrl Pts',(-2.18579398331701,7.60551766755849,141.946913631401));
#52699=CARTESIAN_POINT('Ctrl Pts',(-2.37096792738509,7.5473460293875,141.954755258061));
#52700=CARTESIAN_POINT('Ctrl Pts',(-2.55592384308579,7.48924288393756,141.962587651797));
#52701=CARTESIAN_POINT('Ctrl Pts',(-2.73899071879854,7.42425888124231,141.970420045533));
#52702=CARTESIAN_POINT('Ctrl Pts',(-2.91961411751259,7.35253523655761,141.978252439268));
#52703=CARTESIAN_POINT('Ctrl Pts',(-3.10006000737474,7.28088207876393,141.986077135667));
#52704=CARTESIAN_POINT('Ctrl Pts',(-3.27806687800664,7.20250259767271,141.993901832065));
#52705=CARTESIAN_POINT('Ctrl Pts',(-3.45309443990792,7.11758805980488,142.001726528464));
#52706=CARTESIAN_POINT('Ctrl Pts',(-3.6279840440632,7.03274045207147,142.009545057391));
#52707=CARTESIAN_POINT('Ctrl Pts',(-3.79989870173604,6.94136819931556,142.017363586318));
#52708=CARTESIAN_POINT('Ctrl Pts',(-3.96831696336821,6.84371108962412,142.025182115245));
#52709=CARTESIAN_POINT('Ctrl Pts',(-4.13663522913849,6.74611196240298,142.032996002036));
#52710=CARTESIAN_POINT('Ctrl Pts',(-4.30146093070975,6.64223558726326,142.040809888827));
#52711=CARTESIAN_POINT('Ctrl Pts',(-4.46229598191233,6.53236829716521,142.048623775617));
#52712=CARTESIAN_POINT('Ctrl Pts',(-4.62306680863312,6.42254487915673,142.056434542175));
#52713=CARTESIAN_POINT('Ctrl Pts',(-4.77984986989528,6.30673551059833,142.064245308733));
#52714=CARTESIAN_POINT('Ctrl Pts',(-4.93217475456442,6.1852706642828,142.072056075291));
#52715=CARTESIAN_POINT('Ctrl Pts',(-5.08449358505963,6.06381064560464,142.079866531408));
#52716=CARTESIAN_POINT('Ctrl Pts',(-5.23235431136309,5.93669580913485,142.087676987526));
#52717=CARTESIAN_POINT('Ctrl Pts',(-5.3753180418017,5.8042981444341,142.095487443644));
#52718=CARTESIAN_POINT('Ctrl Pts',(-5.51828571490337,5.67189682846195,142.103298115159));
#52719=CARTESIAN_POINT('Ctrl Pts',(-5.65635586432456,5.53421263261948,142.111108786674));
#52720=CARTESIAN_POINT('Ctrl Pts',(-5.7891250794199,5.39165575819076,142.118919458189));
#52721=CARTESIAN_POINT('Ctrl Pts',(-5.92192133858203,5.2490698460244,142.126731720678));
#52722=CARTESIAN_POINT('Ctrl Pts',(-6.04941427261299,5.10160953561801,142.134543983166));
#52723=CARTESIAN_POINT('Ctrl Pts',(-6.17123942677439,4.94971968271187,142.142356245655));
#52724=CARTESIAN_POINT('Ctrl Pts',(-6.2931108524963,4.79777213908851,142.150171475393));
#52725=CARTESIAN_POINT('Ctrl Pts',(-6.40930999025035,4.64139197595457,142.157986705131));
#52726=CARTESIAN_POINT('Ctrl Pts',(-6.51951445051296,4.48105482331479,142.165801934868));
#52727=CARTESIAN_POINT('Ctrl Pts',(-6.62983876347712,4.32054329623628,142.173625664048));
#52728=CARTESIAN_POINT('Ctrl Pts',(-6.73415517823525,4.15606647454006,142.181449393227));
#52729=CARTESIAN_POINT('Ctrl Pts',(-6.83218565361493,3.98812740450181,142.189273122407));
#52730=CARTESIAN_POINT('Ctrl Pts',(-6.930275606398,3.82008644186562,142.197101598428));
#52731=CARTESIAN_POINT('Ctrl Pts',(-7.02207185368854,3.6485793538073,142.204930074448));
#52732=CARTESIAN_POINT('Ctrl Pts',(-7.10734360929572,3.47413123232317,142.212758550469));
#52733=CARTESIAN_POINT('Ctrl Pts',(-7.19273272273763,3.29944302133152,142.220597800667));
#52734=CARTESIAN_POINT('Ctrl Pts',(-7.2715792669835,3.12180601274751,142.228437050865));
#52735=CARTESIAN_POINT('Ctrl Pts',(-7.34370121033454,2.94176367734239,142.236276301063));
#52736=CARTESIAN_POINT('Ctrl Pts',(-7.38413732362819,2.84082058105531,142.240671479484));
#52737=CARTESIAN_POINT('Ctrl Pts',(-7.4224605075538,2.73912164949256,142.245066657906));
#52738=CARTESIAN_POINT('Ctrl Pts',(-7.45864566386742,2.63676427859446,142.249461836327));
#52739=CARTESIAN_POINT('Ctrl Pts',(-7.53540491871628,2.41963448508658,142.25878528978));
#52740=CARTESIAN_POINT('Ctrl Pts',(-7.60272127187402,2.19903128111711,142.268108743232));
#52741=CARTESIAN_POINT('Ctrl Pts',(-7.66031837808705,1.97571337656599,142.277432196685));
#52742=CARTESIAN_POINT('Ctrl Pts',(-7.71768456206012,1.75329081336332,142.286718269913));
#52743=CARTESIAN_POINT('Ctrl Pts',(-7.76540921234219,1.5281753369818,142.296004343141));
#52744=CARTESIAN_POINT('Ctrl Pts',(-7.80326604226389,1.30113799177921,142.30529041637));
#52745=CARTESIAN_POINT('Ctrl Pts',(-7.840801781141,1.0760263138468,142.314497727721));
#52746=CARTESIAN_POINT('Ctrl Pts',(-7.86863633167718,0.849025309717781,
142.323705039073));
#52747=CARTESIAN_POINT('Ctrl Pts',(-7.88659597041506,0.620906594773285,
142.332912350425));
#52748=CARTESIAN_POINT('Ctrl Pts',(-7.90269228554174,0.416455337393836,
142.341164397538));
#52749=CARTESIAN_POINT('Ctrl Pts',(-7.91085699332149,0.211106556477672,
142.34941644465));
#52750=CARTESIAN_POINT('Ctrl Pts',(-7.91099813726446,0.00542883029005868,
142.357668491763));
#52751=CARTESIAN_POINT('',(-7.90415356074214,-0.00309866779400792,144.357668491763));
#52752=CARTESIAN_POINT('Ctrl Pts',(-7.911,-6.69464483848969E-13,142.357668491763));
#52753=CARTESIAN_POINT('Ctrl Pts',(-7.91099999999981,-2.20167589666747,
142.446255927496));
#52754=CARTESIAN_POINT('Ctrl Pts',(-6.94214576672331,-4.38610418338747,
142.534843363229));
#52755=CARTESIAN_POINT('Ctrl Pts',(-3.67820201488214,-7.34180684107669,
142.712018234694));
#52756=CARTESIAN_POINT('Ctrl Pts',(-1.4086817587166,-8.08992666571352,142.800605670427));
#52757=CARTESIAN_POINT('Ctrl Pts',(2.97309270521359,-7.65454228025225,142.977780541892));
#52758=CARTESIAN_POINT('Ctrl Pts',(5.05102072675677,-6.47444880834168,143.066367977625));
#52759=CARTESIAN_POINT('Ctrl Pts',(7.66951518847908,-2.93425195367614,143.24354284909));
#52760=CARTESIAN_POINT('Ctrl Pts',(8.1895687224708,-0.601881960098144,143.332130284823));
#52761=CARTESIAN_POINT('Ctrl Pts',(7.32306689761295,3.71537198232546,143.509305156288));
#52762=CARTESIAN_POINT('Ctrl Pts',(5.94329958850125,5.66643518936592,143.597892592021));
#52763=CARTESIAN_POINT('Ctrl Pts',(2.16154501637735,7.92205913233029,143.775067463487));
#52764=CARTESIAN_POINT('Ctrl Pts',(-0.210816529301569,8.20894963713,143.863654899219));
#52765=CARTESIAN_POINT('Ctrl Pts',(-4.42123908576543,6.91982244717764,144.040829770685));
#52766=CARTESIAN_POINT('Ctrl Pts',(-6.22631625634273,5.35390358803423,144.129417206418));
#52767=CARTESIAN_POINT('Ctrl Pts',(-7.65317280859508,2.31334857514433,144.264559258688));
#52768=CARTESIAN_POINT('Ctrl Pts',(-7.91100000000001,1.15702837836474,144.311113875225));
#52769=CARTESIAN_POINT('Ctrl Pts',(-7.911,-4.82947015711943E-14,144.357668491763));
#52770=CARTESIAN_POINT('',(-7.91789235578852,-0.0010059796957165,146.357631904486));
#52771=CARTESIAN_POINT('Ctrl Pts',(-7.90105610939419,-0.00450056042370127,
144.357668491763));
#52772=CARTESIAN_POINT('Ctrl Pts',(-7.90689325060477,-0.997333501851549,
144.397473009194));
#52773=CARTESIAN_POINT('Ctrl Pts',(-7.27322451497355,-4.62900481828023,
144.543354679371));
#52774=CARTESIAN_POINT('Ctrl Pts',(-1.82054063441708,-9.17431691246998,
144.795313502303));
#52775=CARTESIAN_POINT('Ctrl Pts',(6.73662521562475,-6.49815555119431,145.113544960548));
#52776=CARTESIAN_POINT('Ctrl Pts',(9.10643661084831,2.16675378454077,145.431776418795));
#52777=CARTESIAN_POINT('Ctrl Pts',(4.10254492915994,7.70430850903412,145.696969300668));
#52778=CARTESIAN_POINT('Ctrl Pts',(-1.32366529678204,8.11696492869233,145.909123606165));
#52779=CARTESIAN_POINT('Ctrl Pts',(-6.11008896738171,6.09778331381346,146.111649179355));
#52780=CARTESIAN_POINT('Ctrl Pts',(-7.9048743251548,2.38505523999662,146.261136176172));
#52781=CARTESIAN_POINT('Ctrl Pts',(-7.92202559494964,-0.000978787874874063,
146.357584596613));
#52782=CARTESIAN_POINT('',(-7.91099987608327,0.00138933783038613,148.357612589845));
#52783=CARTESIAN_POINT('Ctrl Pts',(-7.91099992636282,-0.00105132372223101,
146.357710793261));
#52784=CARTESIAN_POINT('Ctrl Pts',(-7.91069155732802,-2.20237127150424,
146.446284128495));
#52785=CARTESIAN_POINT('Ctrl Pts',(-6.94188600507358,-4.3863394136048,146.534857463728));
#52786=CARTESIAN_POINT('Ctrl Pts',(-3.67820201488245,-7.34180684107653,
146.712018234694));
#52787=CARTESIAN_POINT('Ctrl Pts',(-1.40868175871695,-8.08992666571346,
146.800605670427));
#52788=CARTESIAN_POINT('Ctrl Pts',(2.97309270521326,-7.65454228025238,146.977780541892));
#52789=CARTESIAN_POINT('Ctrl Pts',(5.05102072675649,-6.4744488083419,147.066367977625));
#52790=CARTESIAN_POINT('Ctrl Pts',(7.66951518847895,-2.93425195367647,147.24354284909));
#52791=CARTESIAN_POINT('Ctrl Pts',(8.18956872247077,-0.601881960098497,
147.332130284823));
#52792=CARTESIAN_POINT('Ctrl Pts',(7.32306689761311,3.71537198232515,147.509305156288));
#52793=CARTESIAN_POINT('Ctrl Pts',(5.9432995885015,5.66643518936566,147.597892592021));
#52794=CARTESIAN_POINT('Ctrl Pts',(2.16154501637769,7.9220591323302,147.775067463487));
#52795=CARTESIAN_POINT('Ctrl Pts',(-0.210816529301215,8.20894963713001,
147.863654899219));
#52796=CARTESIAN_POINT('Ctrl Pts',(-4.42123908576514,6.91982244717783,148.040829770685));
#52797=CARTESIAN_POINT('Ctrl Pts',(-6.22631625634249,5.3539035880345,148.129417206418));
#52798=CARTESIAN_POINT('Ctrl Pts',(-7.65297606741948,2.31376782006909,148.264540624715));
#52799=CARTESIAN_POINT('Ctrl Pts',(-7.91079356649125,1.1579540194574,148.311076607279));
#52800=CARTESIAN_POINT('Ctrl Pts',(-7.91099987608327,0.00138933783038613,
148.357612589845));
#52801=CARTESIAN_POINT('',(-7.911,1.33226762955019E-14,150.357668491763));
#52802=CARTESIAN_POINT('Ctrl Pts',(-7.9109998762523,0.00139926271889242,
148.357864421896));
#52803=CARTESIAN_POINT('Ctrl Pts',(-7.91103419945879,-0.192653561413069,
148.365678114097));
#52804=CARTESIAN_POINT('Ctrl Pts',(-7.90392420100454,-0.386895670116855,
148.373491806299));
#52805=CARTESIAN_POINT('Ctrl Pts',(-7.88965428496979,-0.580754908423348,
148.381305498501));
#52806=CARTESIAN_POINT('Ctrl Pts',(-7.87539373648693,-0.774486886942986,
148.389114061368));
#52807=CARTESIAN_POINT('Ctrl Pts',(-7.85398265784157,-0.96783614515552,
148.396922624236));
#52808=CARTESIAN_POINT('Ctrl Pts',(-7.82545752325939,-1.16023081826982,
148.404731187104));
#52809=CARTESIAN_POINT('Ctrl Pts',(-7.79694553304693,-1.3525368360016,148.412536151789));
#52810=CARTESIAN_POINT('Ctrl Pts',(-7.76132606900809,-1.54388879662352,
148.420341116474));
#52811=CARTESIAN_POINT('Ctrl Pts',(-7.71868743478577,-1.73372007085349,
148.428146081159));
#52812=CARTESIAN_POINT('Ctrl Pts',(-7.67605352254792,-1.92353032235738,
148.435950181489));
#52813=CARTESIAN_POINT('Ctrl Pts',(-7.62640205757169,-2.11181987705395,
148.443754281819));
#52814=CARTESIAN_POINT('Ctrl Pts',(-7.56987252230388,-2.29803198325627,
148.451558382149));
#52815=CARTESIAN_POINT('Ctrl Pts',(-7.51334441660939,-2.48423938034751,
148.459362285122));
#52816=CARTESIAN_POINT('Ctrl Pts',(-7.44993868850091,-2.66836909545884,
148.467166188094));
#52817=CARTESIAN_POINT('Ctrl Pts',(-7.37984479689068,-2.84987925600464,
148.474970091067));
#52818=CARTESIAN_POINT('Ctrl Pts',(-7.30974025646079,-3.0314169919771,148.482775179626));
#52819=CARTESIAN_POINT('Ctrl Pts',(-7.23294565545322,-3.21033405121888,
148.490580268184));
#52820=CARTESIAN_POINT('Ctrl Pts',(-7.14969877825737,-3.38610814655779,
148.498385356743));
#52821=CARTESIAN_POINT('Ctrl Pts',(-7.06642450048534,-3.56194009765841,
148.506193014334));
#52822=CARTESIAN_POINT('Ctrl Pts',(-6.97669386727089,-3.73462670542988,
148.514000671925));
#52823=CARTESIAN_POINT('Ctrl Pts',(-6.88079088311935,-3.90366978915758,
148.521808329517));
#52824=CARTESIAN_POINT('Ctrl Pts',(-6.7847833043722,-4.07289723620974,148.529624502367));
#52825=CARTESIAN_POINT('Ctrl Pts',(-6.68259010082437,-4.23847291350021,
148.537440675218));
#52826=CARTESIAN_POINT('Ctrl Pts',(-6.57453954467923,-4.39992622386434,
148.545256848068));
#52827=CARTESIAN_POINT('Ctrl Pts',(-6.46642820732519,-4.56147035585617,
148.553077417717));
#52828=CARTESIAN_POINT('Ctrl Pts',(-6.35245315740072,-4.71888721416122,
148.560897987365));
#52829=CARTESIAN_POINT('Ctrl Pts',(-6.23298335758991,-4.8717388542498,148.568718557013));
#52830=CARTESIAN_POINT('Ctrl Pts',(-6.11333400357754,-5.02482021895698,
148.576550880394));
#52831=CARTESIAN_POINT('Ctrl Pts',(-5.98817362538431,-5.17332238601346,
148.584383203776));
#52832=CARTESIAN_POINT('Ctrl Pts',(-5.85790945201707,-5.31684284627345,
148.592215527157));
#52833=CARTESIAN_POINT('Ctrl Pts',(-5.73663464364711,-5.45045914203059,
148.599507351859));
#52834=CARTESIAN_POINT('Ctrl Pts',(-5.61093668500354,-5.57975779986694,
148.606799176561));
#52835=CARTESIAN_POINT('Ctrl Pts',(-5.48116956406796,-5.70444574081786,
148.614091001264));
#52836=CARTESIAN_POINT('Ctrl Pts',(-5.34161801288141,-5.83853514226644,
148.621932628949));
#52837=CARTESIAN_POINT('Ctrl Pts',(-5.19692320930869,-5.96771174700591,
148.629774256634));
#52838=CARTESIAN_POINT('Ctrl Pts',(-5.04746713421435,-6.09155124159898,
148.637615884319));
#52839=CARTESIAN_POINT('Ctrl Pts',(-4.89818703230537,-6.21524492458603,
148.645448279083));
#52840=CARTESIAN_POINT('Ctrl Pts',(-4.74415708910208,-6.33361378810063,
148.653280673847));
#52841=CARTESIAN_POINT('Ctrl Pts',(-4.58579712909097,-6.44626912956798,
148.661113068611));
#52842=CARTESIAN_POINT('Ctrl Pts',(-4.42759279831991,-6.55881375829469,
148.668937766039));
#52843=CARTESIAN_POINT('Ctrl Pts',(-4.26506720917366,-6.66565584445674,
148.676762463468));
#52844=CARTESIAN_POINT('Ctrl Pts',(-4.09867451543366,-6.76644575952062,
148.684587160897));
#52845=CARTESIAN_POINT('Ctrl Pts',(-3.93241297333208,-6.86715623141787,
148.692405690856));
#52846=CARTESIAN_POINT('Ctrl Pts',(-3.76229069666347,-6.96182385190315,
148.700224220816));
#52847=CARTESIAN_POINT('Ctrl Pts',(-3.58879233452092,-7.05014117445061,
148.708042750775));
#52848=CARTESIAN_POINT('Ctrl Pts',(-3.41539698444037,-7.13840605990649,
148.715856638599));
#52849=CARTESIAN_POINT('Ctrl Pts',(-3.23862985429503,-7.22032799885895,
148.723670526422));
#52850=CARTESIAN_POINT('Ctrl Pts',(-3.05900197109044,-7.29564445000336,
148.731484414246));
#52851=CARTESIAN_POINT('Ctrl Pts',(-2.87944581668535,-7.37093082586921,
148.739295181837));
#52852=CARTESIAN_POINT('Ctrl Pts',(-2.69703150909478,-7.43961683337175,
148.747105949429));
#52853=CARTESIAN_POINT('Ctrl Pts',(-2.5122920913392,-7.50148714907881,148.75491671702));
#52854=CARTESIAN_POINT('Ctrl Pts',(-2.32756001612867,-7.56335500572442,
148.762727174169));
#52855=CARTESIAN_POINT('Ctrl Pts',(-2.14050334543881,-7.61840758997842,
148.770537631317));
#52856=CARTESIAN_POINT('Ctrl Pts',(-1.95167284726542,-7.66647859823837,
148.778348088466));
#52857=CARTESIAN_POINT('Ctrl Pts',(-1.76283714154313,-7.71455093219584,
148.786158761011));
#52858=CARTESIAN_POINT('Ctrl Pts',(-1.57222785179897,-7.75564121901117,
148.793969433556));
#52859=CARTESIAN_POINT('Ctrl Pts',(-1.38040854380454,-7.78963370462254,
148.801780106101));
#52860=CARTESIAN_POINT('Ctrl Pts',(-1.18855016374411,-7.82363311423261,
148.809592369618));
#52861=CARTESIAN_POINT('Ctrl Pts',(-0.99548162096845,-7.85053178116441,
148.817404633135));
#52862=CARTESIAN_POINT('Ctrl Pts',(-0.801774404552212,-7.87026548498873,
148.825216896651));
#52863=CARTESIAN_POINT('Ctrl Pts',(-0.607993614441421,-7.89000668405007,
148.833032127415));
#52864=CARTESIAN_POINT('Ctrl Pts',(-0.413574017275125,-7.9025774635303,
148.840847358178));
#52865=CARTESIAN_POINT('Ctrl Pts',(-0.219090078518901,-7.90796563836077,
148.848662588941));
#52866=CARTESIAN_POINT('Ctrl Pts',(-0.024394629273337,-7.91335967308641,
148.856486319138));
#52867=CARTESIAN_POINT('Ctrl Pts',(0.170364949480691,-7.91155549173148,
148.864310049335));
#52868=CARTESIAN_POINT('Ctrl Pts',(0.364615275489833,-7.90259303652159,
148.872133779532));
#52869=CARTESIAN_POINT('Ctrl Pts',(0.558983457666191,-7.89362514358275,
148.879962256567));
#52870=CARTESIAN_POINT('Ctrl Pts',(0.752841421771199,-7.87749035052994,
148.887790733602));
#52871=CARTESIAN_POINT('Ctrl Pts',(0.945622956665146,-7.85428024861781,
148.895619210637));
#52872=CARTESIAN_POINT('Ctrl Pts',(1.13866981262137,-7.83103820314377,148.903458461835));
#52873=CARTESIAN_POINT('Ctrl Pts',(1.33063693402655,-7.80070145415603,148.911297713034));
#52874=CARTESIAN_POINT('Ctrl Pts',(1.52096917400047,-7.76341250815261,148.919136964233));
#52875=CARTESIAN_POINT('Ctrl Pts',(1.62768110296808,-7.74250603766847,148.923532129325));
#52876=CARTESIAN_POINT('Ctrl Pts',(1.73387939145228,-7.71941510618414,148.927927294418));
#52877=CARTESIAN_POINT('Ctrl Pts',(1.83946864032763,-7.694171568223,148.93232245951));
#52878=CARTESIAN_POINT('Ctrl Pts',(2.02949528431883,-7.64874132932735,148.940232341256));
#52879=CARTESIAN_POINT('Ctrl Pts',(2.21809443601166,-7.59620580985692,148.948142223003));
#52880=CARTESIAN_POINT('Ctrl Pts',(2.40469524067325,-7.53666781804024,148.956052104749));
#52881=CARTESIAN_POINT('Ctrl Pts',(2.59109317887584,-7.47719455403434,148.963953387123));
#52882=CARTESIAN_POINT('Ctrl Pts',(2.77549677173073,-7.41073408516476,148.971854669498));
#52883=CARTESIAN_POINT('Ctrl Pts',(2.95734563337055,-7.33744013977519,148.979755951872));
#52884=CARTESIAN_POINT('Ctrl Pts',(3.13903058666945,-7.26421225742764,148.987650112475));
#52885=CARTESIAN_POINT('Ctrl Pts',(3.31816507795086,-7.1841632964965,148.995544273078));
#52886=CARTESIAN_POINT('Ctrl Pts',(3.49420389537122,-7.09749675150138,149.003438433681));
#52887=CARTESIAN_POINT('Ctrl Pts',(3.67011674338177,-7.01089222313237,149.0113269454));
#52888=CARTESIAN_POINT('Ctrl Pts',(3.84293802269998,-6.91767969689486,149.019215457119));
#52889=CARTESIAN_POINT('Ctrl Pts',(4.01214227058525,-6.81811083809753,149.027103968839));
#52890=CARTESIAN_POINT('Ctrl Pts',(4.18125686511461,-6.71859473614554,149.034988300808));
#52891=CARTESIAN_POINT('Ctrl Pts',(4.34675795045919,-6.61272918715504,149.042872632776));
#52892=CARTESIAN_POINT('Ctrl Pts',(4.50814421646872,-6.50081200493597,149.050756964745));
#52893=CARTESIAN_POINT('Ctrl Pts',(4.66947494000625,-6.38893333997808,149.058638583253));
#52894=CARTESIAN_POINT('Ctrl Pts',(4.8266933834927,-6.27100738904184,149.066520201762));
#52895=CARTESIAN_POINT('Ctrl Pts',(4.97932658136968,-6.1473756836609,149.07440182027));
#52896=CARTESIAN_POINT('Ctrl Pts',(5.13196177866581,-6.02374235876598,149.082283542023));
#52897=CARTESIAN_POINT('Ctrl Pts',(5.28001133691194,-5.89440334054266,149.090165263777));
#52898=CARTESIAN_POINT('Ctrl Pts',(5.4230343537672,-5.75974126136416,149.09804698553));
#52899=CARTESIAN_POINT('Ctrl Pts',(5.56606598655101,-5.62507106993297,149.105929182091));
#52900=CARTESIAN_POINT('Ctrl Pts',(5.70407022283161,-5.48507741474963,149.113811378651));
#52901=CARTESIAN_POINT('Ctrl Pts',(5.83664209074272,-5.34018071834375,149.121693575212));
#52902=CARTESIAN_POINT('Ctrl Pts',(5.9692442529349,-5.19525091128389,149.12957757295));
#52903=CARTESIAN_POINT('Ctrl Pts',(6.09641134020214,-5.04541608503013,149.137461570688));
#52904=CARTESIAN_POINT('Ctrl Pts',(6.21777768138167,-4.89113092289626,149.145345568426));
#52905=CARTESIAN_POINT('Ctrl Pts',(6.33919217889602,-4.7367845427356,149.153232694416));
#52906=CARTESIAN_POINT('Ctrl Pts',(6.45480113091654,-4.57798457913831,149.161119820406));
#52907=CARTESIAN_POINT('Ctrl Pts',(6.56428118224404,-4.41521613971919,149.169006946395));
#52908=CARTESIAN_POINT('Ctrl Pts',(6.67387803675808,-4.25227404425806,149.176902487082));
#52909=CARTESIAN_POINT('Ctrl Pts',(6.77733273705257,-4.08535530243727,149.184798027768));
#52910=CARTESIAN_POINT('Ctrl Pts',(6.87436646860418,-3.91497211424685,149.192693568455));
#52911=CARTESIAN_POINT('Ctrl Pts',(6.97145929053952,-3.74448516824141,149.200593917269));
#52912=CARTESIAN_POINT('Ctrl Pts',(7.0621231892713,-3.57052987500456,149.208494266083));
#52913=CARTESIAN_POINT('Ctrl Pts',(7.14612670179428,-3.39364025228114,149.216394614896));
#52914=CARTESIAN_POINT('Ctrl Pts',(7.23023959088703,-3.21652031085342,149.22430525034));
#52915=CARTESIAN_POINT('Ctrl Pts',(7.30767463577674,-3.03645872443077,149.232215885784));
#52916=CARTESIAN_POINT('Ctrl Pts',(7.37824920807456,-2.85400764251731,149.240126521228));
#52917=CARTESIAN_POINT('Ctrl Pts',(7.40925847635465,-2.77384173625897,149.243602320071));
#52918=CARTESIAN_POINT('Ctrl Pts',(7.43894393371744,-2.69321469837884,149.247078118914));
#52919=CARTESIAN_POINT('Ctrl Pts',(7.4672931863409,-2.61217408861408,149.250553917757));
#52920=CARTESIAN_POINT('Ctrl Pts',(7.53180750577824,-2.42775018667901,149.258463784018));
#52921=CARTESIAN_POINT('Ctrl Pts',(7.58957260064992,-2.24068595604946,149.26637365028));
#52922=CARTESIAN_POINT('Ctrl Pts',(7.64036635717733,-2.05151722588741,149.274283516541));
#52923=CARTESIAN_POINT('Ctrl Pts',(7.69110491135422,-1.86255408316886,149.282184786407));
#52924=CARTESIAN_POINT('Ctrl Pts',(7.73488712950447,-1.67149132670043,149.290086056273));
#52925=CARTESIAN_POINT('Ctrl Pts',(7.77153939559275,-1.47888350546954,149.29798732614));
#52926=CARTESIAN_POINT('Ctrl Pts',(7.80815863908356,-1.28644921813513,149.305881477197));
#52927=CARTESIAN_POINT('Ctrl Pts',(7.83766066325707,-1.09247297585826,149.313775628255));
#52928=CARTESIAN_POINT('Ctrl Pts',(7.85992192259556,-0.897523465265205,
149.321669779313));
#52929=CARTESIAN_POINT('Ctrl Pts',(7.88216726058491,-0.702713383406976,
149.32955828444));
#52930=CARTESIAN_POINT('Ctrl Pts',(7.89718211228078,-0.506931761396544,
149.337446789567));
#52931=CARTESIAN_POINT('Ctrl Pts',(7.90489413375551,-0.31075671210399,149.345335294693));
#52932=CARTESIAN_POINT('Ctrl Pts',(7.91260207186756,-0.114685533616116,
149.353219623013));
#52933=CARTESIAN_POINT('Ctrl Pts',(7.91301487111404,0.0817783131925406,
149.361103951332));
#52934=CARTESIAN_POINT('Ctrl Pts',(7.90611206832419,0.278052087024499,149.368988279652));
#52935=CARTESIAN_POINT('Ctrl Pts',(7.89921163862408,0.474258384601366,149.376869897447));
#52936=CARTESIAN_POINT('Ctrl Pts',(7.88500063145307,0.670274395096636,149.384751515241));
#52937=CARTESIAN_POINT('Ctrl Pts',(7.86351068558139,0.865517589507741,149.392633133036));
#52938=CARTESIAN_POINT('Ctrl Pts',(7.84202044625025,1.06076345009417,149.400514858459));
#52939=CARTESIAN_POINT('Ctrl Pts',(7.81325109885063,1.25523612970774,149.408396583882));
#52940=CARTESIAN_POINT('Ctrl Pts',(7.77728619285518,1.44835785440759,149.416278309306));
#52941=CARTESIAN_POINT('Ctrl Pts',(7.74131910781728,1.64149127997037,149.424160512267));
#52942=CARTESIAN_POINT('Ctrl Pts',(7.6981556580643,1.8332732480634,149.432042715229));
#52943=CARTESIAN_POINT('Ctrl Pts',(7.64793060912958,2.0231357833667,149.43992491819));
#52944=CARTESIAN_POINT('Ctrl Pts',(7.59769406577727,2.21304177028056,149.447808925059));
#52945=CARTESIAN_POINT('Ctrl Pts',(7.54039279115692,2.40102711545622,149.455692931928));
#52946=CARTESIAN_POINT('Ctrl Pts',(7.47621161956474,2.58653838546526,149.463576938796));
#52947=CARTESIAN_POINT('Ctrl Pts',(7.41200495965826,2.77212332769681,149.471464076646));
#52948=CARTESIAN_POINT('Ctrl Pts',(7.34091307133737,2.95523191113743,149.479351214496));
#52949=CARTESIAN_POINT('Ctrl Pts',(7.26316926010277,3.1353298549113,149.487238352346));
#52950=CARTESIAN_POINT('Ctrl Pts',(7.18534246476197,3.31562003606917,149.495133908964));
#52951=CARTESIAN_POINT('Ctrl Pts',(7.1008497010102,3.49289284179275,149.503029465582));
#52952=CARTESIAN_POINT('Ctrl Pts',(7.00997114524581,3.6666368163238,149.5109250222));
#52953=CARTESIAN_POINT('Ctrl Pts',(6.91903722050739,3.84048664669217,149.518825389291));
#52954=CARTESIAN_POINT('Ctrl Pts',(6.82170991802717,4.01080306080901,149.526725756382));
#52955=CARTESIAN_POINT('Ctrl Pts',(6.71831336699858,4.17710264451427,149.534626123473));
#52956=CARTESIAN_POINT('Ctrl Pts',(6.61478214377821,4.34361883050665,149.542536780653));
#52957=CARTESIAN_POINT('Ctrl Pts',(6.50516607441492,4.50610745061167,149.550447437833));
#52958=CARTESIAN_POINT('Ctrl Pts',(6.389830941801,4.66411637239065,149.558358095014));
#52959=CARTESIAN_POINT('Ctrl Pts',(6.33915534438178,4.73354184862885,149.561833855344));
#52960=CARTESIAN_POINT('Ctrl Pts',(6.28737617348114,4.80210296382564,149.565309615674));
#52961=CARTESIAN_POINT('Ctrl Pts',(6.23452673857495,4.86976358214585,149.568785376004));
#52962=CARTESIAN_POINT('Ctrl Pts',(6.11533612381838,5.0223576582549,149.576624211201));
#52963=CARTESIAN_POINT('Ctrl Pts',(5.99035983087738,5.17080368396709,149.584463046398));
#52964=CARTESIAN_POINT('Ctrl Pts',(5.85991829096024,5.31462873804649,149.592301881595));
#52965=CARTESIAN_POINT('Ctrl Pts',(5.72962297355157,5.45829256695022,149.600131929605));
#52966=CARTESIAN_POINT('Ctrl Pts',(5.59387484196166,5.59734548090741,149.607961977615));
#52967=CARTESIAN_POINT('Ctrl Pts',(5.45303667253296,5.73134469806264,149.615792025626));
#52968=CARTESIAN_POINT('Ctrl Pts',(5.31232896916856,5.86521978444739,149.623614820236));
#52969=CARTESIAN_POINT('Ctrl Pts',(5.1665408709855,5.99405025634176,149.631437614847));
#52970=CARTESIAN_POINT('Ctrl Pts',(5.01607448712298,6.11742737918759,149.639260409458));
#52971=CARTESIAN_POINT('Ctrl Pts',(4.86571821943737,6.24071421065578,149.647077479094));
#52972=CARTESIAN_POINT('Ctrl Pts',(4.71069075588652,6.35855541988836,149.654894548729));
#52973=CARTESIAN_POINT('Ctrl Pts',(4.55143016125698,6.47057991892537,149.662711618365));
#52974=CARTESIAN_POINT('Ctrl Pts',(4.39225515036246,6.58254421804248,149.670524487251));
#52975=CARTESIAN_POINT('Ctrl Pts',(4.22885182680198,6.68869783176658,149.678337356136));
#52976=CARTESIAN_POINT('Ctrl Pts',(4.06169050093677,6.78871057525654,149.686150225022));
#52977=CARTESIAN_POINT('Ctrl Pts',(3.89458650789091,6.88868901647876,149.693960414258));
#52978=CARTESIAN_POINT('Ctrl Pts',(3.72372738211049,6.98253060354984,149.701770603493));
#52979=CARTESIAN_POINT('Ctrl Pts',(3.54961167158209,7.06994893764928,149.709580792729));
#52980=CARTESIAN_POINT('Ctrl Pts',(3.3754881087995,7.15737121413266,149.717391334188));
#52981=CARTESIAN_POINT('Ctrl Pts',(3.19810797807609,7.23836949280769,149.725201875647));
#52982=CARTESIAN_POINT('Ctrl Pts',(3.01799410288058,7.3127035079359,149.733012417106));
#52983=CARTESIAN_POINT('Ctrl Pts',(2.83786579167468,7.38704348088726,149.740823584575));
#52984=CARTESIAN_POINT('Ctrl Pts',(2.65500362462042,7.45471799120727,149.748634752044));
#52985=CARTESIAN_POINT('Ctrl Pts',(2.46994997758998,7.5155351178877,149.756445919512));
#52986=CARTESIAN_POINT('Ctrl Pts',(2.28484890716228,7.5763678300743,149.764259088736));
#52987=CARTESIAN_POINT('Ctrl Pts',(2.09755557226844,7.63033954788241,149.77207225796));
#52988=CARTESIAN_POINT('Ctrl Pts',(1.90862720427759,7.67730833007842,149.779885427184));
#52989=CARTESIAN_POINT('Ctrl Pts',(1.71961714309979,7.72429742171523,149.787701974846));
#52990=CARTESIAN_POINT('Ctrl Pts',(1.5289709816044,7.76427746084871,149.795518522507));
#52991=CARTESIAN_POINT('Ctrl Pts',(1.33725597278598,7.79715765284044,149.803335070169));
#52992=CARTESIAN_POINT('Ctrl Pts',(1.14531723083956,7.83007621630996,149.811160739811));
#52993=CARTESIAN_POINT('Ctrl Pts',(0.952307497086017,7.85587832441459,149.818986409454));
#52994=CARTESIAN_POINT('Ctrl Pts',(0.758800081773679,7.8745249657297,149.826812079096));
#52995=CARTESIAN_POINT('Ctrl Pts',(0.565166532832405,7.89318376145518,149.834642849732));
#52996=CARTESIAN_POINT('Ctrl Pts',(0.37103500582103,7.90467777492654,149.842473620369));
#52997=CARTESIAN_POINT('Ctrl Pts',(0.176978712829425,7.90902013748892,149.850304391005));
#52998=CARTESIAN_POINT('Ctrl Pts',(-0.0173579684307403,7.91336877424886,
149.858146476173));
#52999=CARTESIAN_POINT('Ctrl Pts',(-0.211618848159001,7.91054512626607,
149.865988561342));
#53000=CARTESIAN_POINT('Ctrl Pts',(-0.40523472985427,7.90061426812624,149.873830646511));
#53001=CARTESIAN_POINT('Ctrl Pts',(-0.513754139792657,7.89504813968636,
149.878226042424));
#53002=CARTESIAN_POINT('Ctrl Pts',(-0.622071072280622,7.88725023103341,
149.882621438338));
#53003=CARTESIAN_POINT('Ctrl Pts',(-0.730086817096597,7.87723899850079,
149.887016834251));
#53004=CARTESIAN_POINT('Ctrl Pts',(-0.924632870215468,7.85920786998898,
149.894933336871));
#53005=CARTESIAN_POINT('Ctrl Pts',(-1.11878517603069,7.83393988467338,149.902849839492));
#53006=CARTESIAN_POINT('Ctrl Pts',(-1.31196385325694,7.80145318820457,149.910766342112));
#53007=CARTESIAN_POINT('Ctrl Pts',(-1.50491997773897,7.76900391824449,149.918673724474));
#53008=CARTESIAN_POINT('Ctrl Pts',(-1.69690437138156,7.72935255834266,149.926581106836));
#53009=CARTESIAN_POINT('Ctrl Pts',(-1.88734000174799,7.68256914826036,149.934488489198));
#53010=CARTESIAN_POINT('Ctrl Pts',(-2.0775915287638,7.63583096596728,149.942388227111));
#53011=CARTESIAN_POINT('Ctrl Pts',(-2.26629694287303,7.58197455009893,149.950287965023));
#53012=CARTESIAN_POINT('Ctrl Pts',(-2.4528868795594,7.52112138953264,149.958187702936));
#53013=CARTESIAN_POINT('Ctrl Pts',(-2.63933099515242,7.46031578605632,149.966081267158));
#53014=CARTESIAN_POINT('Ctrl Pts',(-2.82366260106464,7.39252443812066,149.973974831381));
#53015=CARTESIAN_POINT('Ctrl Pts',(-3.00532475653873,7.31791938379588,149.981868395604));
#53016=CARTESIAN_POINT('Ctrl Pts',(-3.18687858504193,7.24335881721554,149.989757252814));
#53017=CARTESIAN_POINT('Ctrl Pts',(-3.36576581712271,7.16199277082344,149.997646110025));
#53018=CARTESIAN_POINT('Ctrl Pts',(-3.54144658530784,7.07404248527046,150.005534967236));
#53019=CARTESIAN_POINT('Ctrl Pts',(-3.71705512255395,6.98612836037284,150.013420580953));
#53020=CARTESIAN_POINT('Ctrl Pts',(-3.8894595156393,6.89163554546707,150.021306194669));
#53021=CARTESIAN_POINT('Ctrl Pts',(-4.05814147153863,6.79083270276763,150.029191808386));
#53022=CARTESIAN_POINT('Ctrl Pts',(-4.22680842775133,6.69003882374805,150.037076720891));
#53023=CARTESIAN_POINT('Ctrl Pts',(-4.3917533072821,6.58293620598582,150.044961633396));
#53024=CARTESIAN_POINT('Ctrl Pts',(-4.5524835030535,6.46983886618714,150.052846545901));
#53025=CARTESIAN_POINT('Ctrl Pts',(-4.7132131450218,6.35674191607042,150.060731431238));
#53026=CARTESIAN_POINT('Ctrl Pts',(-4.86972784991524,6.23765048298116,150.068616316575));
#53027=CARTESIAN_POINT('Ctrl Pts',(-5.02156494712211,6.11292127234063,150.076501201912));
#53028=CARTESIAN_POINT('Ctrl Pts',(-5.1734269962266,5.98817156453206,150.084387382999));
#53029=CARTESIAN_POINT('Ctrl Pts',(-5.32060963964438,5.85778245193239,150.092273564086));
#53030=CARTESIAN_POINT('Ctrl Pts',(-5.46268399640442,5.72215034365815,150.100159745172));
#53031=CARTESIAN_POINT('Ctrl Pts',(-5.60480553789616,5.58647319020626,150.108048545362));
#53032=CARTESIAN_POINT('Ctrl Pts',(-5.74181516327823,5.4455498095179,150.115937345551));
#53033=CARTESIAN_POINT('Ctrl Pts',(-5.87332132991007,5.29981297364571,150.123826145741));
#53034=CARTESIAN_POINT('Ctrl Pts',(-6.00495478942234,5.15393507015595,150.131722581984));
#53035=CARTESIAN_POINT('Ctrl Pts',(-6.13107391858747,5.00323466098418,150.139619018227));
#53036=CARTESIAN_POINT('Ctrl Pts',(-6.25132724132941,4.84817787646172,150.147515454469));
#53037=CARTESIAN_POINT('Ctrl Pts',(-6.37164703148385,4.69303538766912,150.155416255296));
#53038=CARTESIAN_POINT('Ctrl Pts',(-6.48609435037436,4.53353200209237,150.163317056122));
#53039=CARTESIAN_POINT('Ctrl Pts',(-6.59436130100118,4.3701624720207,150.171217856949));
#53040=CARTESIAN_POINT('Ctrl Pts',(-6.70275981733189,4.20659441574048,150.179128258807));
#53041=CARTESIAN_POINT('Ctrl Pts',(-6.80496278437607,4.03915112393029,150.187038660665));
#53042=CARTESIAN_POINT('Ctrl Pts',(-6.90070792484196,3.86835250927618,150.194949062523));
#53043=CARTESIAN_POINT('Ctrl Pts',(-6.94226085891219,3.79422672556044,150.198382139181));
#53044=CARTESIAN_POINT('Ctrl Pts',(-6.9825980577417,3.71946922999763,150.20181521584));
#53045=CARTESIAN_POINT('Ctrl Pts',(-7.02170091700514,3.64412365763418,150.205248292498));
#53046=CARTESIAN_POINT('Ctrl Pts',(-7.11711963402917,3.4602655463916,150.213625679123));
#53047=CARTESIAN_POINT('Ctrl Pts',(-7.20539118102205,3.27250754448863,150.222003065747));
#53048=CARTESIAN_POINT('Ctrl Pts',(-7.28620562234504,3.08141665941292,150.230380452372));
#53049=CARTESIAN_POINT('Ctrl Pts',(-7.36691453401297,2.89057530591668,150.238746899582));
#53050=CARTESIAN_POINT('Ctrl Pts',(-7.440185654043,2.69641001091652,150.247113346791));
#53051=CARTESIAN_POINT('Ctrl Pts',(-7.50575542314802,2.49951125780305,150.255479794001));
#53052=CARTESIAN_POINT('Ctrl Pts',(-7.57249511513446,2.29909935587516,150.263995518814));
#53053=CARTESIAN_POINT('Ctrl Pts',(-7.63125588850341,2.09585578156161,150.272511243628));
#53054=CARTESIAN_POINT('Ctrl Pts',(-7.68181022303012,1.89042659136765,150.281026968441));
#53055=CARTESIAN_POINT('Ctrl Pts',(-7.73133129727984,1.68919608807067,150.289368643685));
#53056=CARTESIAN_POINT('Ctrl Pts',(-7.77297801270694,1.48586872873715,150.297710318929));
#53057=CARTESIAN_POINT('Ctrl Pts',(-7.80658574964955,1.28106983937982,150.306051994172));
#53058=CARTESIAN_POINT('Ctrl Pts',(-7.84124532785696,1.06986123778334,150.314654743771));
#53059=CARTESIAN_POINT('Ctrl Pts',(-7.86735446370792,0.857087777498576,
150.323257493369));
#53060=CARTESIAN_POINT('Ctrl Pts',(-7.88478865212675,0.643450783893536,
150.331860242968));
#53061=CARTESIAN_POINT('Ctrl Pts',(-7.90222284054558,0.429813790288495,
150.340462992566));
#53062=CARTESIAN_POINT('Ctrl Pts',(-7.91098199912815,0.21531358928186,150.349065742165));
#53063=CARTESIAN_POINT('Ctrl Pts',(-7.9109999722679,0.000662402618438335,
150.357668491763));
#53064=CARTESIAN_POINT('',(-7.90811390162807,-0.00405051921047928,152.357668491763));
#53065=CARTESIAN_POINT('Ctrl Pts',(-7.911,1.33226762955019E-14,150.357668491763));
#53066=CARTESIAN_POINT('Ctrl Pts',(-7.911,-2.20167589666678,150.446255927496));
#53067=CARTESIAN_POINT('Ctrl Pts',(-6.94214576672369,-4.38610418338688,
150.534843363228));
#53068=CARTESIAN_POINT('Ctrl Pts',(-3.67820201488277,-7.34180684107638,
150.712018234694));
#53069=CARTESIAN_POINT('Ctrl Pts',(-1.4086817587173,-8.0899266657134,150.800605670427));
#53070=CARTESIAN_POINT('Ctrl Pts',(2.97309270521293,-7.6545422802525,150.977780541892));
#53071=CARTESIAN_POINT('Ctrl Pts',(5.05102072675621,-6.47444880834212,151.066367977625));
#53072=CARTESIAN_POINT('Ctrl Pts',(7.66951518847883,-2.9342519536768,151.24354284909));
#53073=CARTESIAN_POINT('Ctrl Pts',(8.18956872247074,-0.60188196009885,151.332130284823));
#53074=CARTESIAN_POINT('Ctrl Pts',(7.32306689761327,3.71537198232483,151.509305156288));
#53075=CARTESIAN_POINT('Ctrl Pts',(5.94329958850174,5.66643518936541,151.597892592021));
#53076=CARTESIAN_POINT('Ctrl Pts',(2.16154501637804,7.92205913233011,151.775067463487));
#53077=CARTESIAN_POINT('Ctrl Pts',(-0.210816529300861,8.20894963713002,
151.863654899219));
#53078=CARTESIAN_POINT('Ctrl Pts',(-4.42123908576484,6.91982244717802,152.040829770685));
#53079=CARTESIAN_POINT('Ctrl Pts',(-6.22631625634226,5.35390358803477,152.129417206418));
#53080=CARTESIAN_POINT('Ctrl Pts',(-7.65317280859495,2.31334857514485,152.264559258688));
#53081=CARTESIAN_POINT('Ctrl Pts',(-7.91099999999997,1.15702837836512,152.311113875225));
#53082=CARTESIAN_POINT('Ctrl Pts',(-7.911,1.84297022087776E-13,152.357668491763));
#53083=CARTESIAN_POINT('',(5.2614341371596,-5.92453136998931,153.089));
#53084=CARTESIAN_POINT('Ctrl Pts',(-7.90647091379303,-0.00635638440671541,
152.357668491763));
#53085=CARTESIAN_POINT('Ctrl Pts',(-7.91213139978848,-0.629379302256461,
152.38273516125));
#53086=CARTESIAN_POINT('Ctrl Pts',(-7.70330066450379,-2.56750138527614,
152.460840407114));
#53087=CARTESIAN_POINT('Ctrl Pts',(-6.0944015489518,-5.52158318776385,152.591984229347));
#53088=CARTESIAN_POINT('Ctrl Pts',(-1.59537475001636,-8.5823965927603,152.804138534849));
#53089=CARTESIAN_POINT('Ctrl Pts',(3.00709256577575,-7.82448181932476,152.969810458397));
#53090=CARTESIAN_POINT('Ctrl Pts',(5.1407390732733,-6.03284475623591,153.082443805573));
#53091=CARTESIAN_POINT('Ctrl Pts',(5.2614341371596,-5.92453136998931,153.089));
#53092=CARTESIAN_POINT('',(-1.31895459586133,-7.80015452554508,153.089118084603));
#53093=CARTESIAN_POINT('Origin',(0.,0.,153.089));
#53094=CARTESIAN_POINT('',(-7.9024637590362,0.00270873549297636,152.642331508237));
#53095=CARTESIAN_POINT('Ctrl Pts',(-1.31926283107568,-7.80022221366431,
153.089));
#53096=CARTESIAN_POINT('Ctrl Pts',(-3.4855731451168,-7.43383102638713,153.00059764804));
#53097=CARTESIAN_POINT('Ctrl Pts',(-5.47418924799311,-6.11917608473493,
152.91219529608));
#53098=CARTESIAN_POINT('Ctrl Pts',(-7.47127099337646,-3.00398534954474,
152.763305798825));
#53099=CARTESIAN_POINT('Ctrl Pts',(-7.91100000000169,-1.50329545889063,
152.702818653531));
#53100=CARTESIAN_POINT('Ctrl Pts',(-7.911,8.90509888051838E-12,152.642331508237));
#53101=CARTESIAN_POINT('',(-7.92179161750093,0.00222580852156247,150.642443359737));
#53102=CARTESIAN_POINT('Ctrl Pts',(-7.89956579123653,0.00362832389775192,
152.642331508237));
#53103=CARTESIAN_POINT('Ctrl Pts',(-7.90553504434981,1.01558807491038,152.601762501006));
#53104=CARTESIAN_POINT('Ctrl Pts',(-7.25780544737249,4.66357791674521,152.455259113975));
#53105=CARTESIAN_POINT('Ctrl Pts',(-1.76836855728288,9.18370799003887,152.202821347136));
#53106=CARTESIAN_POINT('Ctrl Pts',(6.76945915019856,6.45863669117592,151.88501820773));
#53107=CARTESIAN_POINT('Ctrl Pts',(8.69546239001067,-0.742159892978413,
151.620182258224));
#53108=CARTESIAN_POINT('Ctrl Pts',(6.0989790094406,-5.51533468420419,151.408313498619));
#53109=CARTESIAN_POINT('Ctrl Pts',(1.60954184334504,-8.57675766711039,151.196444739013));
#53110=CARTESIAN_POINT('Ctrl Pts',(-5.48070072932496,-7.42723891679903,
150.941154692719));
#53111=CARTESIAN_POINT('Ctrl Pts',(-7.90535662791195,-2.38546751608027,
150.738831836327));
#53112=CARTESIAN_POINT('Ctrl Pts',(-7.92179161750093,0.00222580852156247,
150.642443359737));
#53113=CARTESIAN_POINT('',(-7.91099986105201,0.00147982984735487,146.642308865166));
#53114=CARTESIAN_POINT('Ctrl Pts',(-7.91099961209329,0.00247738972013287,
150.648656354446));
#53115=CARTESIAN_POINT('Ctrl Pts',(-7.91092915531688,0.22746562077841,150.640490528989));
#53116=CARTESIAN_POINT('Ctrl Pts',(-7.90126072315176,0.452335888079179,
150.632016437377));
#53117=CARTESIAN_POINT('Ctrl Pts',(-7.88142029371198,0.683509341423131,
150.622712655205));
#53118=CARTESIAN_POINT('Ctrl Pts',(-7.88080703590663,0.690544226057316,
150.622428961552));
#53119=CARTESIAN_POINT('Ctrl Pts',(-7.87979645475322,0.701960243835202,
150.621967655276));
#53120=CARTESIAN_POINT('Ctrl Pts',(-7.8794048931755,0.706341901386491,150.621790374355));
#53121=CARTESIAN_POINT('Ctrl Pts',(-7.87870958632744,0.714050006509404,
150.621478108927));
#53122=CARTESIAN_POINT('Ctrl Pts',(-7.87840738927717,0.7173765859027,150.62134321488));
#53123=CARTESIAN_POINT('Ctrl Pts',(-7.87781270219561,0.72387719203348,150.621079360247));
#53124=CARTESIAN_POINT('Ctrl Pts',(-7.87752040051,0.727051235824467,150.620950410523));
#53125=CARTESIAN_POINT('Ctrl Pts',(-7.87693567713893,0.733358877483924,
150.620693921517));
#53126=CARTESIAN_POINT('Ctrl Pts',(-7.87664330364484,0.736492479298589,
150.620566385013));
#53127=CARTESIAN_POINT('Ctrl Pts',(-7.87595355558775,0.743837674280561,
150.62026717187));
#53128=CARTESIAN_POINT('Ctrl Pts',(-7.87555467300646,0.74804912125201,150.62009540955));
#53129=CARTESIAN_POINT('Ctrl Pts',(-7.87416074740549,0.762641646552916,
150.619499552508));
#53130=CARTESIAN_POINT('Ctrl Pts',(-7.87314855891915,0.77302103741235,150.619074491792));
#53131=CARTESIAN_POINT('Ctrl Pts',(-7.86220563995538,0.882982879789421,
150.614558392151));
#53132=CARTESIAN_POINT('Ctrl Pts',(-7.85040703174,0.98236661591551,150.610364643893));
#53133=CARTESIAN_POINT('Ctrl Pts',(-7.83230316470806,1.11355072941246,150.604705042791));
#53134=CARTESIAN_POINT('Ctrl Pts',(-7.82768288061923,1.14557791759272,150.603313487368));
#53135=CARTESIAN_POINT('Ctrl Pts',(-7.81770376236306,1.21187116827608,150.600413997071));
#53136=CARTESIAN_POINT('Ctrl Pts',(-7.81231581911655,1.24613214977066,150.598904911465));
#53137=CARTESIAN_POINT('Ctrl Pts',(-7.79915336916526,1.32638742096287,150.595346780335));
#53138=CARTESIAN_POINT('Ctrl Pts',(-7.79119703413402,1.37235036631787,150.593291132861));
#53139=CARTESIAN_POINT('Ctrl Pts',(-7.77883640223423,1.44018146708135,150.590233600891));
#53140=CARTESIAN_POINT('Ctrl Pts',(-7.77474526793858,1.46210616521036,150.58924163456));
#53141=CARTESIAN_POINT('Ctrl Pts',(-7.63817637445548,2.17720561654808,150.556772906631));
#53142=CARTESIAN_POINT('Ctrl Pts',(-7.41363400925527,2.84959123214577,150.523084960769));
#53143=CARTESIAN_POINT('Ctrl Pts',(-6.96836842988337,3.75752981011897,150.478479563164));
#53144=CARTESIAN_POINT('Ctrl Pts',(-6.81812488277147,4.02372822725777,150.465467174321));
#53145=CARTESIAN_POINT('Ctrl Pts',(-6.62877818709735,4.31800882587217,150.451191974965));
#53146=CARTESIAN_POINT('Ctrl Pts',(-6.60438877748413,4.35522093971914,150.449388648229));
#53147=CARTESIAN_POINT('Ctrl Pts',(-6.57321429408625,4.40192125513837,150.447127481806));
#53148=CARTESIAN_POINT('Ctrl Pts',(-6.56672066965125,4.41160249123715,150.446658836459));
#53149=CARTESIAN_POINT('Ctrl Pts',(-6.55634520189289,4.42699743703263,150.445913766547));
#53150=CARTESIAN_POINT('Ctrl Pts',(-6.55247724495641,4.43272045909914,150.445636825025));
#53151=CARTESIAN_POINT('Ctrl Pts',(-6.54517393652263,4.44349597386237,150.445115454841));
#53152=CARTESIAN_POINT('Ctrl Pts',(-6.54174021929269,4.44854956503452,150.444870965467));
#53153=CARTESIAN_POINT('Ctrl Pts',(-6.53400412025852,4.45990688284943,150.444321565301));
#53154=CARTESIAN_POINT('Ctrl Pts',(-6.52969846117015,4.46620837555204,150.444016777363));
#53155=CARTESIAN_POINT('Ctrl Pts',(-6.51871961956967,4.48222650759002,150.443242119683));
#53156=CARTESIAN_POINT('Ctrl Pts',(-6.51203381647745,4.49193449623709,150.442772723128));
#53157=CARTESIAN_POINT('Ctrl Pts',(-6.47485440910975,4.54566265914021,150.440175369299));
#53158=CARTESIAN_POINT('Ctrl Pts',(-6.44393581119019,4.58938776216048,150.438063420303));
#53159=CARTESIAN_POINT('Ctrl Pts',(-5.86439432450722,5.39157143238999,150.399338193375));
#53160=CARTESIAN_POINT('Ctrl Pts',(-5.18602585089256,6.0468999811995,150.369205450616));
#53161=CARTESIAN_POINT('Ctrl Pts',(-4.29766747739003,6.64318696381936,150.330642404276));
#53162=CARTESIAN_POINT('Ctrl Pts',(-4.18452541402164,6.7150296796407,150.325723539682));
#53163=CARTESIAN_POINT('Ctrl Pts',(-3.99123665528837,6.83098128384793,150.317219859528));
#53164=CARTESIAN_POINT('Ctrl Pts',(-3.91204945372838,6.87663750790894,150.313708624991));
#53165=CARTESIAN_POINT('Ctrl Pts',(-3.80531660668065,6.935735231399,150.30891689159));
#53166=CARTESIAN_POINT('Ctrl Pts',(-3.77845627990965,6.95040472016694,150.307706087798));
#53167=CARTESIAN_POINT('Ctrl Pts',(-3.74017508790437,6.9710241084333,150.305972568751));
#53168=CARTESIAN_POINT('Ctrl Pts',(-3.72882351830667,6.97710269197855,150.305457546377));
#53169=CARTESIAN_POINT('Ctrl Pts',(-3.70886608630795,6.98772696074326,150.304550271655));
#53170=CARTESIAN_POINT('Ctrl Pts',(-3.70026655700388,6.99228454295532,150.304158746885));
#53171=CARTESIAN_POINT('Ctrl Pts',(-3.68764993785024,6.99894131132883,150.303583440944));
#53172=CARTESIAN_POINT('Ctrl Pts',(-3.68363939239396,7.00105294725003,150.303400432494));
#53173=CARTESIAN_POINT('Ctrl Pts',(-3.67671920949135,7.00468897556172,150.303084421928));
#53174=CARTESIAN_POINT('Ctrl Pts',(-3.67381042798319,7.00621500733765,150.302951522165));
#53175=CARTESIAN_POINT('Ctrl Pts',(-3.66801538494513,7.0092506550434,150.302686610709));
#53176=CARTESIAN_POINT('Ctrl Pts',(-3.66512914652523,7.01076029747543,150.302554601436));
#53177=CARTESIAN_POINT('Ctrl Pts',(-3.6582729623709,7.01434102269576,150.302240853811));
#53178=CARTESIAN_POINT('Ctrl Pts',(-3.65430219280813,7.01641051631357,150.302059016685));
#53179=CARTESIAN_POINT('Ctrl Pts',(-3.64240530506515,7.02259812148763,150.301513828318));
#53180=CARTESIAN_POINT('Ctrl Pts',(-3.63447399238149,7.02670616859194,150.301149858019));
#53181=CARTESIAN_POINT('Ctrl Pts',(-3.55935828942507,7.06545136890281,150.297698092285));
#53182=CARTESIAN_POINT('Ctrl Pts',(-3.49168957346997,7.0991364073923,150.294553136003));
#53183=CARTESIAN_POINT('Ctrl Pts',(-3.16059923639091,7.25807205917222,150.279033846659));
#53184=CARTESIAN_POINT('Ctrl Pts',(-2.89088412413446,7.36965155334711,150.265997445874));
#53185=CARTESIAN_POINT('Ctrl Pts',(-2.47660163127544,7.51479018988298,150.246023640053));
#53186=CARTESIAN_POINT('Ctrl Pts',(-2.33622482441889,7.55960845750603,150.239262669616));
#53187=CARTESIAN_POINT('Ctrl Pts',(-2.15189696983936,7.61283412606556,150.230450982739));
#53188=CARTESIAN_POINT('Ctrl Pts',(-2.10901043563407,7.6248264887977,150.228405361108));
#53189=CARTESIAN_POINT('Ctrl Pts',(-2.01687265776054,7.64975414414357,150.22402252869));
#53190=CARTESIAN_POINT('Ctrl Pts',(-1.96759304643228,7.66257733451901,150.221685688397));
#53191=CARTESIAN_POINT('Ctrl Pts',(-1.86076081896549,7.6892779027404,150.216638647553));
#53192=CARTESIAN_POINT('Ctrl Pts',(-1.80316910481317,7.7029868707906,150.213929678311));
#53193=CARTESIAN_POINT('Ctrl Pts',(-1.67665362859226,7.73160563237193,150.20800913758));
#53194=CARTESIAN_POINT('Ctrl Pts',(-1.6076731120852,7.74624298387695,150.204800723056));
#53195=CARTESIAN_POINT('Ctrl Pts',(-1.30429137802051,7.80639209773261,150.190789500558));
#53196=CARTESIAN_POINT('Ctrl Pts',(-1.06808583121151,7.84220226626713,150.180145587103));
#53197=CARTESIAN_POINT('Ctrl Pts',(-0.644322659858789,7.88694234952294,
150.161657657725));
#53198=CARTESIAN_POINT('Ctrl Pts',(-0.457387220624849,7.89998825052059,
150.153709218142));
#53199=CARTESIAN_POINT('Ctrl Pts',(-0.1826563605207,7.90937562606933,150.142342655629));
#53200=CARTESIAN_POINT('Ctrl Pts',(-0.0951113524039408,7.91091275458935,
150.138767041912));
#53201=CARTESIAN_POINT('Ctrl Pts',(0.00677694519215901,7.91101008302992,
150.134658277288));
#53202=CARTESIAN_POINT('Ctrl Pts',(0.0211109007411958,7.91098481817794,
150.134081454107));
#53203=CARTESIAN_POINT('Ctrl Pts',(0.0429375071318609,7.91088702440545,
150.133204944196));
#53204=CARTESIAN_POINT('Ctrl Pts',(0.0504302184334194,7.91084280818981,
150.132904381373));
#53205=CARTESIAN_POINT('Ctrl Pts',(0.0634380765365338,7.91074756452198,
150.132383151844));
#53206=CARTESIAN_POINT('Ctrl Pts',(0.0689532474881799,7.91070141447408,
150.132162334252));
#53207=CARTESIAN_POINT('Ctrl Pts',(0.0804269928389719,7.91059340423459,
150.131703313708));
#53208=CARTESIAN_POINT('Ctrl Pts',(0.0863855553656897,7.91053057919053,
150.131465140801));
#53209=CARTESIAN_POINT('Ctrl Pts',(0.100924328230168,7.91036085846773,150.130884505442));
#53210=CARTESIAN_POINT('Ctrl Pts',(0.109504455761332,7.91024673483588,150.13054226708));
#53211=CARTESIAN_POINT('Ctrl Pts',(0.142072888911172,7.9097605444271,150.129244809737));
#53212=CARTESIAN_POINT('Ctrl Pts',(0.166059757534419,7.90929331518965,150.128292540732));
#53213=CARTESIAN_POINT('Ctrl Pts',(0.229241307182391,7.9077750801567,150.125792859797));
#53214=CARTESIAN_POINT('Ctrl Pts',(0.26843114365175,7.90654178965083,150.124251098044));
#53215=CARTESIAN_POINT('Ctrl Pts',(1.17057048911248,7.87143654261414,150.088954905694));
#53216=CARTESIAN_POINT('Ctrl Pts',(2.02208939794266,7.69680456498812,150.060606833125));
#53217=CARTESIAN_POINT('Ctrl Pts',(3.05347760895975,7.30193122630002,150.021909974678));
#53218=CARTESIAN_POINT('Ctrl Pts',(3.27433704111667,7.20559715699836,150.01328328766));
#53219=CARTESIAN_POINT('Ctrl Pts',(3.57069949098794,7.05988835973848,150.000823008299));
#53220=CARTESIAN_POINT('Ctrl Pts',(3.65027582538324,7.01907429375369,149.997386108494));
#53221=CARTESIAN_POINT('Ctrl Pts',(3.75486174685292,6.96317347458829,149.992725813978));
#53222=CARTESIAN_POINT('Ctrl Pts',(3.78050628824733,6.94928368544182,149.991571512775));
#53223=CARTESIAN_POINT('Ctrl Pts',(3.81690770495389,6.92930655366915,149.989915674117));
#53224=CARTESIAN_POINT('Ctrl Pts',(3.82772826294864,6.92333518506525,149.98942126979));
#53225=CARTESIAN_POINT('Ctrl Pts',(3.84673886240101,6.91278591874854,149.988548710246));
#53226=CARTESIAN_POINT('Ctrl Pts',(3.85493485810317,6.90821874815308,149.988171232345));
#53227=CARTESIAN_POINT('Ctrl Pts',(3.86696640198103,6.90148616215294,149.987615173184));
#53228=CARTESIAN_POINT('Ctrl Pts',(3.87080832298895,6.89933209281672,149.987437322277));
#53229=CARTESIAN_POINT('Ctrl Pts',(3.87744847555632,6.89560183261177,149.987129430601));
#53230=CARTESIAN_POINT('Ctrl Pts',(3.88024755340246,6.89402714230009,149.986999487304));
#53231=CARTESIAN_POINT('Ctrl Pts',(3.88580670322695,6.89089524721308,149.986741101565));
#53232=CARTESIAN_POINT('Ctrl Pts',(3.88856679997324,6.88933808758115,149.986612662081));
#53233=CARTESIAN_POINT('Ctrl Pts',(3.89508532224324,6.88565537739181,149.986308965672));
#53234=CARTESIAN_POINT('Ctrl Pts',(3.89884294200569,6.88352840898737,149.986133615303));
#53235=CARTESIAN_POINT('Ctrl Pts',(3.91208808982789,6.87601678189935,149.985514520991));
#53236=CARTESIAN_POINT('Ctrl Pts',(3.92156616709638,6.8706156057767,149.985069685711));
#53237=CARTESIAN_POINT('Ctrl Pts',(4.04493159692747,6.79997615786413,149.979256375689));
#53238=CARTESIAN_POINT('Ctrl Pts',(4.15718397927057,6.73193621906005,149.973706780942));
#53239=CARTESIAN_POINT('Ctrl Pts',(4.57667742043928,6.46317344511306,149.952131008886));
#53240=CARTESIAN_POINT('Ctrl Pts',(4.87150381807986,6.24395776364467,149.935236049072));
#53241=CARTESIAN_POINT('Ctrl Pts',(5.6057130212541,5.6142915080586,149.890493496174));
#53242=CARTESIAN_POINT('Ctrl Pts',(6.01549453998622,5.17284191857809,149.862812196008));
#53243=CARTESIAN_POINT('Ctrl Pts',(6.46386527732439,4.56362718872494,149.830728989147));
#53244=CARTESIAN_POINT('Ctrl Pts',(6.55258410245583,4.43530075497591,149.824255795098));
#53245=CARTESIAN_POINT('Ctrl Pts',(6.6533305152101,4.27994922851812,149.816747317899));
#53246=CARTESIAN_POINT('Ctrl Pts',(6.66907090493354,4.25538078586971,149.815569314261));
#53247=CARTESIAN_POINT('Ctrl Pts',(6.68988708159433,4.22249059395434,149.81400476241));
#53248=CARTESIAN_POINT('Ctrl Pts',(6.69508382794791,4.21424590148369,149.81361360942));
#53249=CARTESIAN_POINT('Ctrl Pts',(6.70362328881433,4.20064229524931,149.812969917956));
#53250=CARTESIAN_POINT('Ctrl Pts',(6.70697483738707,4.19528895570661,149.81271704406));
#53251=CARTESIAN_POINT('Ctrl Pts',(6.71347920027869,4.18487199418691,149.812225822908));
#53252=CARTESIAN_POINT('Ctrl Pts',(6.71663270509428,4.17980880966691,149.811987449555));
#53253=CARTESIAN_POINT('Ctrl Pts',(6.72393195790878,4.1680597300926,149.811435198014));
#53254=CARTESIAN_POINT('Ctrl Pts',(6.72807346878722,4.1613712027745,149.811121480302));
#53255=CARTESIAN_POINT('Ctrl Pts',(6.74142747226627,4.13973248093241,149.810108694158));
#53256=CARTESIAN_POINT('Ctrl Pts',(6.75060019497805,4.1247577371651,149.809411127749));
#53257=CARTESIAN_POINT('Ctrl Pts',(6.8355855099744,3.98497384785066,149.802930231968));
#53258=CARTESIAN_POINT('Ctrl Pts',(6.90798067081007,3.85811504668108,149.797276358375));
#53259=CARTESIAN_POINT('Ctrl Pts',(6.98057463752772,3.7223060041083,149.791441284305));
#53260=CARTESIAN_POINT('Ctrl Pts',(6.98431342346669,3.71528602687971,149.791140269718));
#53261=CARTESIAN_POINT('Ctrl Pts',(6.9986925448824,3.68818925162454,149.78998066874));
#53262=CARTESIAN_POINT('Ctrl Pts',(7.00925699401844,3.6680722041987,149.789124629275));
#53263=CARTESIAN_POINT('Ctrl Pts',(7.03127382170546,3.62570484967388,149.787331786412));
#53264=CARTESIAN_POINT('Ctrl Pts',(7.04270760100052,3.60344513934872,149.78639559728));
#53265=CARTESIAN_POINT('Ctrl Pts',(7.40076418251151,2.89815299162774,149.756910516542));
#53266=CARTESIAN_POINT('Ctrl Pts',(7.64643153588114,2.16853727568436,149.732186654909));
#53267=CARTESIAN_POINT('Ctrl Pts',(7.81762026450783,1.22690391307422,149.698291697599));
#53268=CARTESIAN_POINT('Ctrl Pts',(7.84498757865914,1.03761404069944,149.691353038888));
#53269=CARTESIAN_POINT('Ctrl Pts',(7.87666113311587,0.743668332854099,149.680142740212));
#53270=CARTESIAN_POINT('Ctrl Pts',(7.88579372141803,0.639600569253509,149.676089960124));
#53271=CARTESIAN_POINT('Ctrl Pts',(7.8936674117543,0.523523799019757,149.671446505456));
#53272=CARTESIAN_POINT('Ctrl Pts',(7.89444534213445,0.511659176303168,149.670970452013));
#53273=CARTESIAN_POINT('Ctrl Pts',(7.89576727185624,0.490776737161409,149.670129985119));
#53274=CARTESIAN_POINT('Ctrl Pts',(7.89632257898012,0.481759633472731,149.669766221055));
#53275=CARTESIAN_POINT('Ctrl Pts',(7.89711690924771,0.468490827856677,149.669229663842));
#53276=CARTESIAN_POINT('Ctrl Pts',(7.89736794882502,0.464239824707906,149.669057571748));
#53277=CARTESIAN_POINT('Ctrl Pts',(7.897796524426,0.456881544265296,149.668759352879));
#53278=CARTESIAN_POINT('Ctrl Pts',(7.89797565957893,0.453774357329536,149.668633320134));
#53279=CARTESIAN_POINT('Ctrl Pts',(7.89832832302281,0.447593764138455,149.668382417317));
#53280=CARTESIAN_POINT('Ctrl Pts',(7.89850189054344,0.444520371820042,149.668257549902));
#53281=CARTESIAN_POINT('Ctrl Pts',(7.89891079728028,0.437203928901474,149.667960050495));
#53282=CARTESIAN_POINT('Ctrl Pts',(7.89914451096828,0.432960799074963,149.667787323018));
#53283=CARTESIAN_POINT('Ctrl Pts',(7.89996148959228,0.417907481939246,149.6671738548));
#53284=CARTESIAN_POINT('Ctrl Pts',(7.90052598089328,0.407096331918799,149.666732015811));
#53285=CARTESIAN_POINT('Ctrl Pts',(7.90761760016446,0.265704419743534,149.660937439552));
#53286=CARTESIAN_POINT('Ctrl Pts',(7.91092847763104,0.134988999559838,149.655401499155));
#53287=CARTESIAN_POINT('Ctrl Pts',(7.91100386771795,-0.00505529020108679,
149.649323498358));
#53288=CARTESIAN_POINT('Ctrl Pts',(7.91099243291304,-0.0143692827151416,
149.648918568706));
#53289=CARTESIAN_POINT('Ctrl Pts',(7.9089385233884,-0.70044224624324,149.619040988456));
#53290=CARTESIAN_POINT('Ctrl Pts',(7.82008407366501,-1.37413713735386,149.586362036858));
#53291=CARTESIAN_POINT('Ctrl Pts',(7.63563525924089,-2.06949538491413,149.553463641788));
#53292=CARTESIAN_POINT('Ctrl Pts',(7.62437669984048,-2.1105963495069,149.551521125052));
#53293=CARTESIAN_POINT('Ctrl Pts',(7.59963202440341,-2.19814771870425,149.547388760209));
#53294=CARTESIAN_POINT('Ctrl Pts',(7.58605086525964,-2.24456959187779,149.545201004147));
#53295=CARTESIAN_POINT('Ctrl Pts',(7.55573789075456,-2.34476373549494,149.540487782271));
#53296=CARTESIAN_POINT('Ctrl Pts',(7.53885585049072,-2.39848799449484,149.537966012219));
#53297=CARTESIAN_POINT('Ctrl Pts',(7.5001815210725,-2.51711843053026,149.532411726644));
#53298=CARTESIAN_POINT('Ctrl Pts',(7.47811726366694,-2.58193154771427,149.529386638262));
#53299=CARTESIAN_POINT('Ctrl Pts',(7.36654419751321,-2.89623967871215,149.514768690928));
#53300=CARTESIAN_POINT('Ctrl Pts',(7.26537203284612,-3.14142728292245,149.5035344786));
#53301=CARTESIAN_POINT('Ctrl Pts',(7.13462767580495,-3.41799283883676,149.491065139604));
#53302=CARTESIAN_POINT('Ctrl Pts',(7.11689686531971,-3.45475993291284,149.489411501405));
#53303=CARTESIAN_POINT('Ctrl Pts',(7.0939890648529,-3.50133732567146,149.487321549054));
#53304=CARTESIAN_POINT('Ctrl Pts',(7.08907510291591,-3.51127585172964,149.486875887958));
#53305=CARTESIAN_POINT('Ctrl Pts',(7.08118086248714,-3.52715789256235,149.486164159051));
#53306=CARTESIAN_POINT('Ctrl Pts',(7.0782139645453,-3.53310801967908,149.485897614621));
#53307=CARTESIAN_POINT('Ctrl Pts',(7.07258642472409,-3.5443585368482,149.485393821232));
#53308=CARTESIAN_POINT('Ctrl Pts',(7.06992731782188,-3.54965968704581,149.485156517745));
#53309=CARTESIAN_POINT('Ctrl Pts',(7.06390335035979,-3.56163534460087,149.484620611652));
#53310=CARTESIAN_POINT('Ctrl Pts',(7.06053498418739,-3.56830808768019,149.484322134515));
#53311=CARTESIAN_POINT('Ctrl Pts',(7.05188302436484,-3.58538743008752,149.483558479371));
#53312=CARTESIAN_POINT('Ctrl Pts',(7.04658584102068,-3.5957871460654,149.483093787532));
#53313=CARTESIAN_POINT('Ctrl Pts',(7.01618411311258,-3.65514827928551,149.480443038039));
#53314=CARTESIAN_POINT('Ctrl Pts',(6.99059202867877,-3.70385902782594,149.478274479522));
#53315=CARTESIAN_POINT('Ctrl Pts',(6.54989969593821,-4.52181050347926,149.441958188016));
#53316=CARTESIAN_POINT('Ctrl Pts',(6.01072134227546,-5.21718858489354,149.413430129067));
#53317=CARTESIAN_POINT('Ctrl Pts',(5.12109578670382,-6.03920780721774,149.370729971823));
#53318=CARTESIAN_POINT('Ctrl Pts',(4.8590239118827,-6.25200273239228,149.35842271667));
#53319=CARTESIAN_POINT('Ctrl Pts',(4.56763310984833,-6.45918421800138,149.344166651783));
#53320=CARTESIAN_POINT('Ctrl Pts',(4.55104567371395,-6.47088218500881,149.343353632332));
#53321=CARTESIAN_POINT('Ctrl Pts',(4.52866614015609,-6.48653630109342,149.342254904525));
#53322=CARTESIAN_POINT('Ctrl Pts',(4.52291342823913,-6.49054884540434,149.341972313433));
#53323=CARTESIAN_POINT('Ctrl Pts',(4.51343185646688,-6.49714356075586,149.341506294557));
#53324=CARTESIAN_POINT('Ctrl Pts',(4.50970609046465,-6.49973019051875,149.341323108709));
#53325=CARTESIAN_POINT('Ctrl Pts',(4.5024482631929,-6.50475972504361,149.340966138286));
#53326=CARTESIAN_POINT('Ctrl Pts',(4.49891643243196,-6.50720296111665,149.340792371565));
#53327=CARTESIAN_POINT('Ctrl Pts',(4.49070664082053,-6.51287241990594,149.340388320285));
#53328=CARTESIAN_POINT('Ctrl Pts',(4.48602719351208,-6.51609647800787,149.340157921213));
#53329=CARTESIAN_POINT('Ctrl Pts',(4.47150811876265,-6.52607681609769,149.339442765104));
#53330=CARTESIAN_POINT('Ctrl Pts',(4.46165670107198,-6.53281585117169,149.338957109161));
#53331=CARTESIAN_POINT('Ctrl Pts',(4.37845518211635,-6.58945532760305,149.334852206526));
#53332=CARTESIAN_POINT('Ctrl Pts',(4.3042875199556,-6.63813975639834,149.33117194482));
#53333=CARTESIAN_POINT('Ctrl Pts',(3.55990156228777,-7.10904168312127,149.294138814529));
#53334=CARTESIAN_POINT('Ctrl Pts',(2.83065900917638,-7.42959847810138,149.25764977628));
#53335=CARTESIAN_POINT('Ctrl Pts',(1.79917464852797,-7.70864753382524,149.21190284172));
#53336=CARTESIAN_POINT('Ctrl Pts',(1.52883155996935,-7.76678594866081,149.200354022928));
#53337=CARTESIAN_POINT('Ctrl Pts',(1.20689325086633,-7.81855499691087,149.187087081397));
#53338=CARTESIAN_POINT('Ctrl Pts',(1.15772539519168,-7.82598655418925,149.185073798849));
#53339=CARTESIAN_POINT('Ctrl Pts',(1.0927245790804,-7.8351852263697,149.182428498573));
#53340=CARTESIAN_POINT('Ctrl Pts',(1.07695207409938,-7.83736874019975,149.181787877185));
#53341=CARTESIAN_POINT('Ctrl Pts',(1.05110633813079,-7.84086727737101,149.180740152587));
#53342=CARTESIAN_POINT('Ctrl Pts',(1.04103700037219,-7.84221054039673,149.180332470934));
#53343=CARTESIAN_POINT('Ctrl Pts',(1.02159242672985,-7.84476636223987,149.179546174594));
#53344=CARTESIAN_POINT('Ctrl Pts',(1.01221754634572,-7.84598151947403,149.179167506845));
#53345=CARTESIAN_POINT('Ctrl Pts',(0.990768093654178,-7.84872268001833,
149.178302111037));
#53346=CARTESIAN_POINT('Ctrl Pts',(0.978692121403351,-7.85023763053391,
149.177815609775));
#53347=CARTESIAN_POINT('Ctrl Pts',(0.946739072639208,-7.85417131685011,
149.176530207551));
#53348=CARTESIAN_POINT('Ctrl Pts',(0.926856189083176,-7.856542468275,149.175732286614));
#53349=CARTESIAN_POINT('Ctrl Pts',(0.796108832971649,-7.87163162050543,
149.170497814899));
#53350=CARTESIAN_POINT('Ctrl Pts',(0.684993217024253,-7.88207832916265,
149.166108857532));
#53351=CARTESIAN_POINT('Ctrl Pts',(-0.110773817093137,-7.93993829575988,
149.135071931437));
#53352=CARTESIAN_POINT('Ctrl Pts',(-0.798778168017218,-7.90043385837942,
149.110659956625));
#53353=CARTESIAN_POINT('Ctrl Pts',(-1.67121591648593,-7.73509120590145,
149.078380193435));
#53354=CARTESIAN_POINT('Ctrl Pts',(-1.8678623735826,-7.68997300234885,149.070987374967));
#53355=CARTESIAN_POINT('Ctrl Pts',(-2.19260125175708,-7.60227358415099,
149.058337034674));
#53356=CARTESIAN_POINT('Ctrl Pts',(-2.32171639331088,-7.56384126512282,
149.053187411601));
#53357=CARTESIAN_POINT('Ctrl Pts',(-2.51035481665794,-7.50240613140274,
149.045414714383));
#53358=CARTESIAN_POINT('Ctrl Pts',(-2.57068481570564,-7.48194883268298,
149.042890687503));
#53359=CARTESIAN_POINT('Ctrl Pts',(-2.64038896335427,-7.45737027158181,
149.039923838663));
#53360=CARTESIAN_POINT('Ctrl Pts',(-2.65001132706484,-7.45395634614931,
149.039513151579));
#53361=CARTESIAN_POINT('Ctrl Pts',(-2.66463067652972,-7.44873765040983,
149.038887443896));
#53362=CARTESIAN_POINT('Ctrl Pts',(-2.66963252130659,-7.4469464499161,149.038673053767));
#53363=CARTESIAN_POINT('Ctrl Pts',(-2.67830287152923,-7.44383167046296,
149.038300877909));
#53364=CARTESIAN_POINT('Ctrl Pts',(-2.68197221377194,-7.4425104134495,149.038143201375));
#53365=CARTESIAN_POINT('Ctrl Pts',(-2.68959428536389,-7.43975948859834,
149.037815315808));
#53366=CARTESIAN_POINT('Ctrl Pts',(-2.69354685440106,-7.43832938307341,
149.037645086052));
#53367=CARTESIAN_POINT('Ctrl Pts',(-2.70435080962519,-7.4344105908674,149.037179232755));
#53368=CARTESIAN_POINT('Ctrl Pts',(-2.71119988716017,-7.43191558795201,
149.036883306929));
#53369=CARTESIAN_POINT('Ctrl Pts',(-2.73724493449828,-7.42238702341264,
149.035755664892));
#53370=CARTESIAN_POINT('Ctrl Pts',(-2.75641693850311,-7.41528857196749,
149.034920793306));
#53371=CARTESIAN_POINT('Ctrl Pts',(-3.04508196158709,-7.30713591792976,
149.022275242403));
#53372=CARTESIAN_POINT('Ctrl Pts',(-3.30884578878543,-7.19153976667503,
149.009660128665));
#53373=CARTESIAN_POINT('Ctrl Pts',(-3.86645566951851,-6.9099904760934,148.981486276701));
#53374=CARTESIAN_POINT('Ctrl Pts',(-4.15721345301412,-6.73906663907074,
148.965839381709));
#53375=CARTESIAN_POINT('Ctrl Pts',(-4.73443380443059,-6.34813456049918,
148.933790807392));
#53376=CARTESIAN_POINT('Ctrl Pts',(-5.01855674891759,-6.12599355001103,
148.917455432688));
#53377=CARTESIAN_POINT('Ctrl Pts',(-5.48732525513993,-5.70491086492572,
148.890052053284));
#53378=CARTESIAN_POINT('Ctrl Pts',(-5.67873585817106,-5.51441062791798,
148.87870231674));
#53379=CARTESIAN_POINT('Ctrl Pts',(-5.87258067753897,-5.30066648576751,
148.867040919445));
#53380=CARTESIAN_POINT('Ctrl Pts',(-5.88506392404763,-5.28680353557291,
148.866289113506));
#53381=CARTESIAN_POINT('Ctrl Pts',(-5.9029580740366,-5.26678973192563,148.865210207601));
#53382=CARTESIAN_POINT('Ctrl Pts',(-5.90840859524454,-5.26067447922086,
148.864881409969));
#53383=CARTESIAN_POINT('Ctrl Pts',(-5.9178574563556,-5.25004005084794,148.864311126344));
#53384=CARTESIAN_POINT('Ctrl Pts',(-5.9218601373108,-5.24552475197567,148.864069454827));
#53385=CARTESIAN_POINT('Ctrl Pts',(-5.92955015569906,-5.2368298632195,148.863604975457));
#53386=CARTESIAN_POINT('Ctrl Pts',(-5.93323824865338,-5.23265094862386,
148.863382135414));
#53387=CARTESIAN_POINT('Ctrl Pts',(-5.94192081028687,-5.22279190593248,
148.862857336532));
#53388=CARTESIAN_POINT('Ctrl Pts',(-5.94691155969522,-5.21710850088318,
148.86255553614));
#53389=CARTESIAN_POINT('Ctrl Pts',(-5.96415669192368,-5.19741305464539,
148.861512181106));
#53390=CARTESIAN_POINT('Ctrl Pts',(-5.97636980931023,-5.18336487380359,
148.860772379657));
#53391=CARTESIAN_POINT('Ctrl Pts',(-6.11258035280688,-5.02556681007315,
148.852511257575));
#53392=CARTESIAN_POINT('Ctrl Pts',(-6.23141876092967,-4.87743648363437,
148.845210307832));
#53393=CARTESIAN_POINT('Ctrl Pts',(-6.82841010841845,-4.07581369218198,
148.80781868917));
#53394=CARTESIAN_POINT('Ctrl Pts',(-7.20939802013467,-3.35617009044395,
148.781955481912));
#53395=CARTESIAN_POINT('Ctrl Pts',(-7.52538137031228,-2.44471253632168,
148.748089365807));
#53396=CARTESIAN_POINT('Ctrl Pts',(-7.57186897398844,-2.29668917125152,
148.742536570122));
#53397=CARTESIAN_POINT('Ctrl Pts',(-7.65651502922844,-1.99656218909036,
148.731010833574));
#53398=CARTESIAN_POINT('Ctrl Pts',(-7.6945625978662,-1.84450104108649,148.725036573261));
#53399=CARTESIAN_POINT('Ctrl Pts',(-7.73296796118194,-1.66902753348587,
148.717890519831));
#53400=CARTESIAN_POINT('Ctrl Pts',(-7.73777133156448,-1.6466150721659,148.71697311198));
#53401=CARTESIAN_POINT('Ctrl Pts',(-7.74373287222399,-1.61819640680624,
148.715803593481));
#53402=CARTESIAN_POINT('Ctrl Pts',(-7.74498161522343,-1.61220910145263,
148.715556845351));
#53403=CARTESIAN_POINT('Ctrl Pts',(-7.74696355560872,-1.60265091548136,
148.715162365469));
#53404=CARTESIAN_POINT('Ctrl Pts',(-7.74770123292901,-1.59908095295293,
148.715014901369));
#53405=CARTESIAN_POINT('Ctrl Pts',(-7.74909482285481,-1.59231312339752,
148.714735101477));
#53406=CARTESIAN_POINT('Ctrl Pts',(-7.74975122237288,-1.58911536642455,
148.714602795706));
#53407=CARTESIAN_POINT('Ctrl Pts',(-7.75123785439433,-1.58185016926167,
148.714301971123));
#53408=CARTESIAN_POINT('Ctrl Pts',(-7.75206686439499,-1.57778248286342,
148.714133379559));
#53409=CARTESIAN_POINT('Ctrl Pts',(-7.75419679564904,-1.56728939020988,
148.713698058049));
#53410=CARTESIAN_POINT('Ctrl Pts',(-7.75549292983254,-1.56086302830029,
148.713431045785));
#53411=CARTESIAN_POINT('Ctrl Pts',(-7.76309063535863,-1.52294974451091,
148.711853411207));
#53412=CARTESIAN_POINT('Ctrl Pts',(-7.76920835339804,-1.49142671345929,
148.710532105867));
#53413=CARTESIAN_POINT('Ctrl Pts',(-7.86559670462253,-0.978070393359079,
148.68886949681));
#53414=CARTESIAN_POINT('Ctrl Pts',(-7.91107393500614,-0.488943892504856,
148.666215133163));
#53415=CARTESIAN_POINT('Ctrl Pts',(-7.91093589495348,0.425052308809872,
148.623880575233));
#53416=CARTESIAN_POINT('Ctrl Pts',(-7.87680757959934,0.848248594413475,
148.604279788228));
#53417=CARTESIAN_POINT('Ctrl Pts',(-7.7569377716937,1.58722450434003,148.571244463978));
#53418=CARTESIAN_POINT('Ctrl Pts',(-7.68525539490773,1.90427112437255,148.557459048505));
#53419=CARTESIAN_POINT('Ctrl Pts',(-7.58820368100426,2.23686305051484,148.543448480544));
#53420=CARTESIAN_POINT('Ctrl Pts',(-7.58204250288556,2.25765872214134,148.542574280886));
#53421=CARTESIAN_POINT('Ctrl Pts',(-7.57348107557444,2.28612554211239,148.541380070242));
#53422=CARTESIAN_POINT('Ctrl Pts',(-7.57115457153753,2.29381866126426,148.541057583723));
#53423=CARTESIAN_POINT('Ctrl Pts',(-7.56716680123419,2.30693297498313,148.540508266147));
#53424=CARTESIAN_POINT('Ctrl Pts',(-7.56551142538087,2.31235594608302,148.540281237192));
#53425=CARTESIAN_POINT('Ctrl Pts',(-7.56229197485612,2.32286232356471,148.53984163091));
#53426=CARTESIAN_POINT('Ctrl Pts',(-7.5607286013615,2.32794594093536,148.539629030122));
#53427=CARTESIAN_POINT('Ctrl Pts',(-7.55699694123851,2.34003675874718,148.53912363663));
#53428=CARTESIAN_POINT('Ctrl Pts',(-7.55482403161433,2.34704253346622,148.538830999776));
#53429=CARTESIAN_POINT('Ctrl Pts',(-7.5483529058202,2.36780428034962,148.537964362653));
#53430=CARTESIAN_POINT('Ctrl Pts',(-7.54402682916036,2.38155157505634,148.537391301631));
#53431=CARTESIAN_POINT('Ctrl Pts',(-7.50920547116318,2.49115902882886,148.532828401821));
#53432=CARTESIAN_POINT('Ctrl Pts',(-7.47692126107482,2.58644341140148,148.528899384002));
#53433=CARTESIAN_POINT('Ctrl Pts',(-7.33268651360203,2.98684584932947,148.512527032226));
#53434=CARTESIAN_POINT('Ctrl Pts',(-7.20380449674291,3.28553850822161,148.500673940781));
#53435=CARTESIAN_POINT('Ctrl Pts',(-6.70204633541516,4.27585771948024,148.461510065733));
#53436=CARTESIAN_POINT('Ctrl Pts',(-6.24497034089314,4.91938564427989,148.436653689384));
#53437=CARTESIAN_POINT('Ctrl Pts',(-5.65356205128053,5.53405737612092,148.403595439074));
#53438=CARTESIAN_POINT('Ctrl Pts',(-5.60573459863632,5.5824989044821,148.400913884116));
#53439=CARTESIAN_POINT('Ctrl Pts',(-5.55067177066127,5.63684755417532,148.397809194485));
#53440=CARTESIAN_POINT('Ctrl Pts',(-5.54404276132924,5.64336755084235,148.397435138008));
#53441=CARTESIAN_POINT('Ctrl Pts',(-5.53431024558022,5.65290631890934,148.396885517534));
#53442=CARTESIAN_POINT('Ctrl Pts',(-5.53121571243371,5.65593427181423,148.396710696015));
#53443=CARTESIAN_POINT('Ctrl Pts',(-5.52569713149072,5.66132525748214,148.396398817837));
#53444=CARTESIAN_POINT('Ctrl Pts',(-5.52327404732735,5.66368927979123,148.396261840331));
#53445=CARTESIAN_POINT('Ctrl Pts',(-5.51820917972769,5.66862435147306,148.395975442637));
#53446=CARTESIAN_POINT('Ctrl Pts',(-5.51556711573298,5.67119511047733,148.395825999512));
#53447=CARTESIAN_POINT('Ctrl Pts',(-5.50868893813668,5.67787830440986,148.395436834124));
#53448=CARTESIAN_POINT('Ctrl Pts',(-5.50445002258888,5.68198783924278,148.395196884271));
#53449=CARTESIAN_POINT('Ctrl Pts',(-5.4862551480414,5.69958789862072,148.394166469421));
#53450=CARTESIAN_POINT('Ctrl Pts',(-5.47225426820697,5.71303167987043,148.393372390894));
#53451=CARTESIAN_POINT('Ctrl Pts',(-5.37372892377484,5.80694220330205,148.38777712729));
#53452=CARTESIAN_POINT('Ctrl Pts',(-5.28748588964605,5.88557821216553,148.382842150047));
#53453=CARTESIAN_POINT('Ctrl Pts',(-5.02569905531426,6.11387547205516,148.367840939935));
#53454=CARTESIAN_POINT('Ctrl Pts',(-4.84532029472162,6.25779389824532,148.357479564097));
#53455=CARTESIAN_POINT('Ctrl Pts',(-4.51317490384423,6.49982270225128,148.338721787915));
#53456=CARTESIAN_POINT('Ctrl Pts',(-4.3638394159758,6.60101105854147,148.330394439908));
#53457=CARTESIAN_POINT('Ctrl Pts',(-3.99678933189694,6.83181768334312,148.310369481882));
#53458=CARTESIAN_POINT('Ctrl Pts',(-3.77604505833299,6.95625960055671,148.298685325143));
#53459=CARTESIAN_POINT('Ctrl Pts',(-3.13138256934769,7.27993647787237,148.266008709818));
#53460=CARTESIAN_POINT('Ctrl Pts',(-2.69520571836805,7.45244887556802,148.245652454536));
#53461=CARTESIAN_POINT('Ctrl Pts',(-2.21544924007381,7.5945203667391,148.225323931461));
#53462=CARTESIAN_POINT('Ctrl Pts',(-2.18456222137497,7.60346255785421,148.224023610946));
#53463=CARTESIAN_POINT('Ctrl Pts',(-2.14326201593034,7.61514706591514,148.222296023244));
#53464=CARTESIAN_POINT('Ctrl Pts',(-2.13289673298962,7.61805673594162,148.221863375489));
#53465=CARTESIAN_POINT('Ctrl Pts',(-2.1167084924406,7.62256535692265,148.221189124472));
#53466=CARTESIAN_POINT('Ctrl Pts',(-2.11088960744574,7.62417881006936,148.220947055588));
#53467=CARTESIAN_POINT('Ctrl Pts',(-2.09976769885941,7.62724897028517,148.22048493337));
#53468=CARTESIAN_POINT('Ctrl Pts',(-2.09446499397367,7.62870681262968,148.220264843717));
#53469=CARTESIAN_POINT('Ctrl Pts',(-2.0820826234574,7.63209714332255,148.21975147245));
#53470=CARTESIAN_POINT('Ctrl Pts',(-2.07500177507332,7.63402531367505,148.219458329397));
#53471=CARTESIAN_POINT('Ctrl Pts',(-2.05478149625032,7.6395012424466,148.218622438149));
#53472=CARTESIAN_POINT('Ctrl Pts',(-2.041635550892,7.64302495811424,148.218080459983));
#53473=CARTESIAN_POINT('Ctrl Pts',(-1.95842877204707,7.66509819500693,148.214659227505));
#53474=CARTESIAN_POINT('Ctrl Pts',(-1.8881238719227,7.68271841106502,148.211809741363));
#53475=CARTESIAN_POINT('Ctrl Pts',(-1.68022062607629,7.73179800094543,148.203498978231));
#53476=CARTESIAN_POINT('Ctrl Pts',(-1.54200906600314,7.76054456982866,148.198122883539));
#53477=CARTESIAN_POINT('Ctrl Pts',(-1.23306479534329,7.81622175431553,148.186389871754));
#53478=CARTESIAN_POINT('Ctrl Pts',(-1.06206930170562,7.84128709913149,148.180086778253));
#53479=CARTESIAN_POINT('Ctrl Pts',(-0.476144606609255,7.90765478760128,
148.158954792078));
#53480=CARTESIAN_POINT('Ctrl Pts',(-0.0588370628559313,7.92175856032181,
148.144730754861));
#53481=CARTESIAN_POINT('Ctrl Pts',(0.735032008694882,7.8858337137424,148.117062605254));
#53482=CARTESIAN_POINT('Ctrl Pts',(1.11069911345139,7.84174395717142,148.103689703025));
#53483=CARTESIAN_POINT('Ctrl Pts',(1.55427855291734,7.7571638969136,148.086202855121));
#53484=CARTESIAN_POINT('Ctrl Pts',(1.62661389690692,7.74231878523468,148.083295804598));
#53485=CARTESIAN_POINT('Ctrl Pts',(1.70823157896408,7.72437444331806,148.079942501642));
#53486=CARTESIAN_POINT('Ctrl Pts',(1.71773046271818,7.72226765425011,148.079551108575));
#53487=CARTESIAN_POINT('Ctrl Pts',(1.73168680785101,7.71914520526742,148.078974362287));
#53488=CARTESIAN_POINT('Ctrl Pts',(1.73614734377517,7.71814318997965,148.078789776964));
#53489=CARTESIAN_POINT('Ctrl Pts',(1.74400705435517,7.71637042545534,148.078464076634));
#53490=CARTESIAN_POINT('Ctrl Pts',(1.74740659828806,7.71560129404987,148.078323053398));
#53491=CARTESIAN_POINT('Ctrl Pts',(1.75445713929826,7.71400124232155,148.078030265659));
#53492=CARTESIAN_POINT('Ctrl Pts',(1.75810804766525,7.71316997821378,148.07787848205));
#53493=CARTESIAN_POINT('Ctrl Pts',(1.76753288105133,7.71101702757333,148.077486209544));
#53494=CARTESIAN_POINT('Ctrl Pts',(1.77330590570613,7.7096914496989,148.077245500539));
#53495=CARTESIAN_POINT('Ctrl Pts',(1.79745332059851,7.70411826370192,148.076236883664));
#53496=CARTESIAN_POINT('Ctrl Pts',(1.81581385241687,7.69981147191977,148.07546566866));
#53497=CARTESIAN_POINT('Ctrl Pts',(1.94134500849951,7.6698919241853,148.070164204104));
#53498=CARTESIAN_POINT('Ctrl Pts',(2.04798171734216,7.6421091002705,148.065517679895));
#53499=CARTESIAN_POINT('Ctrl Pts',(2.37634494483499,7.54919214675338,148.050840980337));
#53500=CARTESIAN_POINT('Ctrl Pts',(2.59581708914995,7.47656606828914,148.040506954937));
#53501=CARTESIAN_POINT('Ctrl Pts',(3.00309594389115,7.32169573966932,148.020715655174));
#53502=CARTESIAN_POINT('Ctrl Pts',(3.19151137379599,7.24155144687217,148.011300062701));
#53503=CARTESIAN_POINT('Ctrl Pts',(3.97025895759536,6.87400152092731,147.971759281154));
#53504=CARTESIAN_POINT('Ctrl Pts',(4.52682266400117,6.52096542962951,147.942234803954));
#53505=CARTESIAN_POINT('Ctrl Pts',(5.06692873406214,6.07552805960929,147.913677337722));
#53506=CARTESIAN_POINT('Ctrl Pts',(5.10021357258826,6.04761354511706,147.911916459809));
#53507=CARTESIAN_POINT('Ctrl Pts',(5.14230412986137,6.01171941248033,147.909688236262));
#53508=CARTESIAN_POINT('Ctrl Pts',(5.15132376493752,6.00399246574771,147.909210658862));
#53509=CARTESIAN_POINT('Ctrl Pts',(5.16558309384168,5.99172098869538,147.908455498405));
#53510=CARTESIAN_POINT('Ctrl Pts',(5.17083425372177,5.98718984387565,147.908177369966));
#53511=CARTESIAN_POINT('Ctrl Pts',(5.18023445451904,5.97905696435531,147.907679427706));
#53512=CARTESIAN_POINT('Ctrl Pts',(5.18438571180846,5.97545780490032,147.907459508813));
#53513=CARTESIAN_POINT('Ctrl Pts',(5.19389305945674,5.9671975248454,147.906955794362));
#53514=CARTESIAN_POINT('Ctrl Pts',(5.19924663440435,5.96253350921946,147.906672117775));
#53515=CARTESIAN_POINT('Ctrl Pts',(5.21402073154748,5.94962734041811,147.905889162303));
#53516=CARTESIAN_POINT('Ctrl Pts',(5.22342800055496,5.9413700106717,147.905390507995));
#53517=CARTESIAN_POINT('Ctrl Pts',(5.27408649890585,5.89669066699126,147.902704578308));
#53518=CARTESIAN_POINT('Ctrl Pts',(5.31497691309309,5.85986090164036,147.900534211307));
#53519=CARTESIAN_POINT('Ctrl Pts',(5.50949302237821,5.68095011801749,147.890195000266));
#53520=CARTESIAN_POINT('Ctrl Pts',(5.65782993461925,5.53323372354095,147.882268622808));
#53521=CARTESIAN_POINT('Ctrl Pts',(5.93530290248307,5.23408096556415,147.867232290146));
#53522=CARTESIAN_POINT('Ctrl Pts',(6.06492732134635,5.0833143860368,147.860106424396));
#53523=CARTESIAN_POINT('Ctrl Pts',(6.67884158402428,4.31231332320873,147.825399965357));
#53524=CARTESIAN_POINT('Ctrl Pts',(7.07429577031348,3.62724800941383,147.800275370008));
#53525=CARTESIAN_POINT('Ctrl Pts',(7.37841773920854,2.85391773125621,147.767636923401));
#53526=CARTESIAN_POINT('Ctrl Pts',(7.39432821852242,2.81243752069445,147.765873028821));
#53527=CARTESIAN_POINT('Ctrl Pts',(7.41250649815316,2.76382421632936,147.763788098943));
#53528=CARTESIAN_POINT('Ctrl Pts',(7.41511487590344,2.7568185033495,147.763487209687));
#53529=CARTESIAN_POINT('Ctrl Pts',(7.41926068415732,2.7456350300021,147.763006191873));
#53530=CARTESIAN_POINT('Ctrl Pts',(7.42080452973278,2.74145963836216,147.762826447147));
#53531=CARTESIAN_POINT('Ctrl Pts',(7.42352272867965,2.73408904120906,147.762508876492));
#53532=CARTESIAN_POINT('Ctrl Pts',(7.4246985467434,2.73089437335107,147.762371138848));
#53533=CARTESIAN_POINT('Ctrl Pts',(7.42712466168525,2.72428953166578,147.762086180699));
#53534=CARTESIAN_POINT('Ctrl Pts',(7.42837467252755,2.72087925439996,147.761938942919));
#53535=CARTESIAN_POINT('Ctrl Pts',(7.43157261749131,2.7121359969833,147.761561182414));
#53536=CARTESIAN_POINT('Ctrl Pts',(7.43351714388872,2.70680182250626,147.761330453496));
#53537=CARTESIAN_POINT('Ctrl Pts',(7.44166003651497,2.6843894991263,147.760359916198));
#53538=CARTESIAN_POINT('Ctrl Pts',(7.44780524813394,2.66729227073327,147.759616881641));
#53539=CARTESIAN_POINT('Ctrl Pts',(7.48959725703416,2.54974788335504,147.754491039096));
#53540=CARTESIAN_POINT('Ctrl Pts',(7.52326840734035,2.44861428859249,147.74999360827));
#53541=CARTESIAN_POINT('Ctrl Pts',(7.60155984612015,2.19658012052913,147.738628709491));
#53542=CARTESIAN_POINT('Ctrl Pts',(7.64374011171562,2.0449716652365,147.731655458579));
#53543=CARTESIAN_POINT('Ctrl Pts',(7.76157322352243,1.56663259911239,147.709447980611));
#53544=CARTESIAN_POINT('Ctrl Pts',(7.82099366487555,1.23628781987725,147.693828965333));
#53545=CARTESIAN_POINT('Ctrl Pts',(7.89522874391354,0.59030802259276,147.663789306108));
#53546=CARTESIAN_POINT('Ctrl Pts',(7.91247045273205,0.275557006149398,147.649380083742));
#53547=CARTESIAN_POINT('Ctrl Pts',(7.9092144286864,-0.378229125280889,147.620444312156));
#53548=CARTESIAN_POINT('Ctrl Pts',(7.88576056627405,-0.716623088197248,
147.606025698784));
#53549=CARTESIAN_POINT('Ctrl Pts',(7.83768124596388,-1.07479278363729,147.591407139106));
#53550=CARTESIAN_POINT('Ctrl Pts',(7.83459392930034,-1.09707101651083,147.59050043064));
#53551=CARTESIAN_POINT('Ctrl Pts',(7.8301540947938,-1.12813423125074,147.589239721103));
#53552=CARTESIAN_POINT('Ctrl Pts',(7.82888173003655,-1.1369304506973,147.588883120565));
#53553=CARTESIAN_POINT('Ctrl Pts',(7.82671450949683,-1.15173691008189,147.588283527779));
#53554=CARTESIAN_POINT('Ctrl Pts',(7.82582754914811,-1.157748286295,147.588040279396));
#53555=CARTESIAN_POINT('Ctrl Pts',(7.82414827562132,-1.16903946253727,147.587583730715));
#53556=CARTESIAN_POINT('Ctrl Pts',(7.82335754226196,-1.17431949228743,147.587370379235));
#53557=CARTESIAN_POINT('Ctrl Pts',(7.8213904782326,-1.18736416498312,147.586843629098));
#53558=CARTESIAN_POINT('Ctrl Pts',(7.82020792834831,-1.19512787229747,147.58653043271));
#53559=CARTESIAN_POINT('Ctrl Pts',(7.81642429181523,-1.21972223316322,147.585539233222));
#53560=CARTESIAN_POINT('Ctrl Pts',(7.8137804082903,-1.23654630788361,147.584862621857));
#53561=CARTESIAN_POINT('Ctrl Pts',(7.77114370386214,-1.50226272561509,147.574198662081));
#53562=CARTESIAN_POINT('Ctrl Pts',(7.71932980497701,-1.74912225790972,147.564608268771));
#53563=CARTESIAN_POINT('Ctrl Pts',(7.60590931723317,-2.18478797513713,147.548059670667));
#53564=CARTESIAN_POINT('Ctrl Pts',(7.54882322874031,-2.37453730989995,147.540982091399));
#53565=CARTESIAN_POINT('Ctrl Pts',(7.23103272131675,-3.30295453489013,147.506561783295));
#53566=CARTESIAN_POINT('Ctrl Pts',(6.86881183373858,-4.00204502466144,147.481725711336));
#53567=CARTESIAN_POINT('Ctrl Pts',(6.38391620959262,-4.67241978700235,147.449232658954));
#53568=CARTESIAN_POINT('Ctrl Pts',(6.35758932760608,-4.70817912079544,147.447469099326));
#53569=CARTESIAN_POINT('Ctrl Pts',(6.32657649121231,-4.74956886688329,147.445389947481));
#53570=CARTESIAN_POINT('Ctrl Pts',(6.3221815948993,-4.75541737399408,147.445095267313));
#53571=CARTESIAN_POINT('Ctrl Pts',(6.31517026032976,-4.76472080665741,147.444625076769));
#53572=CARTESIAN_POINT('Ctrl Pts',(6.3125590766239,-4.7681797036503,147.444449950009));
#53573=CARTESIAN_POINT('Ctrl Pts',(6.30795409088466,-4.77426927215136,147.444141069909));
#53574=CARTESIAN_POINT('Ctrl Pts',(6.30596148009766,-4.77690084753458,147.444007404356));
#53575=CARTESIAN_POINT('Ctrl Pts',(6.30184049943086,-4.78233621894065,147.443730942207));
#53576=CARTESIAN_POINT('Ctrl Pts',(6.29971191243885,-4.78513983195751,147.443588129163));
#53577=CARTESIAN_POINT('Ctrl Pts',(6.29422240281678,-4.79236018547139,147.443219788102));
#53578=CARTESIAN_POINT('Ctrl Pts',(6.29085870929139,-4.79677480218072,147.442994054876));
#53579=CARTESIAN_POINT('Ctrl Pts',(6.276840136198,-4.81513310906028,147.442053164647));
#53580=CARTESIAN_POINT('Ctrl Pts',(6.26614359551777,-4.82904476932111,147.441334949204));
#53581=CARTESIAN_POINT('Ctrl Pts',(6.193410077902,-4.92299165604127,147.43645001041));
#53582=CARTESIAN_POINT('Ctrl Pts',(6.12988999094503,-5.00186188030843,147.432177682796));
#53583=CARTESIAN_POINT('Ctrl Pts',(5.91657821073534,-5.25655479407876,147.417874033677));
#53584=CARTESIAN_POINT('Ctrl Pts',(5.76060524623282,-5.42703237305624,147.407484983798));
#53585=CARTESIAN_POINT('Ctrl Pts',(5.54919254572091,-5.63870895343066,147.393762502684));
#53586=CARTESIAN_POINT('Ctrl Pts',(5.50035341283223,-5.68635988328701,147.390615354296));
#53587=CARTESIAN_POINT('Ctrl Pts',(5.32411781332532,-5.85391282173301,147.379356838872));
#53588=CARTESIAN_POINT('Ctrl Pts',(5.19336853283439,-5.97021341680011,147.371183686555));
#53589=CARTESIAN_POINT('Ctrl Pts',(5.00465278059966,-6.12718084850084,147.359731545663));
#53590=CARTESIAN_POINT('Ctrl Pts',(4.94983235730225,-6.17155201717955,147.356443402943));
#53591=CARTESIAN_POINT('Ctrl Pts',(4.8736582885577,-6.23153870574493,147.351932371006));
#53592=CARTESIAN_POINT('Ctrl Pts',(4.85280886932392,-6.24778887592645,147.350703517767));
#53593=CARTESIAN_POINT('Ctrl Pts',(4.81198468946208,-6.27927986264132,147.34830910058));
#53594=CARTESIAN_POINT('Ctrl Pts',(4.79201798958187,-6.29453062890741,147.347143430159));
#53595=CARTESIAN_POINT('Ctrl Pts',(4.75288503744982,-6.32412665342139,147.344869660389));
#53596=CARTESIAN_POINT('Ctrl Pts',(4.73372564642155,-6.33848054488581,147.343761450202));
#53597=CARTESIAN_POINT('Ctrl Pts',(4.48495464062853,-6.52309850461027,147.329438551072));
#53598=CARTESIAN_POINT('Ctrl Pts',(4.24633270470723,-6.68089129609932,147.316440460884));
#53599=CARTESIAN_POINT('Ctrl Pts',(3.73613054745982,-6.97986812395028,147.29042433546));
#53600=CARTESIAN_POINT('Ctrl Pts',(3.46384239562063,-7.11892229455873,147.277490153354));
#53601=CARTESIAN_POINT('Ctrl Pts',(3.16487452184701,-7.25037478776653,147.264274917261));
#53602=CARTESIAN_POINT('Ctrl Pts',(3.14554492703048,-7.25878174512276,147.263424697256));
#53603=CARTESIAN_POINT('Ctrl Pts',(3.11885391029224,-7.27026374504147,147.262256423046));
#53604=CARTESIAN_POINT('Ctrl Pts',(3.11152118116277,-7.27340501937474,147.261936062603));
#53605=CARTESIAN_POINT('Ctrl Pts',(3.09895698223819,-7.27876493043158,147.261388159598));
#53606=CARTESIAN_POINT('Ctrl Pts',(3.09372785711837,-7.2809890287324,147.26116042728));
#53607=CARTESIAN_POINT('Ctrl Pts',(3.08310830553083,-7.28549232568808,147.260698546738));
#53608=CARTESIAN_POINT('Ctrl Pts',(3.07771773660136,-7.28777118090987,147.260464410526));
#53609=CARTESIAN_POINT('Ctrl Pts',(3.06533775182537,-7.29298861607669,147.259927421016));
#53610=CARTESIAN_POINT('Ctrl Pts',(3.05834662524347,-7.29592313605843,147.259624708525));
#53611=CARTESIAN_POINT('Ctrl Pts',(3.04367927068535,-7.30205496035293,147.258990729963));
#53612=CARTESIAN_POINT('Ctrl Pts',(3.03600219619126,-7.30525022241433,147.258659534704));
#53613=CARTESIAN_POINT('Ctrl Pts',(3.01571643378002,-7.31365582434048,147.257786064805));
#53614=CARTESIAN_POINT('Ctrl Pts',(3.00309925598472,-7.31884567312467,147.257244496669));
#53615=CARTESIAN_POINT('Ctrl Pts',(2.96527250767284,-7.33429073886641,147.255625925291));
#53616=CARTESIAN_POINT('Ctrl Pts',(2.94002326199174,-7.34444857868534,147.254552262836));
#53617=CARTESIAN_POINT('Ctrl Pts',(2.6600979644896,-7.45538842083882,147.242722330809));
#53618=CARTESIAN_POINT('Ctrl Pts',(2.40039556468224,-7.54301364581422,147.232425205799));
#53619=CARTESIAN_POINT('Ctrl Pts',(1.42740195179222,-7.81594948556875,147.195696820419));
#53620=CARTESIAN_POINT('Ctrl Pts',(0.693926166972634,-7.91484995316757,
147.171898875596));
#53621=CARTESIAN_POINT('Ctrl Pts',(-0.264972799758299,-7.90968828836991,
147.136974349162));
#53622=CARTESIAN_POINT('Ctrl Pts',(-0.487210570889519,-7.89911433551051,
147.128575362273));
#53623=CARTESIAN_POINT('Ctrl Pts',(-0.724442810736541,-7.87777589374369,
147.119054345134));
#53624=CARTESIAN_POINT('Ctrl Pts',(-0.74016792610319,-7.87631397633031,
147.118420850828));
#53625=CARTESIAN_POINT('Ctrl Pts',(-0.761746669491083,-7.87424267128036,
147.117548353959));
#53626=CARTESIAN_POINT('Ctrl Pts',(-0.767604227070623,-7.87367381753953,
147.117311191943));
#53627=CARTESIAN_POINT('Ctrl Pts',(-0.777603765633786,-7.87269145278235,
147.116905783793));
#53628=CARTESIAN_POINT('Ctrl Pts',(-0.781746070554488,-7.87228120738246,
147.116737683986));
#53629=CARTESIAN_POINT('Ctrl Pts',(-0.789781156683354,-7.87147902442379,
147.116411302963));
#53630=CARTESIAN_POINT('Ctrl Pts',(-0.793673975944867,-7.87108746789276,
147.116253038673));
#53631=CARTESIAN_POINT('Ctrl Pts',(-0.802947350066434,-7.87014776252027,
147.115875694367));
#53632=CARTESIAN_POINT('Ctrl Pts',(-0.808327632158715,-7.86959698394783,
147.115656498815));
#53633=CARTESIAN_POINT('Ctrl Pts',(-0.824319029222221,-7.86794337487276,
147.115004218826));
#53634=CARTESIAN_POINT('Ctrl Pts',(-0.834928455343997,-7.86682459986257,
147.114570442701));
#53635=CARTESIAN_POINT('Ctrl Pts',(-0.921199569797452,-7.8575507349788,
147.111035004269));
#53636=CARTESIAN_POINT('Ctrl Pts',(-0.996740622014635,-7.84832592380449,
147.107888225247));
#53637=CARTESIAN_POINT('Ctrl Pts',(-1.43099667393972,-7.78892552127458,
147.089544810863));
#53638=CARTESIAN_POINT('Ctrl Pts',(-1.78604880867886,-7.71525236003017,
147.07356676));
#53639=CARTESIAN_POINT('Ctrl Pts',(-2.66287500766157,-7.46952472933315,
147.033189570492));
#53640=CARTESIAN_POINT('Ctrl Pts',(-3.17418813919936,-7.2670020763461,147.008886879855));
#53641=CARTESIAN_POINT('Ctrl Pts',(-3.84058693153651,-6.91918351647105,
146.977280065042));
#53642=CARTESIAN_POINT('Ctrl Pts',(-4.01703621966544,-6.81825740125398,
146.968900633639));
#53643=CARTESIAN_POINT('Ctrl Pts',(-4.19558481845984,-6.70679073930889,
146.960388728017));
#53644=CARTESIAN_POINT('Ctrl Pts',(-4.20175438767153,-6.70292727513101,
146.960094562339));
#53645=CARTESIAN_POINT('Ctrl Pts',(-4.21498684211986,-6.69461549249407,
146.959463536559));
#53646=CARTESIAN_POINT('Ctrl Pts',(-4.2220480396606,-6.69016449893049,146.959126742113));
#53647=CARTESIAN_POINT('Ctrl Pts',(-4.23708962740804,-6.68064980496048,
146.958409172855));
#53648=CARTESIAN_POINT('Ctrl Pts',(-4.24506801686404,-6.67558296030649,
146.958028475205));
#53649=CARTESIAN_POINT('Ctrl Pts',(-4.26377629368547,-6.66365477235136,
146.957135584038));
#53650=CARTESIAN_POINT('Ctrl Pts',(-4.27449873902532,-6.65678178544482,
146.956623674359));
#53651=CARTESIAN_POINT('Ctrl Pts',(-4.29318247822905,-6.64474192768985,
146.955731381361));
#53652=CARTESIAN_POINT('Ctrl Pts',(-4.30115114796233,-6.63958657446708,
146.955350721343));
#53653=CARTESIAN_POINT('Ctrl Pts',(-4.31738675145416,-6.62904141108799,
146.954574951285));
#53654=CARTESIAN_POINT('Ctrl Pts',(-4.32565291784011,-6.62365044567749,
146.954179870141));
#53655=CARTESIAN_POINT('Ctrl Pts',(-4.34611076008194,-6.61025377639325,
146.953201820104));
#53656=CARTESIAN_POINT('Ctrl Pts',(-4.35829043946903,-6.6022297880615,146.95261929647));
#53657=CARTESIAN_POINT('Ctrl Pts',(-4.40346132160714,-6.5722916878667,146.95045798881));
#53658=CARTESIAN_POINT('Ctrl Pts',(-4.43631017106618,-6.550163490004,146.948884477606));
#53659=CARTESIAN_POINT('Ctrl Pts',(-4.62718926098445,-6.41948570479533,
146.939729903226));
#53660=CARTESIAN_POINT('Ctrl Pts',(-4.78140126280387,-6.30546455737791,
146.932291023522));
#53661=CARTESIAN_POINT('Ctrl Pts',(-5.06869271538402,-6.07644120466206,
146.918290195343));
#53662=CARTESIAN_POINT('Ctrl Pts',(-5.20237889813908,-5.96238542035076,
146.911710599816));
#53663=CARTESIAN_POINT('Ctrl Pts',(-5.88333562283849,-5.34106642573863,
146.877621751639));
#53664=CARTESIAN_POINT('Ctrl Pts',(-6.36052460095868,-4.76278422421943,
146.852072947798));
#53665=CARTESIAN_POINT('Ctrl Pts',(-6.78023025731822,-4.07625361827561,
146.820500614373));
#53666=CARTESIAN_POINT('Ctrl Pts',(-6.81028555485571,-4.02583858606354,
146.81817346005));
#53667=CARTESIAN_POINT('Ctrl Pts',(-6.84463846831642,-3.96672898766845,
146.815430105813));
#53668=CARTESIAN_POINT('Ctrl Pts',(-6.84948503047238,-3.95835438531086,
146.81504108488));
#53669=CARTESIAN_POINT('Ctrl Pts',(-6.85718233882849,-3.94499737935321,
146.814420040561));
#53670=CARTESIAN_POINT('Ctrl Pts',(-6.86004305727132,-3.94002071100837,
146.814188518869));
#53671=CARTESIAN_POINT('Ctrl Pts',(-6.86507621408844,-3.93124264640356,
146.813779919009));
#53672=CARTESIAN_POINT('Ctrl Pts',(-6.86725092026755,-3.92744254803497,
146.813602956217));
#53673=CARTESIAN_POINT('Ctrl Pts',(-6.87173428210063,-3.91959317821807,
146.813237265763));
#53674=CARTESIAN_POINT('Ctrl Pts',(-6.87404251554839,-3.9155436686142,146.813048516586));
#53675=CARTESIAN_POINT('Ctrl Pts',(-6.87992867086586,-3.90519589183057,
146.812565971342));
#53676=CARTESIAN_POINT('Ctrl Pts',(-6.88350151840562,-3.8988947556134,146.812271913319));
#53677=CARTESIAN_POINT('Ctrl Pts',(-6.89792215031076,-3.87338067076191,
146.811080319352));
#53678=CARTESIAN_POINT('Ctrl Pts',(-6.90869811204368,-3.85412742309881,
146.810179027823));
#53679=CARTESIAN_POINT('Ctrl Pts',(-6.97608728616633,-3.73253343833869,
146.804472300182));
#53680=CARTESIAN_POINT('Ctrl Pts',(-7.03049932969253,-3.62900455969918,
146.799539917991));
#53681=CARTESIAN_POINT('Ctrl Pts',(-7.15093558249259,-3.3869713512484,146.787888806798));
#53682=CARTESIAN_POINT('Ctrl Pts',(-7.21526556239071,-3.24767512257988,
146.781099554338));
#53683=CARTESIAN_POINT('Ctrl Pts',(-7.65056755156856,-2.22822051914534,
146.731257767539));
#53684=CARTESIAN_POINT('Ctrl Pts',(-7.8635908985282,-1.28879029546252,146.68576265606));
#53685=CARTESIAN_POINT('Ctrl Pts',(-7.90557380768858,-0.295490631218893,
146.645226367397));
#53686=CARTESIAN_POINT('Ctrl Pts',(-7.90692190982321,-0.256900584353839,
146.643660990879));
#53687=CARTESIAN_POINT('Ctrl Pts',(-7.90831138068428,-0.206566981904476,
146.641631442917));
#53688=CARTESIAN_POINT('Ctrl Pts',(-7.90860920427075,-0.194831382413272,
146.641159104917));
#53689=CARTESIAN_POINT('Ctrl Pts',(-7.90905439448839,-0.175601179965185,
146.640386530699));
#53690=CARTESIAN_POINT('Ctrl Pts',(-7.90921723276855,-0.168106973880743,
146.640085801187));
#53691=CARTESIAN_POINT('Ctrl Pts',(-7.9094843670096,-0.15495193955771,146.639558525692));
#53692=CARTESIAN_POINT('Ctrl Pts',(-7.90959323787568,-0.149291215646896,
146.639331833835));
#53693=CARTESIAN_POINT('Ctrl Pts',(-7.90979661746725,-0.138091141967158,
146.638883704002));
#53694=CARTESIAN_POINT('Ctrl Pts',(-7.90989138443403,-0.132551800467134,
146.638662257907));
#53695=CARTESIAN_POINT('Ctrl Pts',(-7.91008347407537,-0.120588985773937,
146.638184430707));
#53696=CARTESIAN_POINT('Ctrl Pts',(-7.91017879149016,-0.114165481847901,
146.637928113781));
#53697=CARTESIAN_POINT('Ctrl Pts',(-7.91039063560605,-0.0986121640945126,
146.637308106009));
#53698=CARTESIAN_POINT('Ctrl Pts',(-7.91049918122022,-0.0894822409103802,
146.636944670265));
#53699=CARTESIAN_POINT('Ctrl Pts',(-7.91086278010519,-0.0536862713631455,
146.635521741244));
#53700=CARTESIAN_POINT('Ctrl Pts',(-7.910998807096,-0.0270190770009432,
146.634466053238));
#53701=CARTESIAN_POINT('Ctrl Pts',(-7.91099999218839,-0.000351561277017258,
146.633414644735));
#53702=CARTESIAN_POINT('',(-7.91099997917165,0.000559131365739208,144.642309010809));
#53703=CARTESIAN_POINT('Ctrl Pts',(-7.91099986071816,0.0014844922367362,
146.642331508237));
#53704=CARTESIAN_POINT('Ctrl Pts',(-7.91096070114018,0.210169595666695,
146.63397861785));
#53705=CARTESIAN_POINT('Ctrl Pts',(-7.90265989499709,0.418657654408056,
146.625625727462));
#53706=CARTESIAN_POINT('Ctrl Pts',(-7.88616961499353,0.626298493972929,
146.617272837075));
#53707=CARTESIAN_POINT('Ctrl Pts',(-7.8696532919512,0.834267259954797,146.608906754998));
#53708=CARTESIAN_POINT('Ctrl Pts',(-7.84492168017966,1.04138585805498,146.600540672921));
#53709=CARTESIAN_POINT('Ctrl Pts',(-7.81209836721751,1.24701247023335,146.592174590845));
#53710=CARTESIAN_POINT('Ctrl Pts',(-7.77922265175918,1.45296736578069,146.583795152298));
#53711=CARTESIAN_POINT('Ctrl Pts',(-7.73822947183251,1.65742524414367,146.575415713752));
#53712=CARTESIAN_POINT('Ctrl Pts',(-7.68929294810761,1.85975669327539,146.567036275206));
#53713=CARTESIAN_POINT('Ctrl Pts',(-7.64023459965335,2.06259183519428,146.558635976518));
#53714=CARTESIAN_POINT('Ctrl Pts',(-7.58319341738956,2.26328968901699,146.550235677829));
#53715=CARTESIAN_POINT('Ctrl Pts',(-7.51839346328524,2.46123561066994,146.541835379141));
#53716=CARTESIAN_POINT('Ctrl Pts',(-7.45350555941553,2.65945019450961,146.533423679144));
#53717=CARTESIAN_POINT('Ctrl Pts',(-7.38083794575107,2.85490512674468,146.525011979146));
#53718=CARTESIAN_POINT('Ctrl Pts',(-7.30066244530874,3.04700654079683,146.516600279149));
#53719=CARTESIAN_POINT('Ctrl Pts',(-7.22031945268051,3.23950926803784,146.508171006527));
#53720=CARTESIAN_POINT('Ctrl Pts',(-7.13243732293407,3.42864421540676,146.499741733904));
#53721=CARTESIAN_POINT('Ctrl Pts',(-7.03733443343984,3.61384076460515,146.491312461282));
#53722=CARTESIAN_POINT('Ctrl Pts',(-7.00368404685071,3.6793691150963,146.488329920121));
#53723=CARTESIAN_POINT('Ctrl Pts',(-6.96913004297996,3.74440465389762,146.485347378961));
#53724=CARTESIAN_POINT('Ctrl Pts',(-6.93368780882427,3.8089229934145,146.4823648378));
#53725=CARTESIAN_POINT('Ctrl Pts',(-6.84048602586118,3.97858566903415,146.474521704867));
#53726=CARTESIAN_POINT('Ctrl Pts',(-6.7409070111708,4.1450914995612,146.466678571934));
#53727=CARTESIAN_POINT('Ctrl Pts',(-6.63518906266479,4.30792143645791,146.458835439));
#53728=CARTESIAN_POINT('Ctrl Pts',(-6.52959526863741,4.47056014692423,146.451001516992));
#53729=CARTESIAN_POINT('Ctrl Pts',(-6.41787708549216,4.6295312680319,146.443167594984));
#53730=CARTESIAN_POINT('Ctrl Pts',(-6.30031954512722,4.7843384735288,146.435333672975));
#53731=CARTESIAN_POINT('Ctrl Pts',(-6.18287720066292,4.93899398177679,146.427507427512));
#53732=CARTESIAN_POINT('Ctrl Pts',(-6.05960710492921,5.089493422178,146.419681182048));
#53733=CARTESIAN_POINT('Ctrl Pts',(-5.93083870144767,5.23536754176921,146.411854936584));
#53734=CARTESIAN_POINT('Ctrl Pts',(-5.8021714510098,5.38112707105105,146.404034838968));
#53735=CARTESIAN_POINT('Ctrl Pts',(-5.66801472669524,5.52226825387506,146.396214741352));
#53736=CARTESIAN_POINT('Ctrl Pts',(-5.52873965068755,5.65835301787679,146.388394643737));
#53737=CARTESIAN_POINT('Ctrl Pts',(-5.38954692141156,5.79435732142665,146.380579169773));
#53738=CARTESIAN_POINT('Ctrl Pts',(-5.2452421193869,5.92531091647335,146.372763695809));
#53739=CARTESIAN_POINT('Ctrl Pts',(-5.09623492766473,6.05081073593035,146.364948221845));
#53740=CARTESIAN_POINT('Ctrl Pts',(-4.94728689410474,6.17626073001594,146.357135850745));
#53741=CARTESIAN_POINT('Ctrl Pts',(-4.79364045898952,6.29626103633434,146.349323479645));
#53742=CARTESIAN_POINT('Ctrl Pts',(-4.63574039303495,6.41044709894592,146.341511108546));
#53743=CARTESIAN_POINT('Ctrl Pts',(-4.47784630416448,6.52462883920529,146.333699033172));
#53744=CARTESIAN_POINT('Ctrl Pts',(-4.31569918478182,6.6329965609269,146.325886957799));
#53745=CARTESIAN_POINT('Ctrl Pts',(-4.14977533552394,6.73522721700443,146.318074882425));
#53746=CARTESIAN_POINT('Ctrl Pts',(-3.98384663351259,6.83746086300879,146.310262578573));
#53747=CARTESIAN_POINT('Ctrl Pts',(-3.81414128072488,6.93355690060145,146.302450274721));
#53748=CARTESIAN_POINT('Ctrl Pts',(-3.64116286195743,7.02323671911335,146.294637970868));
#53749=CARTESIAN_POINT('Ctrl Pts',(-3.46814894800641,7.11293493993024,146.286824063931));
#53750=CARTESIAN_POINT('Ctrl Pts',(-3.29186094242496,7.19621415697964,146.279010156993));
#53751=CARTESIAN_POINT('Ctrl Pts',(-3.11282535646868,7.27284258733308,146.271196250056));
#53752=CARTESIAN_POINT('Ctrl Pts',(-2.93372152828843,7.3495002258156,146.263379364725));
#53753=CARTESIAN_POINT('Ctrl Pts',(-2.7518683566932,7.41950188962338,146.255562479394));
#53754=CARTESIAN_POINT('Ctrl Pts',(-2.56781070895024,7.48266457640595,146.247745594063));
#53755=CARTESIAN_POINT('Ctrl Pts',(-2.38355339760369,7.54589578133928,146.239920229066));
#53756=CARTESIAN_POINT('Ctrl Pts',(-2.19708716662012,7.60227307761764,146.232094864069));
#53757=CARTESIAN_POINT('Ctrl Pts',(-2.00897138739168,7.65166354230514,146.224269499071));
#53758=CARTESIAN_POINT('Ctrl Pts',(-1.82074127972997,7.70108402432807,146.216439378164));
#53759=CARTESIAN_POINT('Ctrl Pts',(-1.63085996805879,7.74350913581897,146.208609257256));
#53760=CARTESIAN_POINT('Ctrl Pts',(-1.43989538263479,7.77885738955709,146.200779136349));
#53761=CARTESIAN_POINT('Ctrl Pts',(-1.24866976128388,7.81425396201442,146.192938312185));
#53762=CARTESIAN_POINT('Ctrl Pts',(-1.05635825535513,7.84255430455995,146.185097488022));
#53763=CARTESIAN_POINT('Ctrl Pts',(-0.863533404153835,7.86372882670241,
146.177256663858));
#53764=CARTESIAN_POINT('Ctrl Pts',(-0.759466757756689,7.87515661463898,
146.173025008703));
#53765=CARTESIAN_POINT('Ctrl Pts',(-0.655250596235465,7.88450975841976,
146.168793353547));
#53766=CARTESIAN_POINT('Ctrl Pts',(-0.550974645430076,7.89178990724495,
146.164561698391));
#53767=CARTESIAN_POINT('Ctrl Pts',(-0.35602841327858,7.90540030899158,146.156650524032));
#53768=CARTESIAN_POINT('Ctrl Pts',(-0.160315528008974,7.91180125141527,
146.148739349672));
#53769=CARTESIAN_POINT('Ctrl Pts',(0.0355883609934201,7.91091995083769,
146.140828175313));
#53770=CARTESIAN_POINT('Ctrl Pts',(0.231279864754714,7.91003960570432,146.132925577693));
#53771=CARTESIAN_POINT('Ctrl Pts',(0.427161618077138,7.90189274456782,146.125022980073));
#53772=CARTESIAN_POINT('Ctrl Pts',(0.622652724432515,7.88645830425526,146.117120382454));
#53773=CARTESIAN_POINT('Ctrl Pts',(0.817968181673127,7.87103773181541,146.109224885332));
#53774=CARTESIAN_POINT('Ctrl Pts',(1.01289334956661,7.84834265117043,146.101329388211));
#53775=CARTESIAN_POINT('Ctrl Pts',(1.20684691750255,7.81840402625207,146.093433891089));
#53776=CARTESIAN_POINT('Ctrl Pts',(1.4006622098253,7.78848674552327,146.085544022917));
#53777=CARTESIAN_POINT('Ctrl Pts',(1.59350694285165,7.751336261671,146.077654154744));
#53778=CARTESIAN_POINT('Ctrl Pts',(1.78480423289768,7.70703541254551,146.069764286572));
#53779=CARTESIAN_POINT('Ctrl Pts',(1.97600063222358,7.66275792781044,146.061878579537));
#53780=CARTESIAN_POINT('Ctrl Pts',(2.16565087967339,7.61133766989136,146.053992872503));
#53781=CARTESIAN_POINT('Ctrl Pts',(2.35318732353836,7.55290873904474,146.046107165469));
#53782=CARTESIAN_POINT('Ctrl Pts',(2.54065964789161,7.49449978529931,146.038224154591));
#53783=CARTESIAN_POINT('Ctrl Pts',(2.72601928024173,7.42908703698421,146.030341143714));
#53784=CARTESIAN_POINT('Ctrl Pts',(2.90871252642285,7.35685479254762,146.022458132837));
#53785=CARTESIAN_POINT('Ctrl Pts',(3.09140849903498,7.28462147014981,146.014575004317));
#53786=CARTESIAN_POINT('Ctrl Pts',(3.2714376822132,7.20556856719058,146.006691875797));
#53787=CARTESIAN_POINT('Ctrl Pts',(3.44826466930564,7.11992919700881,145.998808747277));
#53788=CARTESIAN_POINT('Ctrl Pts',(3.62510258979157,7.03428453165718,145.990925131335));
#53789=CARTESIAN_POINT('Ctrl Pts',(3.79873760886763,6.94205273744811,145.983041515394));
#53790=CARTESIAN_POINT('Ctrl Pts',(3.9686572868143,6.8435137422099,145.975157899452));
#53791=CARTESIAN_POINT('Ctrl Pts',(4.13861603366217,6.74495209032407,145.967272470864));
#53792=CARTESIAN_POINT('Ctrl Pts',(4.30485743874423,6.64008052073081,145.959387042277));
#53793=CARTESIAN_POINT('Ctrl Pts',(4.46689629992931,6.52922341826943,145.951501613689));
#53794=CARTESIAN_POINT('Ctrl Pts',(4.62899965623215,6.41832219218346,145.943613046523));
#53795=CARTESIAN_POINT('Ctrl Pts',(4.78689685115993,6.30143088072875,145.935724479357));
#53796=CARTESIAN_POINT('Ctrl Pts',(4.94013394429008,6.17891556929474,145.927835912191));
#53797=CARTESIAN_POINT('Ctrl Pts',(5.09353411499974,6.05626987493559,145.919938949875));
#53798=CARTESIAN_POINT('Ctrl Pts',(5.24226400858081,5.92798844126273,145.912041987559));
#53799=CARTESIAN_POINT('Ctrl Pts',(5.38590406968878,5.79447653823103,145.904145025243));
#53800=CARTESIAN_POINT('Ctrl Pts',(5.52963173212614,5.66088321069906,145.89624324683));
#53801=CARTESIAN_POINT('Ctrl Pts',(5.66826313053842,5.52205329771764,145.888341468417));
#53802=CARTESIAN_POINT('Ctrl Pts',(5.80141734995539,5.37842706854305,145.880439690004));
#53803=CARTESIAN_POINT('Ctrl Pts',(5.93474378375484,5.23461508106149,145.872527691863));
#53804=CARTESIAN_POINT('Ctrl Pts',(6.06257866500054,5.08599464756745,145.864615693723));
#53805=CARTESIAN_POINT('Ctrl Pts',(6.18458224618046,4.93303795244163,145.856703695582));
#53806=CARTESIAN_POINT('Ctrl Pts',(6.23570048705311,4.86895067640507,145.85338865005));
#53807=CARTESIAN_POINT('Ctrl Pts',(6.28579556031459,4.80410249859803,145.850073604517));
#53808=CARTESIAN_POINT('Ctrl Pts',(6.33484481640776,4.7385295347852,145.846758558985));
#53809=CARTESIAN_POINT('Ctrl Pts',(6.45189805716921,4.58204341181436,145.838847392664));
#53810=CARTESIAN_POINT('Ctrl Pts',(6.56330678818272,4.42100714550051,145.830936226343));
#53811=CARTESIAN_POINT('Ctrl Pts',(6.66869797636449,4.25586516469122,145.823025060023));
#53812=CARTESIAN_POINT('Ctrl Pts',(6.77397492383228,4.0909021925649,145.815122469156));
#53813=CARTESIAN_POINT('Ctrl Pts',(6.87324713713644,3.92184265866409,145.80721987829));
#53814=CARTESIAN_POINT('Ctrl Pts',(6.96618221402821,3.74916342147912,145.799317287423));
#53815=CARTESIAN_POINT('Ctrl Pts',(7.05903380358072,3.57663930903866,145.791421795774));
#53816=CARTESIAN_POINT('Ctrl Pts',(7.14555943509989,3.40050227277601,145.783526304125));
#53817=CARTESIAN_POINT('Ctrl Pts',(7.22547021314931,3.22125770451419,145.775630812475));
#53818=CARTESIAN_POINT('Ctrl Pts',(7.30532403317756,3.04214089643896,145.767740948497));
#53819=CARTESIAN_POINT('Ctrl Pts',(7.3785722535376,2.85992128298122,145.759851084519));
#53820=CARTESIAN_POINT('Ctrl Pts',(7.44497197941793,2.67512863722137,145.75196122054));
#53821=CARTESIAN_POINT('Ctrl Pts',(7.51133669660912,2.49043342180787,145.744075516425));
#53822=CARTESIAN_POINT('Ctrl Pts',(7.57085999802765,2.30316820106481,145.736189812311));
#53823=CARTESIAN_POINT('Ctrl Pts',(7.62334707857467,2.11388275918677,145.728304108196));
#53824=CARTESIAN_POINT('Ctrl Pts',(7.67581622202991,1.92466200428138,145.720421098965));
#53825=CARTESIAN_POINT('Ctrl Pts',(7.72125384500339,1.73342273611908,145.712538089734));
#53826=CARTESIAN_POINT('Ctrl Pts',(7.75951489762185,1.54073020142549,145.704655080504));
#53827=CARTESIAN_POINT('Ctrl Pts',(7.79777653046566,1.3480347445673,145.696771951728));
#53828=CARTESIAN_POINT('Ctrl Pts',(7.82886130005154,1.1538863136922,145.688888822952));
#53829=CARTESIAN_POINT('Ctrl Pts',(7.85267509470553,0.958861229267025,145.681005694176));
#53830=CARTESIAN_POINT('Ctrl Pts',(7.87649036537527,0.763824056886142,145.673122076792));
#53831=CARTESIAN_POINT('Ctrl Pts',(7.89303372069079,0.567910465103365,145.665238459408));
#53832=CARTESIAN_POINT('Ctrl Pts',(7.90226284082103,0.37170283100762,145.657354842023));
#53833=CARTESIAN_POINT('Ctrl Pts',(7.91149408435247,0.175450054198505,145.649469410806));
#53834=CARTESIAN_POINT('Ctrl Pts',(7.91340772318329,-0.0210965551616383,
145.641583979589));
#53835=CARTESIAN_POINT('Ctrl Pts',(7.90801356134308,-0.217353430186908,
145.633698548371));
#53836=CARTESIAN_POINT('Ctrl Pts',(7.90261725169281,-0.413688449417042,
145.625809977388));
#53837=CARTESIAN_POINT('Ctrl Pts',(7.8899073528546,-0.609733159915272,145.617921406404));
#53838=CARTESIAN_POINT('Ctrl Pts',(7.86994565581487,-0.804907680743947,
145.61003283542));
#53839=CARTESIAN_POINT('Ctrl Pts',(7.84996271070972,-1.00028995349764,145.602135867511));
#53840=CARTESIAN_POINT('Ctrl Pts',(7.82271258430308,-1.19479984322531,145.594238899603));
#53841=CARTESIAN_POINT('Ctrl Pts',(7.78830863181515,-1.38786514315824,145.586341931694));
#53842=CARTESIAN_POINT('Ctrl Pts',(7.75388369305167,-1.58104821216395,145.578440146666));
#53843=CARTESIAN_POINT('Ctrl Pts',(7.71229630126433,-1.77278459843256,145.570538361638));
#53844=CARTESIAN_POINT('Ctrl Pts',(7.66371016324732,-1.96251561362953,145.56263657661));
#53845=CARTESIAN_POINT('Ctrl Pts',(7.61506117733343,-2.15249205264011,145.554724570342));
#53846=CARTESIAN_POINT('Ctrl Pts',(7.55939546008387,-2.34045760962865,145.546812564074));
#53847=CARTESIAN_POINT('Ctrl Pts',(7.49692584652523,-2.52587090954824,145.538900557806));
#53848=CARTESIAN_POINT('Ctrl Pts',(7.4707517460105,-2.60355710084037,145.535585511729));
#53849=CARTESIAN_POINT('Ctrl Pts',(7.44338378020625,-2.68079550062831,145.532270465653));
#53850=CARTESIAN_POINT('Ctrl Pts',(7.41484003564203,-2.75754750563615,145.528955419576));
#53851=CARTESIAN_POINT('Ctrl Pts',(7.34733185913206,-2.93907196854973,145.521115077705));
#53852=CARTESIAN_POINT('Ctrl Pts',(7.27305221069926,-3.11838892380742,145.513274735834));
#53853=CARTESIAN_POINT('Ctrl Pts',(7.19216390375891,-3.29495058862305,145.505434393962));
#53854=CARTESIAN_POINT('Ctrl Pts',(7.11136603235314,-3.47131485224254,145.497602817826));
#53855=CARTESIAN_POINT('Ctrl Pts',(7.02397435983904,-3.64492964307849,145.489771241691));
#53856=CARTESIAN_POINT('Ctrl Pts',(6.93020116613366,-3.81526313599988,145.481939665555));
#53857=CARTESIAN_POINT('Ctrl Pts',(6.83651458008369,-3.98543931120736,145.474115322557));
#53858=CARTESIAN_POINT('Ctrl Pts',(6.73645837867059,-4.15233991798948,145.466290979559));
#53859=CARTESIAN_POINT('Ctrl Pts',(6.63029261615817,-4.31545372169816,145.458466636561));
#53860=CARTESIAN_POINT('Ctrl Pts',(6.52420427454969,-4.47844857540045,145.45064799943));
#53861=CARTESIAN_POINT('Ctrl Pts',(6.41201543666426,-4.63766183289461,145.442829362299));
#53862=CARTESIAN_POINT('Ctrl Pts',(6.29403179840267,-4.7926072988193,145.435010725168));
#53863=CARTESIAN_POINT('Ctrl Pts',(6.1761112783406,-4.94746987292123,145.427196270806));
#53864=CARTESIAN_POINT('Ctrl Pts',(6.05240234581321,-5.09806892458549,145.419381816444));
#53865=CARTESIAN_POINT('Ctrl Pts',(5.92325378516453,-5.2439475203833,145.411567362082));
#53866=CARTESIAN_POINT('Ctrl Pts',(5.79414923184489,-5.38977640809814,145.403755570493));
#53867=CARTESIAN_POINT('Ctrl Pts',(5.6596089763201,-5.53088778187332,145.395943778904));
#53868=CARTESIAN_POINT('Ctrl Pts',(5.52002194177641,-5.66685792677979,145.388131987314));
#53869=CARTESIAN_POINT('Ctrl Pts',(5.38042837433479,-5.80283443530795,145.380319830121));
#53870=CARTESIAN_POINT('Ctrl Pts',(5.23578780148227,-5.93366898234449,145.372507672927));
#53871=CARTESIAN_POINT('Ctrl Pts',(5.08652621748585,-6.0589745038933,145.364695515733));
#53872=CARTESIAN_POINT('Ctrl Pts',(4.93725243122015,-6.18429026928164,145.356882719889));
#53873=CARTESIAN_POINT('Ctrl Pts',(4.7833571502544,-6.3040758819019,145.349069924044));
#53874=CARTESIAN_POINT('Ctrl Pts',(4.62529960652721,-6.41798446164053,145.341257128199));
#53875=CARTESIAN_POINT('Ctrl Pts',(4.46720132987094,-6.53192239670121,145.333442318923));
#53876=CARTESIAN_POINT('Ctrl Pts',(4.30493893892572,-6.63998007596844,145.325627509647));
#53877=CARTESIAN_POINT('Ctrl Pts',(4.13900092100807,-6.74185377888711,145.31781270037));
#53878=CARTESIAN_POINT('Ctrl Pts',(3.9729909385748,-6.84377166271005,145.309994501943));
#53879=CARTESIAN_POINT('Ctrl Pts',(3.8033024531629,-6.93950004389283,145.302176303516));
#53880=CARTESIAN_POINT('Ctrl Pts',(3.63044895345303,-7.02878093244994,145.294358105089));
#53881=CARTESIAN_POINT('Ctrl Pts',(3.45739425320743,-7.11816574347688,145.286530806322));
#53882=CARTESIAN_POINT('Ctrl Pts',(3.28116749311361,-7.20108791123106,145.278703507554));
#53883=CARTESIAN_POINT('Ctrl Pts',(3.10230357176408,-7.27733698193369,145.270876208787));
#53884=CARTESIAN_POINT('Ctrl Pts',(2.92332288731849,-7.35363582834012,145.263043800326));
#53885=CARTESIAN_POINT('Ctrl Pts',(2.74170193806947,-7.42325277108259,145.255211391866));
#53886=CARTESIAN_POINT('Ctrl Pts',(2.55799128137919,-7.48602709081313,145.247378983406));
#53887=CARTESIAN_POINT('Ctrl Pts',(2.3740169740096,-7.54889150053811,145.239535334336));
#53888=CARTESIAN_POINT('Ctrl Pts',(2.18794730468875,-7.60489357274815,145.231691685266));
#53889=CARTESIAN_POINT('Ctrl Pts',(2.00034467952648,-7.653923318344,145.223848036197));
#53890=CARTESIAN_POINT('Ctrl Pts',(1.89912660538616,-7.68037655384915,145.219616117521));
#53891=CARTESIAN_POINT('Ctrl Pts',(1.79746242346425,-7.70480105338649,145.215384198845));
#53892=CARTESIAN_POINT('Ctrl Pts',(1.69544106047893,-7.72718581441149,145.211152280169));
#53893=CARTESIAN_POINT('Ctrl Pts',(1.50456310870687,-7.76906682060793,145.203234527011));
#53894=CARTESIAN_POINT('Ctrl Pts',(1.31186409198688,-7.8039298644076,145.195316773853));
#53895=CARTESIAN_POINT('Ctrl Pts',(1.11790229142303,-7.83161640192056,145.187399020695));
#53896=CARTESIAN_POINT('Ctrl Pts',(0.924163339010726,-7.85927112959421,
145.179490364466));
#53897=CARTESIAN_POINT('Ctrl Pts',(0.729164830202006,-7.87976572598927,
145.171581708237));
#53898=CARTESIAN_POINT('Ctrl Pts',(0.533478058350739,-7.89299196510793,
145.163673052008));
#53899=CARTESIAN_POINT('Ctrl Pts',(0.337979892166719,-7.90620545659101,
145.155772018253));
#53900=CARTESIAN_POINT('Ctrl Pts',(0.141795125631044,-7.91216452283891,
145.147870984498));
#53901=CARTESIAN_POINT('Ctrl Pts',(-0.054496661243007,-7.91081229166218,
145.139969950743));
#53902=CARTESIAN_POINT('Ctrl Pts',(-0.250635582957945,-7.90946111355566,
145.132075070036));
#53903=CARTESIAN_POINT('Ctrl Pts',(-0.446881016145848,-7.90080998421351,
145.124180189329));
#53904=CARTESIAN_POINT('Ctrl Pts',(-0.642649897258296,-7.88485396881603,
145.116285308623));
#53905=CARTESIAN_POINT('Ctrl Pts',(-0.838302538104702,-7.86890742750588,
145.108395115602));
#53906=CARTESIAN_POINT('Ctrl Pts',(-1.03347884837812,-7.84566467070511,
145.100504922581));
#53907=CARTESIAN_POINT('Ctrl Pts',(-1.22759711815532,-7.81517282697553,
145.09261472956));
#53908=CARTESIAN_POINT('Ctrl Pts',(-1.42163603338515,-7.78469344815439,
145.084727762009));
#53909=CARTESIAN_POINT('Ctrl Pts',(-1.61461743037493,-7.74697094173008,
145.076840794458));
#53910=CARTESIAN_POINT('Ctrl Pts',(-1.80596578028313,-7.7021041670732,145.068953826907));
#53911=CARTESIAN_POINT('Ctrl Pts',(-1.99729751289319,-7.65724128878947,
145.061067544286));
#53912=CARTESIAN_POINT('Ctrl Pts',(-2.18699614429357,-7.60523545070669,
145.053181261665));
#53913=CARTESIAN_POINT('Ctrl Pts',(-2.37449686967172,-7.54623652000911,
145.045294979043));
#53914=CARTESIAN_POINT('Ctrl Pts',(-2.56199726549072,-7.48723769301052,
145.037408710283));
#53915=CARTESIAN_POINT('Ctrl Pts',(-2.74729943412486,-7.42124590078946,
145.029522441523));
#53916=CARTESIAN_POINT('Ctrl Pts',(-2.92985415210936,-7.34846076721973,
145.021636172763));
#53917=CARTESIAN_POINT('Ctrl Pts',(-3.11243914634898,-7.27566356241296,
145.013748596084));
#53918=CARTESIAN_POINT('Ctrl Pts',(-3.29227546195785,-7.19607089894714,
145.005861019405));
#53919=CARTESIAN_POINT('Ctrl Pts',(-3.46883403197991,-7.10993048197927,
144.997973442727));
#53920=CARTESIAN_POINT('Ctrl Pts',(-3.6454514760663,-7.02376134119217,144.990083235908));
#53921=CARTESIAN_POINT('Ctrl Pts',(-3.81878868736588,-6.93104024755936,
144.98219302909));
#53922=CARTESIAN_POINT('Ctrl Pts',(-3.98834114846013,-6.83206088113241,
144.974302822272));
#53923=CARTESIAN_POINT('Ctrl Pts',(-4.15805733980565,-6.73298593416105,
144.966404996186));
#53924=CARTESIAN_POINT('Ctrl Pts',(-4.32398118316231,-6.62764081706805,
144.9585071701));
#53925=CARTESIAN_POINT('Ctrl Pts',(-4.48563622476486,-6.51636314665453,
144.950609344015));
#53926=CARTESIAN_POINT('Ctrl Pts',(-4.64738077781904,-6.40502385969187,
144.942707144753));
#53927=CARTESIAN_POINT('Ctrl Pts',(-4.80485154056625,-6.28774567512402,
144.934804945492));
#53928=CARTESIAN_POINT('Ctrl Pts',(-4.95760490001591,-6.16490670289002,
144.926902746231));
#53929=CARTESIAN_POINT('Ctrl Pts',(-5.1105426443513,-6.04191945470359,144.918991008416));
#53930=CARTESIAN_POINT('Ctrl Pts',(-5.25875135179053,-5.91335823652702,
144.911079270601));
#53931=CARTESIAN_POINT('Ctrl Pts',(-5.40182325383769,-5.77963896227943,
144.903167532786));
#53932=CARTESIAN_POINT('Ctrl Pts',(-5.46100688095171,-5.72432417613491,
144.899894735444));
#53933=CARTESIAN_POINT('Ctrl Pts',(-5.51931197328507,-5.66812716490685,
144.896621938103));
#53934=CARTESIAN_POINT('Ctrl Pts',(-5.57671167798816,-5.61107902818971,
144.893349140761));
#53935=CARTESIAN_POINT('Ctrl Pts',(-5.72254114542075,-5.46614275302046,
144.885034284513));
#53936=CARTESIAN_POINT('Ctrl Pts',(-5.86284221960547,-5.31539421925882,
144.876719428264));
#53937=CARTESIAN_POINT('Ctrl Pts',(-5.99715259149553,-5.15927144026348,
144.868404572015));
#53938=CARTESIAN_POINT('Ctrl Pts',(-6.13129756483191,-5.00334092104287,
144.860099955223));
#53939=CARTESIAN_POINT('Ctrl Pts',(-6.25946635928404,-4.8420495774869,144.851795338431));
#53940=CARTESIAN_POINT('Ctrl Pts',(-6.38123353964414,-4.67587205904104,
144.843490721638));
#53941=CARTESIAN_POINT('Ctrl Pts',(-6.50285879985164,-4.5098882211806,144.835195783911));
#53942=CARTESIAN_POINT('Ctrl Pts',(-6.61809715472091,-4.33902980270076,
144.826900846184));
#53943=CARTESIAN_POINT('Ctrl Pts',(-6.72656296210199,-4.16380495663254,
144.818605908457));
#53944=CARTESIAN_POINT('Ctrl Pts',(-6.83486619940837,-3.98884274002332,
144.810323403299));
#53945=CARTESIAN_POINT('Ctrl Pts',(-6.93641699278435,-3.80952740488747,
144.802040898141));
#53946=CARTESIAN_POINT('Ctrl Pts',(-7.03087254620634,-3.62639659152194,
144.793758392983));
#53947=CARTESIAN_POINT('Ctrl Pts',(-7.12524132875031,-3.44343400988967,
144.785483496486));
#53948=CARTESIAN_POINT('Ctrl Pts',(-7.21252773529438,-3.25666319938354,
144.777208599989));
#53949=CARTESIAN_POINT('Ctrl Pts',(-7.29243360353874,-3.06664851881969,
144.768933703491));
#53950=CARTESIAN_POINT('Ctrl Pts',(-7.37224806995356,-2.87685119012029,
144.76066827239));
#53951=CARTESIAN_POINT('Ctrl Pts',(-7.44469873091024,-2.68381766523571,
144.752402841288));
#53952=CARTESIAN_POINT('Ctrl Pts',(-7.50953436370736,-2.48813477132939,
144.744137410187));
#53953=CARTESIAN_POINT('Ctrl Pts',(-7.53487068490354,-2.41166625488684,
144.74090746381));
#53954=CARTESIAN_POINT('Ctrl Pts',(-7.55904464307123,-2.33479340311073,
144.737677517434));
#53955=CARTESIAN_POINT('Ctrl Pts',(-7.58204322356163,-2.25755211590856,
144.734447571058));
#53956=CARTESIAN_POINT('Ctrl Pts',(-7.6367944674298,-2.07366874301679,144.726758245109));
#53957=CARTESIAN_POINT('Ctrl Pts',(-7.68484746179367,-1.88780794319174,
144.719068919161));
#53958=CARTESIAN_POINT('Ctrl Pts',(-7.72607096885417,-1.70051415290459,
144.711379593213));
#53959=CARTESIAN_POINT('Ctrl Pts',(-7.76730118200993,-1.51318989432178,
144.703689016393));
#53960=CARTESIAN_POINT('Ctrl Pts',(-7.80169962506568,-1.32443253807318,
144.695998439572));
#53961=CARTESIAN_POINT('Ctrl Pts',(-7.82918637756967,-1.13479586943093,
144.688307862751));
#53962=CARTESIAN_POINT('Ctrl Pts',(-7.85669790838933,-0.944988250173958,
144.680610353153));
#53963=CARTESIAN_POINT('Ctrl Pts',(-7.87728525577776,-0.754300096158211,
144.672912843555));
#53964=CARTESIAN_POINT('Ctrl Pts',(-7.89092041321999,-0.563290362271563,
144.665215333957));
#53965=CARTESIAN_POINT('Ctrl Pts',(-7.90432776465935,-0.375471876023305,
144.657646428587));
#53966=CARTESIAN_POINT('Ctrl Pts',(-7.91101345033552,-0.187342803459868,
144.650077523217));
#53967=CARTESIAN_POINT('Ctrl Pts',(-7.91099997967269,0.000567114363191055,
144.642508617847));
#53968=CARTESIAN_POINT('',(-7.91099998020127,-0.000555341303987942,142.642353853155));
#53969=CARTESIAN_POINT('Ctrl Pts',(-7.91099997917165,0.000559131365739208,
144.642309010808));
#53970=CARTESIAN_POINT('Ctrl Pts',(-7.91083596349065,2.2020457259927,144.553729074218));
#53971=CARTESIAN_POINT('Ctrl Pts',(-6.94200761631339,4.38622928711889,144.465149137628));
#53972=CARTESIAN_POINT('Ctrl Pts',(-3.67820201487554,7.34180684108,144.287981765306));
#53973=CARTESIAN_POINT('Ctrl Pts',(-1.40868175870934,8.08992666571478,144.199394329573));
#53974=CARTESIAN_POINT('Ctrl Pts',(2.97309270522046,7.65454228024958,144.022219458108));
#53975=CARTESIAN_POINT('Ctrl Pts',(5.05102072676259,6.47444880833715,143.933632022375));
#53976=CARTESIAN_POINT('Ctrl Pts',(7.66951518848171,2.93425195366926,143.756457150909));
#53977=CARTESIAN_POINT('Ctrl Pts',(8.18956872247134,0.60188196009079,143.667869715177));
#53978=CARTESIAN_POINT('Ctrl Pts',(7.32306689760961,-3.71537198233204,143.490694843711));
#53979=CARTESIAN_POINT('Ctrl Pts',(5.94329958849617,-5.66643518937126,143.402107407979));
#53980=CARTESIAN_POINT('Ctrl Pts',(2.16154501637024,-7.92205913233223,143.224932536513));
#53981=CARTESIAN_POINT('Ctrl Pts',(-0.21081652930894,-8.20894963712981,
143.13634510078));
#53982=CARTESIAN_POINT('Ctrl Pts',(-4.42123908577165,-6.91982244717367,
142.959170229315));
#53983=CARTESIAN_POINT('Ctrl Pts',(-6.22631625634753,-5.35390358802864,
142.870582793582));
#53984=CARTESIAN_POINT('Ctrl Pts',(-7.653094167907,-2.31351615424296,142.735448189618));
#53985=CARTESIAN_POINT('Ctrl Pts',(-7.91091749410943,-1.15739837654274,
142.688901021386));
#53986=CARTESIAN_POINT('Ctrl Pts',(-7.91099998020127,-0.000555341303987942,
142.642353853155));
#53987=CARTESIAN_POINT('',(-7.91156134791759,-0.0007562664353129,140.64330292144));
#53988=CARTESIAN_POINT('Ctrl Pts',(-7.91099998025987,-0.000558863451393805,
142.642266634146));
#53989=CARTESIAN_POINT('Ctrl Pts',(-7.91101396606582,0.197417422812076,
142.634266600749));
#53990=CARTESIAN_POINT('Ctrl Pts',(-7.90359199240421,0.39563115781575,142.626266567353));
#53991=CARTESIAN_POINT('Ctrl Pts',(-7.88870658119376,0.593489238175604,
142.618266533957));
#53992=CARTESIAN_POINT('Ctrl Pts',(-7.87383727106835,0.791133301621042,
142.610275153947));
#53993=CARTESIAN_POINT('Ctrl Pts',(-7.85152063367933,0.988422146600453,
142.602283773937));
#53994=CARTESIAN_POINT('Ctrl Pts',(-7.82178119339689,1.18476156361639,142.594292393928));
#53995=CARTESIAN_POINT('Ctrl Pts',(-7.79207685683757,1.38086922628637,142.586310446751));
#53996=CARTESIAN_POINT('Ctrl Pts',(-7.75496723908072,1.57602936757451,142.578328499575));
#53997=CARTESIAN_POINT('Ctrl Pts',(-7.71052873213815,1.76965185018752,142.570346552399));
#53998=CARTESIAN_POINT('Ctrl Pts',(-7.66612070386264,1.9631415345679,142.562370079734));
#53999=CARTESIAN_POINT('Ctrl Pts',(-7.61439387511261,2.15509533749356,142.55439360707));
#54000=CARTESIAN_POINT('Ctrl Pts',(-7.5554760441043,2.34493128832511,142.546417134405));
#54001=CARTESIAN_POINT('Ctrl Pts',(-7.49659622615169,2.53464475934965,142.538445808062));
#54002=CARTESIAN_POINT('Ctrl Pts',(-7.43053475480413,2.72224278470734,142.530474481718));
#54003=CARTESIAN_POINT('Ctrl Pts',(-7.35746985812211,2.90715639187586,142.522503155375));
#54004=CARTESIAN_POINT('Ctrl Pts',(-7.3187358346882,3.00518497083198,142.518277301985));
#54005=CARTESIAN_POINT('Ctrl Pts',(-7.2780344182534,3.10245935149916,142.514051448594));
#54006=CARTESIAN_POINT('Ctrl Pts',(-7.2353978186162,3.19889659200856,142.509825595203));
#54007=CARTESIAN_POINT('Ctrl Pts',(-7.1519925489431,3.38754611189657,142.501559025058));
#54008=CARTESIAN_POINT('Ctrl Pts',(-7.06125235358972,3.57282549477544,142.493292454913));
#54009=CARTESIAN_POINT('Ctrl Pts',(-6.96348352833377,3.75417343107965,142.485025884768));
#54010=CARTESIAN_POINT('Ctrl Pts',(-6.86562710107853,3.93568385723422,142.476751907681));
#54011=CARTESIAN_POINT('Ctrl Pts',(-6.76072961063135,4.11325554586154,142.468477930593));
#54012=CARTESIAN_POINT('Ctrl Pts',(-6.64914181382372,4.2863544113455,142.460203953506));
#54013=CARTESIAN_POINT('Ctrl Pts',(-6.5374467900207,4.45961961106836,142.451922025785));
#54014=CARTESIAN_POINT('Ctrl Pts',(-6.41904878404736,4.62840316036439,142.443640098063));
#54015=CARTESIAN_POINT('Ctrl Pts',(-6.29434059322681,4.79220173787135,142.435358170342));
#54016=CARTESIAN_POINT('Ctrl Pts',(-6.16942568390501,4.95627183079542,142.427062514351));
#54017=CARTESIAN_POINT('Ctrl Pts',(-6.038179856008,5.11534019772091,142.41876685836));
#54018=CARTESIAN_POINT('Ctrl Pts',(-5.90103607306085,5.26893672997073,142.410471202369));
#54019=CARTESIAN_POINT('Ctrl Pts',(-5.76376833867507,5.42267208376047,142.402168048711));
#54020=CARTESIAN_POINT('Ctrl Pts',(-5.62059220905539,5.57092551696632,142.393864895052));
#54021=CARTESIAN_POINT('Ctrl Pts',(-5.471976837168,5.71326443406018,142.385561741394));
#54022=CARTESIAN_POINT('Ctrl Pts',(-5.32313488081947,5.85582036630137,142.377245928442));
#54023=CARTESIAN_POINT('Ctrl Pts',(-5.16883732252925,5.99244355951086,142.36893011549));
#54024=CARTESIAN_POINT('Ctrl Pts',(-5.0095870836539,6.12274107335007,142.360614302538));
#54025=CARTESIAN_POINT('Ctrl Pts',(-4.94772987490577,6.17335224084241,142.357384210192));
#54026=CARTESIAN_POINT('Ctrl Pts',(-4.88512574290236,6.22300947232399,142.354154117846));
#54027=CARTESIAN_POINT('Ctrl Pts',(-4.82180532302,6.27169151241481,142.3509240255));
#54028=CARTESIAN_POINT('Ctrl Pts',(-4.66672440730128,6.39092090745619,142.343013059657));
#54029=CARTESIAN_POINT('Ctrl Pts',(-4.50702284465997,6.50454530354762,142.335102093814));
#54030=CARTESIAN_POINT('Ctrl Pts',(-4.34314304490546,6.61218795040563,142.32719112797));
#54031=CARTESIAN_POINT('Ctrl Pts',(-4.17942907636278,6.71972167285319,142.319288167294));
#54032=CARTESIAN_POINT('Ctrl Pts',(-4.01154557821584,6.82128551566821,142.311385206617));
#54033=CARTESIAN_POINT('Ctrl Pts',(-3.83996763692179,6.9165431790305,142.30348224594));
#54034=CARTESIAN_POINT('Ctrl Pts',(-3.66853156416113,7.01172207897545,142.295585819794));
#54035=CARTESIAN_POINT('Ctrl Pts',(-3.49340743333372,7.10060502088164,142.287689393649));
#54036=CARTESIAN_POINT('Ctrl Pts',(-3.3150991308719,7.182899049304,142.279792967503));
#54037=CARTESIAN_POINT('Ctrl Pts',(-3.13690527287704,7.26514025855819,142.271901609559));
#54038=CARTESIAN_POINT('Ctrl Pts',(-2.95553162687625,7.34080083646944,142.264010251614));
#54039=CARTESIAN_POINT('Ctrl Pts',(-2.77150674539036,7.40963368596962,142.256118893669));
#54040=CARTESIAN_POINT('Ctrl Pts',(-2.58756593752473,7.47843508848935,142.248231140971));
#54041=CARTESIAN_POINT('Ctrl Pts',(-2.40097662985685,7.5404148581255,142.240343388273));
#54042=CARTESIAN_POINT('Ctrl Pts',(-2.21228768731736,7.59537386759493,142.232455635574));
#54043=CARTESIAN_POINT('Ctrl Pts',(-2.02365005161559,7.65031793303563,142.224570027653));
#54044=CARTESIAN_POINT('Ctrl Pts',(-1.83291424938462,7.6982449471224,142.216684419731));
#54045=CARTESIAN_POINT('Ctrl Pts',(-1.64064492386193,7.73900544216155,142.208798811809));
#54046=CARTESIAN_POINT('Ctrl Pts',(-1.44835292184097,7.77977074454733,142.200912273849));
#54047=CARTESIAN_POINT('Ctrl Pts',(-1.25452737076121,7.81336776091123,142.193025735888));
#54048=CARTESIAN_POINT('Ctrl Pts',(-1.05974437350371,7.83969788083873,142.185139197927));
#54049=CARTESIAN_POINT('Ctrl Pts',(-0.864936837270453,7.86603131786363,
142.177251666412));
#54050=CARTESIAN_POINT('Ctrl Pts',(-0.669171956001874,7.88509598734318,
142.169364134897));
#54051=CARTESIAN_POINT('Ctrl Pts',(-0.473032219651286,7.89684503578307,
142.161476603381));
#54052=CARTESIAN_POINT('Ctrl Pts',(-0.276834898113549,7.90859753365736,
142.153586756144));
#54053=CARTESIAN_POINT('Ctrl Pts',(-0.0802628461053111,7.91303010974445,
142.145696908908));
#54054=CARTESIAN_POINT('Ctrl Pts',(0.11609991967804,7.91014802697464,142.137807061671));
#54055=CARTESIAN_POINT('Ctrl Pts',(0.312553249532429,7.9072646149653,142.129913575574));
#54056=CARTESIAN_POINT('Ctrl Pts',(0.508796756665151,7.89705982647217,142.122020089477));
#54057=CARTESIAN_POINT('Ctrl Pts',(0.704249769468778,7.87959093241541,142.11412660338));
#54058=CARTESIAN_POINT('Ctrl Pts',(0.899928725686014,7.86210184434119,142.106223992423));
#54059=CARTESIAN_POINT('Ctrl Pts',(1.09481501909843,7.83733190836066,142.098321381467));
#54060=CARTESIAN_POINT('Ctrl Pts',(1.28833525885604,7.80539001336822,142.090418770511));
#54061=CARTESIAN_POINT('Ctrl Pts',(1.48198385178215,7.77342693277042,142.082510918113));
#54062=CARTESIAN_POINT('Ctrl Pts',(1.67426424830275,7.73428247856622,142.074603065714));
#54063=CARTESIAN_POINT('Ctrl Pts',(1.86461625191157,7.68811597422329,142.066695213316));
#54064=CARTESIAN_POINT('Ctrl Pts',(2.05522871105117,7.64188630100814,142.058776540732));
#54065=CARTESIAN_POINT('Ctrl Pts',(2.24390717669586,7.58861547974743,142.050857868149));
#54066=CARTESIAN_POINT('Ctrl Pts',(2.4301084074716,7.52851207928471,142.042939195566));
#54067=CARTESIAN_POINT('Ctrl Pts',(2.50706496337553,7.50367147711224,142.039666425741));
#54068=CARTESIAN_POINT('Ctrl Pts',(2.58359862466643,7.47766432900829,142.036393655917));
#54069=CARTESIAN_POINT('Ctrl Pts',(2.65967219190864,7.45050768951941,142.033120886092));
#54070=CARTESIAN_POINT('Ctrl Pts',(2.84198110194762,7.3854273005615,142.025277753173));
#54071=CARTESIAN_POINT('Ctrl Pts',(3.02218579136077,7.31354933772559,142.017434620255));
#54072=CARTESIAN_POINT('Ctrl Pts',(3.19973595932908,7.23502666135906,142.009591487336));
#54073=CARTESIAN_POINT('Ctrl Pts',(3.37707761352304,7.15659620151819,142.001757565342));
#54074=CARTESIAN_POINT('Ctrl Pts',(3.55177063578898,7.07153670688227,141.993923643347));
#54075=CARTESIAN_POINT('Ctrl Pts',(3.72327973891718,6.98005078676143,141.986089721353));
#54076=CARTESIAN_POINT('Ctrl Pts',(3.89462077842683,6.88865451467968,141.978263475904));
#54077=CARTESIAN_POINT('Ctrl Pts',(4.06278380421339,6.79084452189787,141.970437230454));
#54078=CARTESIAN_POINT('Ctrl Pts',(4.22725320722755,6.68687156463951,141.962610985005));
#54079=CARTESIAN_POINT('Ctrl Pts',(4.39159341254989,6.58298028254895,141.954790887403));
#54080=CARTESIAN_POINT('Ctrl Pts',(4.55224547833337,6.47293586517373,141.946970789801));
#54081=CARTESIAN_POINT('Ctrl Pts',(4.70871796283319,6.35703516951826,141.9391506922));
#54082=CARTESIAN_POINT('Ctrl Pts',(4.86509793259174,6.24120300043414,141.93133521825));
#54083=CARTESIAN_POINT('Ctrl Pts',(5.01730296197389,6.11952165904375,141.9235197443));
#54084=CARTESIAN_POINT('Ctrl Pts',(5.1648700477419,5.99233163217279,141.91570427035));
#54085=CARTESIAN_POINT('Ctrl Pts',(5.31237854709233,5.86519210171156,141.907891899265));
#54086=CARTESIAN_POINT('Ctrl Pts',(5.45525250555584,5.73254847238278,141.900079528179));
#54087=CARTESIAN_POINT('Ctrl Pts',(5.59306137127033,5.5947819883534,141.892267157093));
#54088=CARTESIAN_POINT('Ctrl Pts',(5.73086502042888,5.45702071927568,141.884455081734));
#54089=CARTESIAN_POINT('Ctrl Pts',(5.86360370383074,5.3141372239608,141.876643006374));
#54090=CARTESIAN_POINT('Ctrl Pts',(5.99088284554568,5.16655046727955,141.868830931014));
#54091=CARTESIAN_POINT('Ctrl Pts',(6.11816570977847,5.01895939414605,141.861018627176));
#54092=CARTESIAN_POINT('Ctrl Pts',(6.23998848388287,4.86666505156086,141.853206323338));
#54093=CARTESIAN_POINT('Ctrl Pts',(6.35599613246674,4.71012039804376,141.845394019499));
#54094=CARTESIAN_POINT('Ctrl Pts',(6.47202758583008,4.55354362155027,141.837580112575));
#54095=CARTESIAN_POINT('Ctrl Pts',(6.58224132716533,4.39271507933296,141.829766205651));
#54096=CARTESIAN_POINT('Ctrl Pts',(6.68632491450132,4.22811780083277,141.821952298727));
#54097=CARTESIAN_POINT('Ctrl Pts',(6.79044817493164,4.06345778349426,141.81413541341));
#54098=CARTESIAN_POINT('Ctrl Pts',(6.88843643913402,3.89502646545144,141.806318528093));
#54099=CARTESIAN_POINT('Ctrl Pts',(6.98002251231746,3.7233327446713,141.798501642776));
#54100=CARTESIAN_POINT('Ctrl Pts',(7.0717079370148,3.55145277252679,141.790676277792));
#54101=CARTESIAN_POINT('Ctrl Pts',(7.15697713402299,3.37630363968181,141.782850912808));
#54102=CARTESIAN_POINT('Ctrl Pts',(7.23561004969321,3.19841651583696,141.775025547823));
#54103=CARTESIAN_POINT('Ctrl Pts',(7.31429075496577,3.02042128007946,141.767195426929));
#54104=CARTESIAN_POINT('Ctrl Pts',(7.38632701118634,2.8396850627496,141.759365306035));
#54105=CARTESIAN_POINT('Ctrl Pts',(7.45154818893114,2.6567556507961,141.751535185141));
#54106=CARTESIAN_POINT('Ctrl Pts',(7.51685851970399,2.47357618645844,141.74369436099));
#54107=CARTESIAN_POINT('Ctrl Pts',(7.57533506014372,2.288197873882,141.735853536839));
#54108=CARTESIAN_POINT('Ctrl Pts',(7.62685768736909,2.10118129075504,141.728012712689));
#54109=CARTESIAN_POINT('Ctrl Pts',(7.65466420313479,2.00024933430764,141.723781057354));
#54110=CARTESIAN_POINT('Ctrl Pts',(7.6804461335336,1.89884034749855,141.719549402019));
#54111=CARTESIAN_POINT('Ctrl Pts',(7.70419086017597,1.79704317977644,141.715317746684));
#54112=CARTESIAN_POINT('Ctrl Pts',(7.74858215794803,1.60673109689738,141.707406572348));
#54113=CARTESIAN_POINT('Ctrl Pts',(7.78597718486723,1.41451736889222,141.699495398012));
#54114=CARTESIAN_POINT('Ctrl Pts',(7.8162126789919,1.22095878585896,141.691584223675));
#54115=CARTESIAN_POINT('Ctrl Pts',(7.84641539391533,1.02761004546037,141.683681626079));
#54116=CARTESIAN_POINT('Ctrl Pts',(7.86947398378279,0.832919691770439,141.675779028483));
#54117=CARTESIAN_POINT('Ctrl Pts',(7.88527541788998,0.637457907645663,141.667876430887));
#54118=CARTESIAN_POINT('Ctrl Pts',(7.90106265437923,0.442171746297559,141.659980933789));
#54119=CARTESIAN_POINT('Ctrl Pts',(7.9096056970441,0.246115876839994,141.652085436692));
#54120=CARTESIAN_POINT('Ctrl Pts',(7.91084281652067,0.0498691518213697,
141.644189939594));
#54121=CARTESIAN_POINT('Ctrl Pts',(7.91207905401571,-0.146237662711553,
141.636300071446));
#54122=CARTESIAN_POINT('Ctrl Pts',(7.90601974352117,-0.342534718297289,
141.628410203298));
#54123=CARTESIAN_POINT('Ctrl Pts',(7.89265507442595,-0.538439296614054,
141.620520335149));
#54124=CARTESIAN_POINT('Ctrl Pts',(7.87929745389464,-0.734240554307788,
141.612634628139));
#54125=CARTESIAN_POINT('Ctrl Pts',(7.85864217554049,-0.92964940398611,141.60474892113));
#54126=CARTESIAN_POINT('Ctrl Pts',(7.83073150669614,-1.12408410274164,141.59686321412));
#54127=CARTESIAN_POINT('Ctrl Pts',(7.80283038062938,-1.31845232343824,141.588980203267));
#54128=CARTESIAN_POINT('Ctrl Pts',(7.76767885704064,-1.51184671610671,141.581097192414));
#54129=CARTESIAN_POINT('Ctrl Pts',(7.72537098081794,-1.70369134784916,141.573214181561));
#54130=CARTESIAN_POINT('Ctrl Pts',(7.683062473214,-1.89553884258334,141.565331053067));
#54131=CARTESIAN_POINT('Ctrl Pts',(7.63359746557776,-2.08583619164996,141.557447924572));
#54132=CARTESIAN_POINT('Ctrl Pts',(7.57712110211298,-2.27401776684226,141.549564796077));
#54133=CARTESIAN_POINT('Ctrl Pts',(7.52064124665819,-2.46221097748943,141.541681180161));
#54134=CARTESIAN_POINT('Ctrl Pts',(7.45714927014244,-2.64828782294039,141.533797564244));
#54135=CARTESIAN_POINT('Ctrl Pts',(7.38684018405892,-2.83169791735848,141.525913948328));
#54136=CARTESIAN_POINT('Ctrl Pts',(7.316514932111,-3.01515018246717,141.518028519765));
#54137=CARTESIAN_POINT('Ctrl Pts',(7.23936957072014,-3.19593415264087,141.510143091203));
#54138=CARTESIAN_POINT('Ctrl Pts',(7.15564732919218,-3.3735192752117,141.502257662641));
#54139=CARTESIAN_POINT('Ctrl Pts',(7.07189176432692,-3.55117508065998,141.494369095501));
#54140=CARTESIAN_POINT('Ctrl Pts',(6.98155425019417,-3.72562918976471,141.48648052836));
#54141=CARTESIAN_POINT('Ctrl Pts',(6.88492415136977,-3.89637529376794,141.47859196122));
#54142=CARTESIAN_POINT('Ctrl Pts',(6.7881912171149,-4.0673031087424,141.470694998929));
#54143=CARTESIAN_POINT('Ctrl Pts',(6.68515249212069,-4.2345147363401,141.462798036639));
#54144=CARTESIAN_POINT('Ctrl Pts',(6.57614148809467,-4.39753159494733,141.454901074348));
#54145=CARTESIAN_POINT('Ctrl Pts',(6.46706400185862,-4.56064787215115,141.446999295961));
#54146=CARTESIAN_POINT('Ctrl Pts',(6.35200717688742,-4.71956400151608,141.439097517574));
#54147=CARTESIAN_POINT('Ctrl Pts',(6.23134521550626,-4.87383399442239,141.431195739187));
#54148=CARTESIAN_POINT('Ctrl Pts',(6.11052719654456,-5.02830351169883,141.423283741072));
#54149=CARTESIAN_POINT('Ctrl Pts',(5.98408978299929,-5.1781146272737,141.415371742957));
#54150=CARTESIAN_POINT('Ctrl Pts',(5.8524452240126,-5.32285693025203,141.407459744842));
#54151=CARTESIAN_POINT('Ctrl Pts',(5.79728750742877,-5.38350246689117,141.404144698987));
#54152=CARTESIAN_POINT('Ctrl Pts',(5.74121608317219,-5.44325863162316,141.400829653132));
#54153=CARTESIAN_POINT('Ctrl Pts',(5.68426301255612,-5.5020973277548,141.397514607277));
#54154=CARTESIAN_POINT('Ctrl Pts',(5.54834778401845,-5.64251249317228,141.38960344094));
#54155=CARTESIAN_POINT('Ctrl Pts',(5.4070439001594,-5.77807722674997,141.381692274603));
#54156=CARTESIAN_POINT('Ctrl Pts',(5.26073092161834,-5.90835266130321,141.373781108266));
#54157=CARTESIAN_POINT('Ctrl Pts',(5.11457654171377,-6.03848688140989,141.365878517384));
#54158=CARTESIAN_POINT('Ctrl Pts',(4.96342413749641,-6.16334299540037,141.357975926501));
#54159=CARTESIAN_POINT('Ctrl Pts',(4.80769173920856,-6.28251710230428,141.350073335618));
#54160=CARTESIAN_POINT('Ctrl Pts',(4.65209924163074,-6.40158415028945,141.342177843952));
#54161=CARTESIAN_POINT('Ctrl Pts',(4.49193521834265,-6.51497915131509,141.334282352286));
#54162=CARTESIAN_POINT('Ctrl Pts',(4.32765277895553,-6.62233662877375,141.32638686062));
#54163=CARTESIAN_POINT('Ctrl Pts',(4.16348743519291,-6.72961758502348,141.318496996625));
#54164=CARTESIAN_POINT('Ctrl Pts',(3.9952098113043,-6.83086940362176,141.31060713263));
#54165=CARTESIAN_POINT('Ctrl Pts',(3.82330439283543,-6.92576815376643,141.302717268635));
#54166=CARTESIAN_POINT('Ctrl Pts',(3.65148961002931,-7.02061686935612,141.294831564504));
#54167=CARTESIAN_POINT('Ctrl Pts',(3.47605114517209,-7.10911902477591,141.286945860372));
#54168=CARTESIAN_POINT('Ctrl Pts',(3.29750087674578,-7.19099499150575,141.279060156241));
#54169=CARTESIAN_POINT('Ctrl Pts',(3.11901162661846,-7.27284297769956,141.271177146993));
#54170=CARTESIAN_POINT('Ctrl Pts',(2.9374130054616,-7.34806914478693,141.263294137746));
#54171=CARTESIAN_POINT('Ctrl Pts',(2.75324005826381,-7.41644053313795,141.255411128498));
#54172=CARTESIAN_POINT('Ctrl Pts',(2.56906431809793,-7.48481295833564,141.247527999705));
#54173=CARTESIAN_POINT('Ctrl Pts',(2.38231449418747,-7.54633026916426,141.239644870913));
#54174=CARTESIAN_POINT('Ctrl Pts',(2.19354465274656,-7.60080803970255,141.23176174212));
#54175=CARTESIAN_POINT('Ctrl Pts',(2.0047631110577,-7.65528918685767,141.223878124718));
#54176=CARTESIAN_POINT('Ctrl Pts',(1.81396163369587,-7.70272982805217,141.215994507317));
#54177=CARTESIAN_POINT('Ctrl Pts',(1.62170849017035,-7.74299571050568,141.208110889916));
#54178=CARTESIAN_POINT('Ctrl Pts',(1.42941111376424,-7.78327085718207,141.200225458681));
#54179=CARTESIAN_POINT('Ctrl Pts',(1.23566174328376,-7.81636788504171,141.192340027447));
#54180=CARTESIAN_POINT('Ctrl Pts',(1.04103809916656,-7.8422038150053,141.184454596212));
#54181=CARTESIAN_POINT('Ctrl Pts',(0.84633696115265,-7.86805003214081,141.176566025212));
#54182=CARTESIAN_POINT('Ctrl Pts',(0.650761197511675,-7.88662934509372,
141.168677454211));
#54183=CARTESIAN_POINT('Ctrl Pts',(0.454893143980661,-7.89791068748941,
141.16078888321));
#54184=CARTESIAN_POINT('Ctrl Pts',(0.258816600300158,-7.90920403821784,
141.152891915284));
#54185=CARTESIAN_POINT('Ctrl Pts',(0.0624474897329449,-7.91318388217811,
141.144994947358));
#54186=CARTESIAN_POINT('Ctrl Pts',(-0.133631241430665,-7.90987128158946,
141.137097979432));
#54187=CARTESIAN_POINT('Ctrl Pts',(-0.329829579847529,-7.90655666032751,
141.129196194387));
#54188=CARTESIAN_POINT('Ctrl Pts',(-0.525736842255237,-7.8959407446982,
141.121294409342));
#54189=CARTESIAN_POINT('Ctrl Pts',(-0.720775434481017,-7.87809645619097,
141.113392624297));
#54190=CARTESIAN_POINT('Ctrl Pts',(-0.916066316057366,-7.86022908546238,
141.105480618012));
#54191=CARTESIAN_POINT('Ctrl Pts',(-1.11048594208799,-7.8351147098806,141.097568611727));
#54192=CARTESIAN_POINT('Ctrl Pts',(-1.30346601147186,-7.80287750492968,
141.089656605442));
#54193=CARTESIAN_POINT('Ctrl Pts',(-1.38432259279204,-7.78937046147192,
141.086341559584));
#54194=CARTESIAN_POINT('Ctrl Pts',(-1.46492662522691,-7.77461359795081,
141.083026513727));
#54195=CARTESIAN_POINT('Ctrl Pts',(-1.5452371234515,-7.75861864202046,141.079711467869));
#54196=CARTESIAN_POINT('Ctrl Pts',(-1.73517771216056,-7.72078932439762,
141.071871126));
#54197=CARTESIAN_POINT('Ctrl Pts',(-1.92401397181497,-7.67592392978999,
141.064030784131));
#54198=CARTESIAN_POINT('Ctrl Pts',(-2.11117921729541,-7.6240962292235,141.056190442262));
#54199=CARTESIAN_POINT('Ctrl Pts',(-2.29813520646132,-7.57232647356865,
141.048358866128));
#54200=CARTESIAN_POINT('Ctrl Pts',(-2.48342356625144,-7.5136100046007,141.040527289995));
#54201=CARTESIAN_POINT('Ctrl Pts',(-2.66648551247275,-7.44807196607101,
141.032695713861));
#54202=CARTESIAN_POINT('Ctrl Pts',(-2.84937838515238,-7.38259445758877,
141.024871370865));
#54203=CARTESIAN_POINT('Ctrl Pts',(-3.03004861066099,-7.31030804406366,
141.01704702787));
#54204=CARTESIAN_POINT('Ctrl Pts',(-3.20795014846785,-7.23138830688445,
141.009222684874));
#54205=CARTESIAN_POINT('Ctrl Pts',(-3.38572195238176,-7.15252612156713,
141.001404047745));
#54206=CARTESIAN_POINT('Ctrl Pts',(-3.56072877009257,-7.06704038916747,
140.993585410616));
#54207=CARTESIAN_POINT('Ctrl Pts',(-3.73244203572983,-6.97515572943837,
140.985766773487));
#54208=CARTESIAN_POINT('Ctrl Pts',(-3.90406343920261,-6.8833202256303,140.977952319127));
#54209=CARTESIAN_POINT('Ctrl Pts',(-4.07239449130314,-6.7850927792193,140.970137864768));
#54210=CARTESIAN_POINT('Ctrl Pts',(-4.2369286752944,-6.68074519799012,140.962323410408));
#54211=CARTESIAN_POINT('Ctrl Pts',(-4.40140679431659,-6.57643317316492,
140.954511618821));
#54212=CARTESIAN_POINT('Ctrl Pts',(-4.56209032647814,-6.4660053567526,140.946699827233));
#54213=CARTESIAN_POINT('Ctrl Pts',(-4.71849917888739,-6.34977846061097,
140.938888035646));
#54214=CARTESIAN_POINT('Ctrl Pts',(-4.87491535148405,-6.23354612486251,
140.931075878455));
#54215=CARTESIAN_POINT('Ctrl Pts',(-5.02705615694601,-6.11151436953882,
140.923263721263));
#54216=CARTESIAN_POINT('Ctrl Pts',(-5.17447180221511,-5.9840423267287,140.915451564072));
#54217=CARTESIAN_POINT('Ctrl Pts',(-5.32189949884725,-5.85655986296319,
140.907638768229));
#54218=CARTESIAN_POINT('Ctrl Pts',(-5.46460099908586,-5.72363645529987,
140.899825972386));
#54219=CARTESIAN_POINT('Ctrl Pts',(-5.60216090650573,-5.58567043224168,
140.892013176544));
#54220=CARTESIAN_POINT('Ctrl Pts',(-5.73975626441959,-5.44766885402963,
140.88419836727));
#54221=CARTESIAN_POINT('Ctrl Pts',(-5.87220714147425,-5.3046223206498,140.876383557995));
#54222=CARTESIAN_POINT('Ctrl Pts',(-5.99913610811226,-5.15696489772266,
140.868568748721));
#54223=CARTESIAN_POINT('Ctrl Pts',(-6.12612012169816,-5.00924343826642,
140.860750550296));
#54224=CARTESIAN_POINT('Ctrl Pts',(-6.24757722533467,-4.85690737227738,
140.852932351871));
#54225=CARTESIAN_POINT('Ctrl Pts',(-6.36317117017967,-4.70042271067127,
140.845114153446));
#54226=CARTESIAN_POINT('Ctrl Pts',(-6.47889966575044,-4.54375590176654,
140.837286854681));
#54227=CARTESIAN_POINT('Ctrl Pts',(-6.58875116277602,-4.38293113545497,
140.829459555915));
#54228=CARTESIAN_POINT('Ctrl Pts',(-6.69243294611102,-4.21844310875563,
140.82163225715));
#54229=CARTESIAN_POINT('Ctrl Pts',(-6.79618241333639,-4.05384770360262,
140.813799848692));
#54230=CARTESIAN_POINT('Ctrl Pts',(-6.89375396476075,-3.88558457557204,
140.805967440234));
#54231=CARTESIAN_POINT('Ctrl Pts',(-6.98490150243916,-3.71417177863695,
140.798135031776));
#54232=CARTESIAN_POINT('Ctrl Pts',(-7.07617984967847,-3.54251298018309,
140.790291382708));
#54233=CARTESIAN_POINT('Ctrl Pts',(-7.16101561659004,-3.36769579977956,
140.78244773364));
#54234=CARTESIAN_POINT('Ctrl Pts',(-7.23921091056943,-3.19025804478142,
140.774604084572));
#54235=CARTESIAN_POINT('Ctrl Pts',(-7.28139996368055,-3.09452426735603,
140.770372165868));
#54236=CARTESIAN_POINT('Ctrl Pts',(-7.32165685034114,-2.99802791882006,
140.766140247165));
#54237=CARTESIAN_POINT('Ctrl Pts',(-7.35995658780249,-2.90085505078464,
140.761908328462));
#54238=CARTESIAN_POINT('Ctrl Pts',(-7.44302986567066,-2.69008418908618,
140.752729170022));
#54239=CARTESIAN_POINT('Ctrl Pts',(-7.51709701138963,-2.47561178123072,
140.743550011582));
#54240=CARTESIAN_POINT('Ctrl Pts',(-7.58186242813559,-2.25815923283232,
140.734370853142));
#54241=CARTESIAN_POINT('Ctrl Pts',(-7.64626385011824,-2.04192881181091,
140.725243283432));
#54242=CARTESIAN_POINT('Ctrl Pts',(-7.70146774048433,-1.82275176528591,
140.716115713722));
#54243=CARTESIAN_POINT('Ctrl Pts',(-7.74722959436371,-1.6013602381148,140.706988144012));
#54244=CARTESIAN_POINT('Ctrl Pts',(-7.79280697487484,-1.38086117567706,
140.697897368999));
#54245=CARTESIAN_POINT('Ctrl Pts',(-7.82901820197523,-1.15816555753905,
140.688806593986));
#54246=CARTESIAN_POINT('Ctrl Pts',(-7.8556687641481,-0.934017809245542,
140.679715818973));
#54247=CARTESIAN_POINT('Ctrl Pts',(-7.88213558553228,-0.711415434884059,
140.670687719792));
#54248=CARTESIAN_POINT('Ctrl Pts',(-7.89917304269829,-0.487381005202657,
140.661659620611));
#54249=CARTESIAN_POINT('Ctrl Pts',(-7.9066383030024,-0.262662798080353,
140.65263152143));
#54250=CARTESIAN_POINT('Ctrl Pts',(-7.90947730148492,-0.177203668321175,
140.649198183699));
#54251=CARTESIAN_POINT('Ctrl Pts',(-7.9109324306235,-0.0916458368497545,
140.645764845968));
#54252=CARTESIAN_POINT('Ctrl Pts',(-7.91099770101101,-0.00603113576254674,
140.642331508237));
#54253=CARTESIAN_POINT('',(-7.90671737907022,0.00501511144919005,138.642331508237));
#54254=CARTESIAN_POINT('Ctrl Pts',(-7.911,7.88147325181399E-12,140.642331508237));
#54255=CARTESIAN_POINT('Ctrl Pts',(-7.91099999999781,2.20167589667468,140.553744072504));
#54256=CARTESIAN_POINT('Ctrl Pts',(-6.94214576671932,4.3861041833938,140.465156636771));
#54257=CARTESIAN_POINT('Ctrl Pts',(-3.67820201487544,7.34180684108005,140.287981765306));
#54258=CARTESIAN_POINT('Ctrl Pts',(-1.40868175870923,8.0899266657148,140.199394329573));
#54259=CARTESIAN_POINT('Ctrl Pts',(2.97309270522057,7.65454228024954,140.022219458108));
#54260=CARTESIAN_POINT('Ctrl Pts',(5.05102072676267,6.47444880833708,139.933632022375));
#54261=CARTESIAN_POINT('Ctrl Pts',(7.66951518848175,2.93425195366915,139.756457150909));
#54262=CARTESIAN_POINT('Ctrl Pts',(8.18956872247135,0.601881960090677,139.667869715177));
#54263=CARTESIAN_POINT('Ctrl Pts',(7.32306689760956,-3.71537198233214,139.490694843711));
#54264=CARTESIAN_POINT('Ctrl Pts',(5.94329958849609,-5.66643518937134,139.402107407979));
#54265=CARTESIAN_POINT('Ctrl Pts',(2.16154501637013,-7.92205913233226,139.224932536513));
#54266=CARTESIAN_POINT('Ctrl Pts',(-0.210816529309054,-8.20894963712981,
139.13634510078));
#54267=CARTESIAN_POINT('Ctrl Pts',(-4.42123908577174,-6.91982244717361,
138.959170229315));
#54268=CARTESIAN_POINT('Ctrl Pts',(-6.22631625634761,-5.35390358802856,
138.870582793582));
#54269=CARTESIAN_POINT('Ctrl Pts',(-7.65317280859725,-2.31334857513722,
138.735440741312));
#54270=CARTESIAN_POINT('Ctrl Pts',(-7.91100000000113,-1.15702837835722,
138.688886124774));
#54271=CARTESIAN_POINT('Ctrl Pts',(-7.911,7.71105401753402E-12,138.642331508237));
#54272=CARTESIAN_POINT('',(-7.92070690004078,0.000688450382506796,136.642332689193));
#54273=CARTESIAN_POINT('Ctrl Pts',(-7.90399247642154,0.00820607573821075,
138.642331508237));
#54274=CARTESIAN_POINT('Ctrl Pts',(-7.91040497386928,0.880579291061528,
138.60731645636));
#54275=CARTESIAN_POINT('Ctrl Pts',(-7.37502394767783,4.3833748071562,138.466367024682));
#54276=CARTESIAN_POINT('Ctrl Pts',(-3.34421556203096,8.05994887033659,138.272450403101));
#54277=CARTESIAN_POINT('Ctrl Pts',(2.08882747359352,7.95366654480699,138.060581643496));
#54278=CARTESIAN_POINT('Ctrl Pts',(6.87299752086058,5.37665868323933,137.848712883892));
#54279=CARTESIAN_POINT('Ctrl Pts',(9.20038080623976,-1.70147935996806,137.583876934383));
#54280=CARTESIAN_POINT('Ctrl Pts',(3.54223654011048,-8.65913268958539,137.266073794978));
#54281=CARTESIAN_POINT('Ctrl Pts',(-5.24241200874194,-7.67706431858937,
136.952225856877));
#54282=CARTESIAN_POINT('Ctrl Pts',(-7.91663072399812,-2.52296611631306,
136.744312298581));
#54283=CARTESIAN_POINT('Ctrl Pts',(-7.92424864988173,0.000678108123123556,
136.642333120087));
#54284=CARTESIAN_POINT('',(-7.90858822339541,-0.00709720147611503,134.642331508237));
#54285=CARTESIAN_POINT('Ctrl Pts',(-7.91099996752649,0.000716795584281833,
136.642331508237));
#54286=CARTESIAN_POINT('Ctrl Pts',(-7.91099111508014,0.0984178756964286,
136.638376844212));
#54287=CARTESIAN_POINT('Ctrl Pts',(-7.90917241970919,0.196100735934578,
136.634422180187));
#54288=CARTESIAN_POINT('Ctrl Pts',(-7.90554545851632,0.293720961682897,
136.630467516162));
#54289=CARTESIAN_POINT('Ctrl Pts',(-7.89835480577871,0.487258500740033,
136.622627174293));
#54290=CARTESIAN_POINT('Ctrl Pts',(-7.88404199044287,0.680822908395119,
136.614786832423));
#54291=CARTESIAN_POINT('Ctrl Pts',(-7.862589869426,0.873842975138913,136.606946490554));
#54292=CARTESIAN_POINT('Ctrl Pts',(-7.84116173251893,1.06664723970303,136.599114914421));
#54293=CARTESIAN_POINT('Ctrl Pts',(-7.81261022220641,1.25890802941457,136.591283338287));
#54294=CARTESIAN_POINT('Ctrl Pts',(-7.77697017092517,1.45005377849934,136.583451762153));
#54295=CARTESIAN_POINT('Ctrl Pts',(-7.74136303631394,1.64102298795184,136.575627419158));
#54296=CARTESIAN_POINT('Ctrl Pts',(-7.69868046261918,1.8308788645228,136.567803076162));
#54297=CARTESIAN_POINT('Ctrl Pts',(-7.64900910350115,2.01905441594737,136.559978733166));
#54298=CARTESIAN_POINT('Ctrl Pts',(-7.59937396699795,2.20709274119893,136.552160096037));
#54299=CARTESIAN_POINT('Ctrl Pts',(-7.54276028534159,2.39345284352173,136.544341458909));
#54300=CARTESIAN_POINT('Ctrl Pts',(-7.47930590308153,2.57757719731723,136.53652282178));
#54301=CARTESIAN_POINT('Ctrl Pts',(-7.41588546727722,2.76160304933861,136.52870836742));
#54302=CARTESIAN_POINT('Ctrl Pts',(-7.34563173519456,2.94339520389513,136.52089391306));
#54303=CARTESIAN_POINT('Ctrl Pts',(-7.26873264174794,3.12241041229177,136.5130794587));
#54304=CARTESIAN_POINT('Ctrl Pts',(-7.19185975164176,3.30136462131586,136.505267667113));
#54305=CARTESIAN_POINT('Ctrl Pts',(-7.10834615052097,3.47754344687064,136.497455875526));
#54306=CARTESIAN_POINT('Ctrl Pts',(-7.01842830329717,3.65042259902566,136.489644083939));
#54307=CARTESIAN_POINT('Ctrl Pts',(-6.92850624777322,3.82330984220358,136.481831926747));
#54308=CARTESIAN_POINT('Ctrl Pts',(-6.83217950146916,3.99289678728025,136.474019769556));
#54309=CARTESIAN_POINT('Ctrl Pts',(-6.72973122239094,4.15868232429173,136.466207612364));
#54310=CARTESIAN_POINT('Ctrl Pts',(-6.62727456807317,4.32448141442095,136.458394816522));
#54311=CARTESIAN_POINT('Ctrl Pts',(-6.51869556836926,4.48647817765456,136.450582020679));
#54312=CARTESIAN_POINT('Ctrl Pts',(-6.40432154194982,4.6441992406999,136.442769224837));
#54313=CARTESIAN_POINT('Ctrl Pts',(-6.2899180402582,4.80196094996018,136.434954415562));
#54314=CARTESIAN_POINT('Ctrl Pts',(-6.16971674319755,4.95544447913854,136.427139606288));
#54315=CARTESIAN_POINT('Ctrl Pts',(-6.044086281573,5.10420826582351,136.419324797014));
#54316=CARTESIAN_POINT('Ctrl Pts',(-5.91840133613917,5.25303656885011,136.411506598589));
#54317=CARTESIAN_POINT('Ctrl Pts',(-5.78728276248387,5.39714078345749,136.403688400164));
#54318=CARTESIAN_POINT('Ctrl Pts',(-5.65113727012219,5.53611493325743,136.395870201739));
#54319=CARTESIAN_POINT('Ctrl Pts',(-5.51483330514526,5.67525084821456,136.388042902974));
#54320=CARTESIAN_POINT('Ctrl Pts',(-5.37349098096021,5.80924452064656,136.380215604208));
#54321=CARTESIAN_POINT('Ctrl Pts',(-5.22755224155258,5.93772840081446,136.372388305443));
#54322=CARTESIAN_POINT('Ctrl Pts',(-5.08151823274156,6.06629615578254,136.364555896985));
#54323=CARTESIAN_POINT('Ctrl Pts',(-4.93088210049844,6.18934672898214,136.356723488527));
#54324=CARTESIAN_POINT('Ctrl Pts',(-4.7761162513342,6.30655488787193,136.348891080069));
#54325=CARTESIAN_POINT('Ctrl Pts',(-4.62112829136721,6.42393125698639,136.341047431001));
#54326=CARTESIAN_POINT('Ctrl Pts',(-4.4619990639663,6.53544826420216,136.333203781933));
#54327=CARTESIAN_POINT('Ctrl Pts',(-4.29922813247562,6.64082513434364,136.325360132865));
#54328=CARTESIAN_POINT('Ctrl Pts',(-4.2114076112622,6.69767958356815,136.321128214161));
#54329=CARTESIAN_POINT('Ctrl Pts',(-4.12252740358087,6.75274745884198,136.316896295458));
#54330=CARTESIAN_POINT('Ctrl Pts',(-4.03266850263118,6.80599043107514,136.312664376754));
#54331=CARTESIAN_POINT('Ctrl Pts',(-3.86454603947509,6.90560593430282,136.304746623602));
#54332=CARTESIAN_POINT('Ctrl Pts',(-3.6924939819573,6.99912829698076,136.296828870449));
#54333=CARTESIAN_POINT('Ctrl Pts',(-3.51699275295656,7.0862319306985,136.288911117296));
#54334=CARTESIAN_POINT('Ctrl Pts',(-3.34169316224011,7.17323548860847,136.281002461072));
#54335=CARTESIAN_POINT('Ctrl Pts',(-3.16295259883223,7.2538348549971,136.273093804848));
#54336=CARTESIAN_POINT('Ctrl Pts',(-2.981279617994,7.32774814246052,136.265185148623));
#54337=CARTESIAN_POINT('Ctrl Pts',(-2.79978173613478,7.40159019125592,136.257284114873));
#54338=CARTESIAN_POINT('Ctrl Pts',(-2.6153573838318,7.468758869378,136.249383081124));
#54339=CARTESIAN_POINT('Ctrl Pts',(-2.4285390862048,7.52901845573349,136.241482047374));
#54340=CARTESIAN_POINT('Ctrl Pts',(-2.24186627611685,7.58923111403626,136.233587166672));
#54341=CARTESIAN_POINT('Ctrl Pts',(-2.05280356129854,7.64254529511686,136.22569228597));
#54342=CARTESIAN_POINT('Ctrl Pts',(-1.86190305875275,7.68877350425978,136.217797405268));
#54343=CARTESIAN_POINT('Ctrl Pts',(-1.67111590581146,7.7349742648148,136.209907212252));
#54344=CARTESIAN_POINT('Ctrl Pts',(-1.47849347330298,7.77409735625623,136.202017019236));
#54345=CARTESIAN_POINT('Ctrl Pts',(-1.28460291636169,7.8060051465058,136.19412682622));
#54346=CARTESIAN_POINT('Ctrl Pts',(-1.09079162088131,7.83789989301508,136.186239858675));
#54347=CARTESIAN_POINT('Ctrl Pts',(-0.895713573480848,7.86258516091987,
136.178352891129));
#54348=CARTESIAN_POINT('Ctrl Pts',(-0.699946279108443,7.87997437853463,
136.170465923584));
#54349=CARTESIAN_POINT('Ctrl Pts',(-0.504195985789498,7.89736208601452,
136.162579640967));
#54350=CARTESIAN_POINT('Ctrl Pts',(-0.307756907132425,7.90745496869302,
136.154693358351));
#54351=CARTESIAN_POINT('Ctrl Pts',(-0.111212357335414,7.91021825309365,
136.146807075735));
#54352=CARTESIAN_POINT('Ctrl Pts',(0.0853318470066554,7.91298153263741,
136.138920806979));
#54353=CARTESIAN_POINT('Ctrl Pts',(0.281981177578248,7.90841523417769,136.131034538224));
#54354=CARTESIAN_POINT('Ctrl Pts',(0.478151515600098,7.89653671732927,136.123148269469));
#54355=CARTESIAN_POINT('Ctrl Pts',(0.674354387994053,7.88465623045781,136.115260692796));
#54356=CARTESIAN_POINT('Ctrl Pts',(0.870077765617847,7.86546112963606,136.107373116122));
#54357=CARTESIAN_POINT('Ctrl Pts',(1.06474159487503,7.83902075109787,136.099485539449));
#54358=CARTESIAN_POINT('Ctrl Pts',(1.25947033545747,7.81257155592426,136.091595332636));
#54359=CARTESIAN_POINT('Ctrl Pts',(1.45313848250933,7.7788723156153,136.083705125822));
#54360=CARTESIAN_POINT('Ctrl Pts',(1.64517487955874,7.73804372019627,136.075814919009));
#54361=CARTESIAN_POINT('Ctrl Pts',(1.83739671872727,7.69717569818222,136.067917092929));
#54362=CARTESIAN_POINT('Ctrl Pts',(2.02798332339201,7.64916464147595,136.060019266848));
#54363=CARTESIAN_POINT('Ctrl Pts',(2.21637641015455,7.59418176030245,136.052121440767));
#54364=CARTESIAN_POINT('Ctrl Pts',(2.40487381372971,7.53916843406851,136.044219241511));
#54365=CARTESIAN_POINT('Ctrl Pts',(2.59117495151574,7.47717569490734,136.036317042255));
#54366=CARTESIAN_POINT('Ctrl Pts',(2.77474002911661,7.40842350104379,136.028414842999));
#54367=CARTESIAN_POINT('Ctrl Pts',(2.95852668368397,7.33958831806949,136.020503105189));
#54368=CARTESIAN_POINT('Ctrl Pts',(3.13957036413097,7.26397751525178,136.012591367379));
#54369=CARTESIAN_POINT('Ctrl Pts',(3.31735346046525,7.18185818701116,136.004679629569));
#54370=CARTESIAN_POINT('Ctrl Pts',(3.39089584404692,7.14788841563545,136.001406832162));
#54371=CARTESIAN_POINT('Ctrl Pts',(3.46388059569693,7.11280545460241,135.998134034754));
#54372=CARTESIAN_POINT('Ctrl Pts',(3.53627246584339,7.07663041618806,135.994861237346));
#54373=CARTESIAN_POINT('Ctrl Pts',(3.72019096729623,6.98472425543122,135.986546381085));
#54374=CARTESIAN_POINT('Ctrl Pts',(3.90068215448687,6.88556557792565,135.978231524823));
#54375=CARTESIAN_POINT('Ctrl Pts',(4.07716969805466,6.77942536305732,135.969916668562));
#54376=CARTESIAN_POINT('Ctrl Pts',(4.25343990334744,6.67341585617406,135.961612051757));
#54377=CARTESIAN_POINT('Ctrl Pts',(4.42571604825334,6.5604421096607,135.953307434951));
#54378=CARTESIAN_POINT('Ctrl Pts',(4.59344533142924,6.44082145282501,135.945002818146));
#54379=CARTESIAN_POINT('Ctrl Pts',(4.76097912543036,6.3213402143607,135.936707880407));
#54380=CARTESIAN_POINT('Ctrl Pts',(4.92397638964062,6.19522768689238,135.928412942667));
#54381=CARTESIAN_POINT('Ctrl Pts',(5.08191160489734,6.06284549036257,135.920118004927));
#54382=CARTESIAN_POINT('Ctrl Pts',(5.23961010463231,5.93066171013067,135.911835499756));
#54383=CARTESIAN_POINT('Ctrl Pts',(5.39226147249852,5.79222720192398,135.903552994586));
#54384=CARTESIAN_POINT('Ctrl Pts',(5.53937162988225,5.64794501974441,135.895270489416));
#54385=CARTESIAN_POINT('Ctrl Pts',(5.68634664563341,5.50379538129939,135.886995592906));
#54386=CARTESIAN_POINT('Ctrl Pts',(5.82779039332744,5.3538089859626,135.878720696396));
#54387=CARTESIAN_POINT('Ctrl Pts',(5.96324280045138,5.19842825312274,135.870445799886));
#54388=CARTESIAN_POINT('Ctrl Pts',(6.09854026778757,5.04322525546144,135.862180368773));
#54389=CARTESIAN_POINT('Ctrl Pts',(6.22785987768987,4.88264045350778,135.853914937659));
#54390=CARTESIAN_POINT('Ctrl Pts',(6.35077908591578,4.71715231913225,135.845649506546));
#54391=CARTESIAN_POINT('Ctrl Pts',(6.39881317348746,4.6524832437827,135.842419560245));
#54392=CARTESIAN_POINT('Ctrl Pts',(6.44587027874722,4.58706578330995,135.839189613944));
#54393=CARTESIAN_POINT('Ctrl Pts',(6.49192678752703,4.52092994696766,135.835959667643));
#54394=CARTESIAN_POINT('Ctrl Pts',(6.60980161422419,4.35166504926146,135.827693097498));
#54395=CARTESIAN_POINT('Ctrl Pts',(6.72098648933855,4.17788312753284,135.819426527353));
#54396=CARTESIAN_POINT('Ctrl Pts',(6.82516088355226,4.00013748684069,135.811159957208));
#54397=CARTESIAN_POINT('Ctrl Pts',(6.9294286192295,3.82223258399623,135.80288598012));
#54398=CARTESIAN_POINT('Ctrl Pts',(7.02667318534892,3.64035712532824,135.794612003032));
#54399=CARTESIAN_POINT('Ctrl Pts',(7.11662041098348,3.45508826601772,135.786338025945));
#54400=CARTESIAN_POINT('Ctrl Pts',(7.20665406874608,3.26964137807256,135.778056098223));
#54401=CARTESIAN_POINT('Ctrl Pts',(7.28937625859859,3.08079484345056,135.769774170502));
#54402=CARTESIAN_POINT('Ctrl Pts',(7.36456093580272,2.88914576005582,135.76149224278));
#54403=CARTESIAN_POINT('Ctrl Pts',(7.43987024045673,2.69717899575291,135.753196586789));
#54404=CARTESIAN_POINT('Ctrl Pts',(7.5076169457623,2.50240066888266,135.744900930798));
#54405=CARTESIAN_POINT('Ctrl Pts',(7.56762425173167,2.30542494664274,135.736605274807));
#54406=CARTESIAN_POINT('Ctrl Pts',(7.62768579269254,2.10827119647023,135.728302121148));
#54407=CARTESIAN_POINT('Ctrl Pts',(7.67999389271445,1.90891636903003,135.719998967489));
#54408=CARTESIAN_POINT('Ctrl Pts',(7.72442260553246,1.70798606877784,135.711695813831));
#54409=CARTESIAN_POINT('Ctrl Pts',(7.76891905599974,1.50674942280136,135.703380000879));
#54410=CARTESIAN_POINT('Ctrl Pts',(7.8055120496907,1.30393279076379,135.695064187926));
#54411=CARTESIAN_POINT('Ctrl Pts',(7.83412706679606,1.10017003290101,135.686748374974));
#54412=CARTESIAN_POINT('Ctrl Pts',(7.84524193292429,1.02102292747637,135.683518282629));
#54413=CARTESIAN_POINT('Ctrl Pts',(7.85515366939065,0.941733108081712,135.680288190284));
#54414=CARTESIAN_POINT('Ctrl Pts',(7.86386002732667,0.862337793798822,135.677058097939));
#54415=CARTESIAN_POINT('Ctrl Pts',(7.8851831639089,0.667887124198026,135.669147132095));
#54416=CARTESIAN_POINT('Ctrl Pts',(7.89931662002861,0.472399687478545,135.661236166252));
#54417=CARTESIAN_POINT('Ctrl Pts',(7.90616827704328,0.276449226937729,135.653325200409));
#54418=CARTESIAN_POINT('Ctrl Pts',(7.91301300081428,0.0806970501535383,
135.645422239732));
#54419=CARTESIAN_POINT('Ctrl Pts',(7.91259059119092,-0.115516875670679,
135.637519279055));
#54420=CARTESIAN_POINT('Ctrl Pts',(7.90486046843095,-0.311611897458337,
135.629616318378));
#54421=CARTESIAN_POINT('Ctrl Pts',(7.89713673729206,-0.507544778861777,
135.621719892233));
#54422=CARTESIAN_POINT('Ctrl Pts',(7.8821173439548,-0.703358609790985,135.613823466087));
#54423=CARTESIAN_POINT('Ctrl Pts',(7.85981370664763,-0.89847064325665,135.605927039942));
#54424=CARTESIAN_POINT('Ctrl Pts',(7.83752438459008,-1.09345744703786,135.598035681997));
#54425=CARTESIAN_POINT('Ctrl Pts',(7.80796017272988,-1.28774300978114,135.590144324053));
#54426=CARTESIAN_POINT('Ctrl Pts',(7.77118448809304,-1.48074732889246,135.582252966108));
#54427=CARTESIAN_POINT('Ctrl Pts',(7.73442560479834,-1.67366347203555,135.57436521341));
#54428=CARTESIAN_POINT('Ctrl Pts',(7.69046187840374,-1.86529920028309,135.566477460711));
#54429=CARTESIAN_POINT('Ctrl Pts',(7.63940826737231,-2.05508207242525,135.558589708013));
#54430=CARTESIAN_POINT('Ctrl Pts',(7.58836853844377,-2.24481334027724,135.550704100091));
#54431=CARTESIAN_POINT('Ctrl Pts',(7.53024285678663,-2.43269242390119,135.54281849217));
#54432=CARTESIAN_POINT('Ctrl Pts',(7.46519681095899,-2.61815919562729,135.534932884248));
#54433=CARTESIAN_POINT('Ctrl Pts',(7.40014309351457,-2.80364784155004,135.527046346287));
#54434=CARTESIAN_POINT('Ctrl Pts',(7.32816748864173,-2.98672327972482,135.519159808327));
#54435=CARTESIAN_POINT('Ctrl Pts',(7.24948499505314,-3.16684200845248,135.511273270366));
#54436=CARTESIAN_POINT('Ctrl Pts',(7.17079258895755,-3.34698342873552,135.503385738851));
#54437=CARTESIAN_POINT('Ctrl Pts',(7.0853917478297,-3.5241670811841,135.495498207335));
#54438=CARTESIAN_POINT('Ctrl Pts',(6.99354501429168,-3.69787089188846,135.48761067582));
#54439=CARTESIAN_POINT('Ctrl Pts',(6.90167131522661,-3.87162570075711,135.479720828583));
#54440=CARTESIAN_POINT('Ctrl Pts',(6.80334811350886,-4.04189832734603,135.471830981346));
#54441=CARTESIAN_POINT('Ctrl Pts',(6.69888327813029,-4.20819246541629,135.46394113411));
#54442=CARTESIAN_POINT('Ctrl Pts',(6.59437026273732,-4.37456329966796,135.456047648012));
#54443=CARTESIAN_POINT('Ctrl Pts',(6.48371015218338,-4.5369516974449,135.448154161915));
#54444=CARTESIAN_POINT('Ctrl Pts',(6.36725351846449,-4.69489122681257,135.440260675818));
#54445=CARTESIAN_POINT('Ctrl Pts',(6.2506622610382,-4.85301333405757,135.432358064862));
#54446=CARTESIAN_POINT('Ctrl Pts',(6.12826130060803,-5.00667602300382,135.424455453906));
#54447=CARTESIAN_POINT('Ctrl Pts',(6.00044153449429,-5.15544589643959,135.41655284295));
#54448=CARTESIAN_POINT('Ctrl Pts',(5.87253699134649,-5.30431444216221,135.408644990551));
#54449=CARTESIAN_POINT('Ctrl Pts',(5.73920671084679,-5.44828345092031,135.400737138153));
#54450=CARTESIAN_POINT('Ctrl Pts',(5.60087783257149,-5.58695699863613,135.392829285755));
#54451=CARTESIAN_POINT('Ctrl Pts',(5.46235968115648,-5.72582029109722,135.384910613171));
#54452=CARTESIAN_POINT('Ctrl Pts',(5.31882952213985,-5.85937341628803,135.376991940588));
#54453=CARTESIAN_POINT('Ctrl Pts',(5.17074776761939,-5.98726051910714,135.369073268005));
#54454=CARTESIAN_POINT('Ctrl Pts',(5.10954590674255,-6.04011597520315,135.36580049818));
#54455=CARTESIAN_POINT('Ctrl Pts',(5.04756691244677,-6.09200409841252,135.362527728355));
#54456=CARTESIAN_POINT('Ctrl Pts',(4.98484468130388,-6.14290196106664,135.35925495853));
#54457=CARTESIAN_POINT('Ctrl Pts',(4.83453200360936,-6.26487775633198,135.351411825612));
#54458=CARTESIAN_POINT('Ctrl Pts',(4.67950387729446,-6.38152445229471,135.343568692693));
#54459=CARTESIAN_POINT('Ctrl Pts',(4.52017677883435,-6.49245122338911,135.335725559774));
#54460=CARTESIAN_POINT('Ctrl Pts',(4.36103679309332,-6.60324772279741,135.32789163778));
#54461=CARTESIAN_POINT('Ctrl Pts',(4.19760817327514,-6.70833747434412,135.320057715786));
#54462=CARTESIAN_POINT('Ctrl Pts',(4.03034210722823,-6.80736832400768,135.312223793792));
#54463=CARTESIAN_POINT('Ctrl Pts',(3.86323994700134,-6.90630213227483,135.304397548342));
#54464=CARTESIAN_POINT('Ctrl Pts',(3.6923081291256,-6.99918868440921,135.296571302893));
#54465=CARTESIAN_POINT('Ctrl Pts',(3.51802876084143,-7.0857176515786,135.288745057443));
#54466=CARTESIAN_POINT('Ctrl Pts',(3.34388629639326,-7.17217864657407,135.280924959842));
#54467=CARTESIAN_POINT('Ctrl Pts',(3.16640183223815,-7.25229184785456,135.27310486224));
#54468=CARTESIAN_POINT('Ctrl Pts',(2.98608431467643,-7.32579152485541,135.265284764638));
#54469=CARTESIAN_POINT('Ctrl Pts',(2.80587341029001,-7.39924774499165,135.257469290689));
#54470=CARTESIAN_POINT('Ctrl Pts',(2.6228331137715,-7.46609809773762,135.249653816739));
#54471=CARTESIAN_POINT('Ctrl Pts',(2.43749488034718,-7.52612381696457,135.241838342789));
#54472=CARTESIAN_POINT('Ctrl Pts',(2.25223022907008,-7.58612570505194,135.234025971703));
#54473=CARTESIAN_POINT('Ctrl Pts',(2.06466979255896,-7.63930824978848,135.226213600618));
#54474=CARTESIAN_POINT('Ctrl Pts',(1.87536299592791,-7.68550158633152,135.218401229532));
#54475=CARTESIAN_POINT('Ctrl Pts',(1.68606336523435,-7.73169317429201,135.210589154172));
#54476=CARTESIAN_POINT('Ctrl Pts',(1.49501784547347,-7.77089598903363,135.202777078813));
#54477=CARTESIAN_POINT('Ctrl Pts',(1.30278940599468,-7.80299050131602,135.194965003453));
#54478=CARTESIAN_POINT('Ctrl Pts',(1.11055534443338,-7.83508595226283,135.187152699615));
#54479=CARTESIAN_POINT('Ctrl Pts',(0.917138641137321,-7.8600726279092,135.179340395776));
#54480=CARTESIAN_POINT('Ctrl Pts',(0.723110773275259,-7.87788244451345,
135.171528091938));
#54481=CARTESIAN_POINT('Ctrl Pts',(0.529043090878745,-7.89569591569354,
135.163714185014));
#54482=CARTESIAN_POINT('Ctrl Pts',(0.3343643443826,-7.9063295619679,135.15590027809));
#54483=CARTESIAN_POINT('Ctrl Pts',(0.139649580975725,-7.90976731608037,
135.148086371167));
#54484=CARTESIAN_POINT('Ctrl Pts',(-0.0551394010230107,-7.91320638054685,
135.140269485849));
#54485=CARTESIAN_POINT('Ctrl Pts',(-0.249964075889232,-7.90944408307697,
135.132452600532));
#54486=CARTESIAN_POINT('Ctrl Pts',(-0.444250795860102,-7.89851645756199,
135.124635715215));
#54487=CARTESIAN_POINT('Ctrl Pts',(-0.638748275819347,-7.88757697788516,
135.116810350231));
#54488=CARTESIAN_POINT('Ctrl Pts',(-0.832706284084506,-7.86945666540598,
135.108984985247));
#54489=CARTESIAN_POINT('Ctrl Pts',(-1.02555662959735,-7.84424340516591,
135.101159620263));
#54490=CARTESIAN_POINT('Ctrl Pts',(-1.21852418100588,-7.81901482142336,
135.093329499369));
#54491=CARTESIAN_POINT('Ctrl Pts',(-1.41038238231514,-7.78668475716327,
135.085499378474));
#54492=CARTESIAN_POINT('Ctrl Pts',(-1.60057451687288,-7.74739196219845,
135.07766925758));
#54493=CARTESIAN_POINT('Ctrl Pts',(-1.79102663147558,-7.70804545658663,
135.06982843343));
#54494=CARTESIAN_POINT('Ctrl Pts',(-1.97980779030585,-7.66171729424447,
135.061987609279));
#54495=CARTESIAN_POINT('Ctrl Pts',(-2.16637658307278,-7.60859602688393,
135.054146785128));
#54496=CARTESIAN_POINT('Ctrl Pts',(-2.26706686920622,-7.57992673267359,
135.049915129793));
#54497=CARTESIAN_POINT('Ctrl Pts',(-2.36711309001969,-7.54927964076426,
135.045683474458));
#54498=CARTESIAN_POINT('Ctrl Pts',(-2.466432769271,-7.51669012229892,135.041451819124));
#54499=CARTESIAN_POINT('Ctrl Pts',(-2.65211313201021,-7.45576328830433,
135.033540644787));
#54500=CARTESIAN_POINT('Ctrl Pts',(-2.83578417829544,-7.38787034295405,
135.025629470451));
#54501=CARTESIAN_POINT('Ctrl Pts',(-3.01688532541028,-7.31316100830032,
135.017718296115));
#54502=CARTESIAN_POINT('Ctrl Pts',(-3.19779013536897,-7.238532668265,135.009815698519));
#54503=CARTESIAN_POINT('Ctrl Pts',(-3.37613027977014,-7.15710278872621,
135.001913100922));
#54504=CARTESIAN_POINT('Ctrl Pts',(-3.55135982482645,-7.06907097111131,
134.994010503326));
#54505=CARTESIAN_POINT('Ctrl Pts',(-3.72643192580988,-6.98111825024865,
134.986115006229));
#54506=CARTESIAN_POINT('Ctrl Pts',(-3.89839868890227,-6.88657556191102,
134.978219509131));
#54507=CARTESIAN_POINT('Ctrl Pts',(-4.06673342096132,-6.78569084786776,
134.970324012034));
#54508=CARTESIAN_POINT('Ctrl Pts',(-4.234948141876,-6.68487805772181,134.962434143885));
#54509=CARTESIAN_POINT('Ctrl Pts',(-4.39953569613678,-6.57773242665006,
134.954544275737));
#54510=CARTESIAN_POINT('Ctrl Pts',(-4.55999305689652,-6.46454826890909,
134.946654407588));
#54511=CARTESIAN_POINT('Ctrl Pts',(-4.72036579199413,-6.35142380481038,
134.938768700579));
#54512=CARTESIAN_POINT('Ctrl Pts',(-4.87661239299423,-6.23226735835444,
134.930882993569));
#54513=CARTESIAN_POINT('Ctrl Pts',(-5.02825771881472,-6.10741723752194,
134.922997286559));
#54514=CARTESIAN_POINT('Ctrl Pts',(-5.17985119644617,-5.98260980348268,
134.915114275706));
#54515=CARTESIAN_POINT('Ctrl Pts',(-5.326846268445,-5.85211279380975,134.907231264854));
#54516=CARTESIAN_POINT('Ctrl Pts',(-5.46879965459889,-5.71630574216067,
134.899348254001));
#54517=CARTESIAN_POINT('Ctrl Pts',(-5.61075515919423,-5.58049666379497,
134.891465125506));
#54518=CARTESIAN_POINT('Ctrl Pts',(-5.74766857261715,-5.43937761735855,
134.883581997011));
#54519=CARTESIAN_POINT('Ctrl Pts',(-5.87913196389727,-5.29336644783652,
134.875698868517));
#54520=CARTESIAN_POINT('Ctrl Pts',(-6.01060348369017,-5.14734625029805,
134.8678152526));
#54521=CARTESIAN_POINT('Ctrl Pts',(-6.13662407855223,-4.99643358295228,
134.859931636684));
#54522=CARTESIAN_POINT('Ctrl Pts',(-6.25682474599815,-4.84108098443573,
134.852048020767));
#54523=CARTESIAN_POINT('Ctrl Pts',(-6.37705305066459,-4.68569266636691,
134.844162592205));
#54524=CARTESIAN_POINT('Ctrl Pts',(-6.49145855034864,-4.52586265573655,
134.836277163643));
#54525=CARTESIAN_POINT('Ctrl Pts',(-6.59971423703762,-4.36207439063606,
134.82839173508));
#54526=CARTESIAN_POINT('Ctrl Pts',(-6.70801301192683,-4.19822093411906,
134.82050316794));
#54527=CARTESIAN_POINT('Ctrl Pts',(-6.81015690638498,-4.03040637137842,
134.8126146008));
#54528=CARTESIAN_POINT('Ctrl Pts',(-6.90586359404163,-3.85914096924308,
134.804726033659));
#54529=CARTESIAN_POINT('Ctrl Pts',(-7.00167213441906,-3.6876933034895,134.796829071369));
#54530=CARTESIAN_POINT('Ctrl Pts',(-7.09102961629076,-3.51278776416627,
134.788932109078));
#54531=CARTESIAN_POINT('Ctrl Pts',(-7.17370033858609,-3.33495793859081,
134.781035146788));
#54532=CARTESIAN_POINT('Ctrl Pts',(-7.25642147902373,-3.15701966047971,
134.773133368401));
#54533=CARTESIAN_POINT('Ctrl Pts',(-7.33244759646324,-2.97615385770899,
134.765231590014));
#54534=CARTESIAN_POINT('Ctrl Pts',(-7.40159197747227,-2.79291195690414,
134.757329811627));
#54535=CARTESIAN_POINT('Ctrl Pts',(-7.47082578604139,-2.60943306104842,
134.749417813512));
#54536=CARTESIAN_POINT('Ctrl Pts',(-7.53315997106042,-2.42357225487405,
134.741505815397));
#54537=CARTESIAN_POINT('Ctrl Pts',(-7.58845798383476,-2.23589499475592,
134.733593817282));
#54538=CARTESIAN_POINT('Ctrl Pts',(-7.61162728258782,-2.15726015254958,
134.730278771426));
#54539=CARTESIAN_POINT('Ctrl Pts',(-7.63356198405403,-2.07830654139874,
134.726963725571));
#54540=CARTESIAN_POINT('Ctrl Pts',(-7.65425473420167,-1.99907615261434,
134.723648679716));
#54541=CARTESIAN_POINT('Ctrl Pts',(-7.71759372002424,-1.7565577615776,134.713501568242));
#54542=CARTESIAN_POINT('Ctrl Pts',(-7.76943036390135,-1.51092178810988,
134.703354456769));
#54543=CARTESIAN_POINT('Ctrl Pts',(-7.80951006415253,-1.26312056348565,
134.693207345296));
#54544=CARTESIAN_POINT('Ctrl Pts',(-7.84891124105464,-1.01951445299105,
134.683232017844));
#54545=CARTESIAN_POINT('Ctrl Pts',(-7.87695022360203,-0.773815615821124,
134.673256690391));
#54546=CARTESIAN_POINT('Ctrl Pts',(-7.89343050424911,-0.526949593974311,
134.663281362939));
#54547=CARTESIAN_POINT('Ctrl Pts',(-7.90496760305664,-0.35412986187993,
134.656298087537));
#54548=CARTESIAN_POINT('Ctrl Pts',(-7.91084097439085,-0.180738545498725,
134.649314812135));
#54549=CARTESIAN_POINT('Ctrl Pts',(-7.91099681386514,-0.00710007152402601,
134.642331536734));
#54550=CARTESIAN_POINT('',(-7.89859990304224,0.000673465603601259,132.642392143699));
#54551=CARTESIAN_POINT('Ctrl Pts',(-7.90858822339541,-0.00709720147611503,
134.642331508237));
#54552=CARTESIAN_POINT('Ctrl Pts',(-7.89174604813805,1.95238971443055,134.56350285226));
#54553=CARTESIAN_POINT('Ctrl Pts',(-6.16908709444098,6.57245961758447,134.378739816482));
#54554=CARTESIAN_POINT('Ctrl Pts',(1.59515389369185,9.21941012471406,134.0880424009));
#54555=CARTESIAN_POINT('Ctrl Pts',(7.42670583543603,4.5815492960006,133.823206451394));
#54556=CARTESIAN_POINT('Ctrl Pts',(8.18443024418726,-0.799445619444897,
133.611337691789));
#54557=CARTESIAN_POINT('Ctrl Pts',(6.39974472309062,-5.93210089235586,133.399468932183));
#54558=CARTESIAN_POINT('Ctrl Pts',(-0.219058148002564,-9.35382555535514,
133.134632982678));
#54559=CARTESIAN_POINT('Ctrl Pts',(-6.81879397155213,-5.54610506984683,
132.864618323215));
#54560=CARTESIAN_POINT('Ctrl Pts',(-7.89554591951126,-1.44945742194562,
132.700538043555));
#54561=CARTESIAN_POINT('Ctrl Pts',(-7.89859990304224,0.000673465603601259,
132.642392143699));
#54562=CARTESIAN_POINT('',(-7.91099958186279,-0.00257211328256086,128.642116733665));
#54563=CARTESIAN_POINT('Ctrl Pts',(-7.9109999900693,0.000396388217883126,
132.635232504311));
#54564=CARTESIAN_POINT('Ctrl Pts',(-7.91094795170318,1.03896286230102,132.594969264453));
#54565=CARTESIAN_POINT('Ctrl Pts',(-7.70642795972031,2.06713172426845,132.562880167328));
#54566=CARTESIAN_POINT('Ctrl Pts',(-7.26277582939789,3.1385874062988,132.519128789588));
#54567=CARTESIAN_POINT('Ctrl Pts',(-7.21378524248674,3.24960670015131,132.514440493338));
#54568=CARTESIAN_POINT('Ctrl Pts',(-7.15375931622026,3.37758044291283,132.508807127237));
#54569=CARTESIAN_POINT('Ctrl Pts',(-7.1451868268163,3.39567772316477,132.508005074824));
#54570=CARTESIAN_POINT('Ctrl Pts',(-7.13393196830758,3.41920639359231,132.506955005739));
#54571=CARTESIAN_POINT('Ctrl Pts',(-7.13131187994195,3.42466765702155,132.506710759162));
#54572=CARTESIAN_POINT('Ctrl Pts',(-7.1270490433218,3.43352693002828,132.506313698973));
#54573=CARTESIAN_POINT('Ctrl Pts',(-7.1254101270074,3.43692679104352,132.506161120237));
#54574=CARTESIAN_POINT('Ctrl Pts',(-7.1222576605826,3.44345449956403,132.505867780234));
#54575=CARTESIAN_POINT('Ctrl Pts',(-7.12074448532198,3.44658251735062,132.505727042026));
#54576=CARTESIAN_POINT('Ctrl Pts',(-7.11726503482431,3.45376312358334,132.505403571937));
#54577=CARTESIAN_POINT('Ctrl Pts',(-7.115297359392,3.45781502933073,132.505220753944));
#54578=CARTESIAN_POINT('Ctrl Pts',(-7.11005202093613,3.46859297733137,132.504733699352));
#54579=CARTESIAN_POINT('Ctrl Pts',(-7.10676828187674,3.47531603883496,132.504429092044));
#54580=CARTESIAN_POINT('Ctrl Pts',(-7.0847362246594,3.52026222537289,132.50238742415));
#54581=CARTESIAN_POINT('Ctrl Pts',(-7.06568946305138,3.55833750450519,132.500632423061));
#54582=CARTESIAN_POINT('Ctrl Pts',(-6.69321051406074,4.28815531483912,132.466529263544));
#54583=CARTESIAN_POINT('Ctrl Pts',(-6.24011065199555,4.9242715280125,132.429196272166));
#54584=CARTESIAN_POINT('Ctrl Pts',(-5.47240228657801,5.72241320228477,132.379576049925));
#54585=CARTESIAN_POINT('Ctrl Pts',(-5.22851662524904,5.9460781776067,132.365197900984));
#54586=CARTESIAN_POINT('Ctrl Pts',(-4.91685151743975,6.1978542360538,132.348540362587));
#54587=CARTESIAN_POINT('Ctrl Pts',(-4.86178908113642,6.24114037931201,132.345656815579));
#54588=CARTESIAN_POINT('Ctrl Pts',(-4.78407932283109,6.30057764708837,132.341668796865));
#54589=CARTESIAN_POINT('Ctrl Pts',(-4.76191150434184,6.31734853394899,132.340540252326));
#54590=CARTESIAN_POINT('Ctrl Pts',(-4.72846890179672,6.34237321974727,132.338851261044));
#54591=CARTESIAN_POINT('Ctrl Pts',(-4.71726000541295,6.35071446828932,132.338287432713));
#54592=CARTESIAN_POINT('Ctrl Pts',(-4.69916748147276,6.36410393121257,132.337380979926));
#54593=CARTESIAN_POINT('Ctrl Pts',(-4.69229770223487,6.36917075767319,132.337037637922));
#54594=CARTESIAN_POINT('Ctrl Pts',(-4.67914146613145,6.37884134098802,132.336381710035));
#54595=CARTESIAN_POINT('Ctrl Pts',(-4.6728563845281,6.38344694687672,132.336069053155));
#54596=CARTESIAN_POINT('Ctrl Pts',(-4.66169209213125,6.39160263530104,132.335514908935));
#54597=CARTESIAN_POINT('Ctrl Pts',(-4.65681560966391,6.39515643180208,132.335273279085));
#54598=CARTESIAN_POINT('Ctrl Pts',(-4.64718383090292,6.40215885053305,132.334796843789));
#54599=CARTESIAN_POINT('Ctrl Pts',(-4.64242875028248,6.40560776229773,132.334562027312));
#54600=CARTESIAN_POINT('Ctrl Pts',(-4.62961550578364,6.41487958645215,132.333930336976));
#54601=CARTESIAN_POINT('Ctrl Pts',(-4.62155018750916,6.42069261881666,132.333533841232));
#54602=CARTESIAN_POINT('Ctrl Pts',(-4.59194489407692,6.44194578181686,132.332082525674));
#54603=CARTESIAN_POINT('Ctrl Pts',(-4.57033821705598,6.45729292855071,132.331031253419));
#54604=CARTESIAN_POINT('Ctrl Pts',(-4.22535730263465,6.69973270689204,132.31437085995));
#54605=CARTESIAN_POINT('Ctrl Pts',(-3.88548028124914,6.90240161556681,132.299733877187));
#54606=CARTESIAN_POINT('Ctrl Pts',(-3.34715800890321,7.17098716448073,132.278355786895));
#54607=CARTESIAN_POINT('Ctrl Pts',(-3.15892726184116,7.25587383091731,132.271183081488));
#54608=CARTESIAN_POINT('Ctrl Pts',(-2.61412396807595,7.47634098188474,132.25091564276));
#54609=CARTESIAN_POINT('Ctrl Pts',(-2.25079216990757,7.5936311732605,132.23799617387));
#54610=CARTESIAN_POINT('Ctrl Pts',(-1.72073573494283,7.72334257308298,132.218493191774));
#54611=CARTESIAN_POINT('Ctrl Pts',(-1.55986348048593,7.75743344346827,132.212486692338));
#54612=CARTESIAN_POINT('Ctrl Pts',(-1.28977901677055,7.80592673992084,132.202096264893));
#54613=CARTESIAN_POINT('Ctrl Pts',(-1.18111550855892,7.82310593368083,132.197834040615));
#54614=CARTESIAN_POINT('Ctrl Pts',(-1.05359868904454,7.84054849938519,132.192701881381));
#54615=CARTESIAN_POINT('Ctrl Pts',(-1.0350550412092,7.84301804279016,132.191952340923));
#54616=CARTESIAN_POINT('Ctrl Pts',(-1.01072785409723,7.84617002853083,132.190964618979));
#54617=CARTESIAN_POINT('Ctrl Pts',(-1.0049519447476,7.84691190851998,132.19072978234));
#54618=CARTESIAN_POINT('Ctrl Pts',(-0.995536243046376,7.84811073097967,
132.190346421189));
#54619=CARTESIAN_POINT('Ctrl Pts',(-0.991896934104965,7.84857152155503,
132.190198115428));
#54620=CARTESIAN_POINT('Ctrl Pts',(-0.984893002831329,7.84945337402424,
132.189912443526));
#54621=CARTESIAN_POINT('Ctrl Pts',(-0.981528426883154,7.84987480442578,
132.189775098502));
#54622=CARTESIAN_POINT('Ctrl Pts',(-0.973829634070222,7.85083409062804,
132.189460566666));
#54623=CARTESIAN_POINT('Ctrl Pts',(-0.969495243439694,7.85137052033414,
132.18928329783));
#54624=CARTESIAN_POINT('Ctrl Pts',(-0.957943699437552,7.85279044268084,
132.188810352685));
#54625=CARTESIAN_POINT('Ctrl Pts',(-0.950725783858959,7.85366757325387,
132.188514307789));
#54626=CARTESIAN_POINT('Ctrl Pts',(-0.90078313612652,7.85966681113154,132.186462296839));
#54627=CARTESIAN_POINT('Ctrl Pts',(-0.85801918780058,7.86445011294794,132.184687024655));
#54628=CARTESIAN_POINT('Ctrl Pts',(0.0186333393416185,7.95527161920517,
132.147953451114));
#54629=CARTESIAN_POINT('Ctrl Pts',(0.86092998641323,7.90858411738611,132.106983843917));
#54630=CARTESIAN_POINT('Ctrl Pts',(1.85443983819299,7.6926427696871,132.061545989791));
#54631=CARTESIAN_POINT('Ctrl Pts',(2.02731538522306,7.64890170177291,132.053719070985));
#54632=CARTESIAN_POINT('Ctrl Pts',(2.31672561877076,7.5651723044627,132.04078890563));
#54633=CARTESIAN_POINT('Ctrl Pts',(2.43406849349038,7.52823764126726,132.035594997805));
#54634=CARTESIAN_POINT('Ctrl Pts',(2.61187809791459,7.46767816836738,132.027801359881));
#54635=CARTESIAN_POINT('Ctrl Pts',(2.6729916807331,7.44602176805093,132.025136644212));
#54636=CARTESIAN_POINT('Ctrl Pts',(2.7582244420919,7.41463381056795,132.02143938825));
#54637=CARTESIAN_POINT('Ctrl Pts',(2.7825714613354,7.40553122319316,132.02038545397));
#54638=CARTESIAN_POINT('Ctrl Pts',(2.81917980552136,7.39163848444385,132.018804006081));
#54639=CARTESIAN_POINT('Ctrl Pts',(2.83147464019921,7.38693749971669,132.018273435129));
#54640=CARTESIAN_POINT('Ctrl Pts',(2.85131051991028,7.37929636407066,132.017418324722));
#54641=CARTESIAN_POINT('Ctrl Pts',(2.85885886034996,7.37637529731627,132.017093128996));
#54642=CARTESIAN_POINT('Ctrl Pts',(2.87330900930542,7.37075784719751,132.016470986355));
#54643=CARTESIAN_POINT('Ctrl Pts',(2.88021153591049,7.36806334213986,132.016173975111));
#54644=CARTESIAN_POINT('Ctrl Pts',(2.89250007835589,7.36324641786719,132.015645513019));
#54645=CARTESIAN_POINT('Ctrl Pts',(2.89788756427784,7.3611277789828,132.015413932));
#54646=CARTESIAN_POINT('Ctrl Pts',(2.90855290091077,7.35692009214983,132.014955689146));
#54647=CARTESIAN_POINT('Ctrl Pts',(2.91383083769874,7.35483127400743,132.014729019584));
#54648=CARTESIAN_POINT('Ctrl Pts',(2.92659786310087,7.34976264332575,132.014180960208));
#54649=CARTESIAN_POINT('Ctrl Pts',(2.93408466238265,7.34677705936597,132.013859770034));
#54650=CARTESIAN_POINT('Ctrl Pts',(2.96183600284105,7.33566120020737,132.012669952706));
#54651=CARTESIAN_POINT('Ctrl Pts',(2.98207151011635,7.32745844549907,132.01180383477));
#54652=CARTESIAN_POINT('Ctrl Pts',(3.32003177746828,7.18882951898955,131.997362332769));
#54653=CARTESIAN_POINT('Ctrl Pts',(3.62897825334765,7.03792785898434,131.984538251107));
#54654=CARTESIAN_POINT('Ctrl Pts',(4.09283314236616,6.77267007839567,131.965391487316));
#54655=CARTESIAN_POINT('Ctrl Pts',(4.2550238055422,6.67196512140592,131.958713375773));
#54656=CARTESIAN_POINT('Ctrl Pts',(4.66916527709572,6.3935732931529,131.941463400556));
#54657=CARTESIAN_POINT('Ctrl Pts',(4.91464688839365,6.20686131123768,131.931043404374));
#54658=CARTESIAN_POINT('Ctrl Pts',(5.33638453856187,5.84534760120043,131.911836957138));
#54659=CARTESIAN_POINT('Ctrl Pts',(5.5164997941389,5.67567683911407,131.903140796033));
#54660=CARTESIAN_POINT('Ctrl Pts',(5.79912937379087,5.38325391866127,131.888111139432));
#54661=CARTESIAN_POINT('Ctrl Pts',(5.90640090886794,5.26533446712871,131.882039253812));
#54662=CARTESIAN_POINT('Ctrl Pts',(6.02509285689291,5.12666690078153,131.874778676996));
#54663=CARTESIAN_POINT('Ctrl Pts',(6.0400763906773,5.10900524752315,131.873851754122));
#54664=CARTESIAN_POINT('Ctrl Pts',(6.05894947626649,5.08655976557817,131.872670662167));
#54665=CARTESIAN_POINT('Ctrl Pts',(6.06291142525821,5.08183668114252,131.872421958219));
#54666=CARTESIAN_POINT('Ctrl Pts',(6.06922349211669,5.07429410611729,131.872024503519));
#54667=CARTESIAN_POINT('Ctrl Pts',(6.07157718244386,5.07147759436793,131.871876024749));
#54668=CARTESIAN_POINT('Ctrl Pts',(6.07601603174254,5.06615838613592,131.871595489335));
#54669=CARTESIAN_POINT('Ctrl Pts',(6.07810160936931,5.0636560346834,131.87146346451));
#54670=CARTESIAN_POINT('Ctrl Pts',(6.08282208055239,5.0579851244103,131.871164149244));
#54671=CARTESIAN_POINT('Ctrl Pts',(6.08545603929925,5.05481580040668,131.870996787837));
#54672=CARTESIAN_POINT('Ctrl Pts',(6.09323888713325,5.04543614999178,131.870501241705));
#54673=CARTESIAN_POINT('Ctrl Pts',(6.09838074083817,5.03922002081146,131.870172522504));
#54674=CARTESIAN_POINT('Ctrl Pts',(6.13259273654294,4.99773114220861,131.867976535246));
#54675=CARTESIAN_POINT('Ctrl Pts',(6.16136566898044,4.96221555058488,131.866087157071));
#54676=CARTESIAN_POINT('Ctrl Pts',(6.66638880892651,4.32768062494586,131.832194411121));
#54677=CARTESIAN_POINT('Ctrl Pts',(7.0535396805134,3.66294428229163,131.794938896219));
#54678=CARTESIAN_POINT('Ctrl Pts',(7.4576447239246,2.65859771345574,131.745354575948));
#54679=CARTESIAN_POINT('Ctrl Pts',(7.55827724914286,2.35734591467176,131.731183309549));
#54680=CARTESIAN_POINT('Ctrl Pts',(7.67660025608047,1.91652548443221,131.711633354972));
#54681=CARTESIAN_POINT('Ctrl Pts',(7.70910570283183,1.7812785755044,131.705788320328));
#54682=CARTESIAN_POINT('Ctrl Pts',(7.7478294659085,1.59914974625125,131.698119186125));
#54683=CARTESIAN_POINT('Ctrl Pts',(7.75721717900618,1.55297233888448,131.696191887625));
#54684=CARTESIAN_POINT('Ctrl Pts',(7.770101227033,1.48656289536027,131.693444391243));
#54685=CARTESIAN_POINT('Ctrl Pts',(7.77393216493602,1.46639729394148,131.692613293131));
#54686=CARTESIAN_POINT('Ctrl Pts',(7.77971464450336,1.43529939845721,131.691336513389));
#54687=CARTESIAN_POINT('Ctrl Pts',(7.78172171020141,1.42437759721175,131.690889025046));
#54688=CARTESIAN_POINT('Ctrl Pts',(7.78541675798574,1.40402941884346,131.690057033618));
#54689=CARTESIAN_POINT('Ctrl Pts',(7.78711063207951,1.39460414064827,131.68967233954));
#54690=CARTESIAN_POINT('Ctrl Pts',(7.78988219011802,1.37901978197349,131.689037387381));
#54691=CARTESIAN_POINT('Ctrl Pts',(7.7909696913176,1.37286247097084,131.688786810826));
#54692=CARTESIAN_POINT('Ctrl Pts',(7.7930877055696,1.36078694157827,131.688295954902));
#54693=CARTESIAN_POINT('Ctrl Pts',(7.79411877955699,1.35486882665335,131.688055657487));
#54694=CARTESIAN_POINT('Ctrl Pts',(7.79648925002074,1.34117064444636,131.687500076104));
#54695=CARTESIAN_POINT('Ctrl Pts',(7.79782374473194,1.33338972914269,131.687184951107));
#54696=CARTESIAN_POINT('Ctrl Pts',(7.80138162582009,1.31245709975048,131.6863384149));
#54697=CARTESIAN_POINT('Ctrl Pts',(7.80358340596412,1.29930171200063,131.685807702898));
#54698=CARTESIAN_POINT('Ctrl Pts',(7.81900233569048,1.20572226688222,131.682041741535));
#54699=CARTESIAN_POINT('Ctrl Pts',(7.83100943927282,1.125102384467,131.678845690526));
#54700=CARTESIAN_POINT('Ctrl Pts',(7.91896026888329,0.464675656566267,131.653035159888));
#54701=CARTESIAN_POINT('Ctrl Pts',(7.9316514265255,-0.121759544513063,131.632629427665));
#54702=CARTESIAN_POINT('Ctrl Pts',(7.84316226858836,-1.11183984236711,131.598400623501));
#54703=CARTESIAN_POINT('Ctrl Pts',(7.77516385517507,-1.51597293921305,131.584434331657));
#54704=CARTESIAN_POINT('Ctrl Pts',(7.63598187411996,-2.07446096873227,131.563252345613));
#54705=CARTESIAN_POINT('Ctrl Pts',(7.59066262230468,-2.23460197419843,131.55694914809));
#54706=CARTESIAN_POINT('Ctrl Pts',(7.52914742851288,-2.42842050066906,131.548915818308));
#54707=CARTESIAN_POINT('Ctrl Pts',(7.51771953247,-2.46357059711809,131.547442850672));
#54708=CARTESIAN_POINT('Ctrl Pts',(7.50329665156053,-2.50689770949118,131.545608370049));
#54709=CARTESIAN_POINT('Ctrl Pts',(7.50053379095651,-2.5151520067348,131.545258032619));
#54710=CARTESIAN_POINT('Ctrl Pts',(7.49616650419597,-2.52812848061597,131.5447059537));
#54711=CARTESIAN_POINT('Ctrl Pts',(7.49457122037041,-2.53285374543423,131.544504643964));
#54712=CARTESIAN_POINT('Ctrl Pts',(7.49172801176544,-2.54124918598517,131.544146488653));
#54713=CARTESIAN_POINT('Ctrl Pts',(7.4904818545929,-2.54491996209606,131.543989725659));
#54714=CARTESIAN_POINT('Ctrl Pts',(7.48759928362759,-2.55339062515391,131.54362760119));
#54715=CARTESIAN_POINT('Ctrl Pts',(7.48596095272213,-2.55818985435979,131.543422150995));
#54716=CARTESIAN_POINT('Ctrl Pts',(7.48145326778402,-2.57135298824682,131.542857884869));
#54717=CARTESIAN_POINT('Ctrl Pts',(7.47857450918445,-2.57971364648603,131.542498638606));
#54718=CARTESIAN_POINT('Ctrl Pts',(7.46438476031598,-2.62070097284575,131.540733359138));
#54719=CARTESIAN_POINT('Ctrl Pts',(7.45287435907547,-2.65325784178718,131.539318388305));
#54720=CARTESIAN_POINT('Ctrl Pts',(7.29297855637333,-3.09626787658655,131.519898925119));
#54721=CARTESIAN_POINT('Ctrl Pts',(7.11109337842901,-3.49381222573771,131.500570918388));
#54722=CARTESIAN_POINT('Ctrl Pts',(6.70528432356826,-4.21626843459996,131.463806649159));
#54723=CARTESIAN_POINT('Ctrl Pts',(6.4880263442299,-4.54348941593306,131.446426747615));
#54724=CARTESIAN_POINT('Ctrl Pts',(6.06606946027511,-5.08665661225072,131.416878620206));
#54725=CARTESIAN_POINT('Ctrl Pts',(5.8718072473367,-5.30972415006333,131.40449583932));
#54726=CARTESIAN_POINT('Ctrl Pts',(5.62930591405306,-5.55855433409347,131.390351730688));
#54727=CARTESIAN_POINT('Ctrl Pts',(5.59273992746962,-5.59534373847565,131.388251003892));
#54728=CARTESIAN_POINT('Ctrl Pts',(5.54429746231643,-5.64313285138328,131.385508756135));
#54729=CARTESIAN_POINT('Ctrl Pts',(5.5327456039383,-5.65445919728429,131.384857818466));
#54730=CARTESIAN_POINT('Ctrl Pts',(5.51384237877515,-5.67288000859969,131.383797472318));
#54731=CARTESIAN_POINT('Ctrl Pts',(5.50651188801334,-5.67999579205593,131.383387458373));
#54732=CARTESIAN_POINT('Ctrl Pts',(5.4925265928464,-5.69351894409775,131.382607452013));
#54733=CARTESIAN_POINT('Ctrl Pts',(5.48587430704625,-5.6999288967277,131.382237386594));
#54734=CARTESIAN_POINT('Ctrl Pts',(5.47167526625449,-5.71356280433379,131.381449524467));
#54735=CARTESIAN_POINT('Ctrl Pts',(5.46412539406275,-5.72078349678331,131.381031819927));
#54736=CARTESIAN_POINT('Ctrl Pts',(5.44114928664589,-5.74267085236367,131.379764322483));
#54737=CARTESIAN_POINT('Ctrl Pts',(5.4256781032117,-5.75729026577929,131.378915860604));
#54738=CARTESIAN_POINT('Ctrl Pts',(5.37373696486679,-5.80597645639405,131.376084006294));
#54739=CARTESIAN_POINT('Ctrl Pts',(5.33700347100113,-5.83976074913527,131.374108585878));
#54740=CARTESIAN_POINT('Ctrl Pts',(5.09255342306083,-6.06035167687583,131.361139427583));
#54741=CARTESIAN_POINT('Ctrl Pts',(4.87538086881165,-6.23639607301965,131.350459051153));
#54742=CARTESIAN_POINT('Ctrl Pts',(4.49149460519032,-6.51524821110713,131.332735679711));
#54743=CARTESIAN_POINT('Ctrl Pts',(4.32945852145937,-6.62403007630357,131.325570973267));
#54744=CARTESIAN_POINT('Ctrl Pts',(3.60891623936488,-7.0700167587946,131.294717704627));
#54745=CARTESIAN_POINT('Ctrl Pts',(3.01400059395305,-7.34336654465063,131.271963906837));
#54746=CARTESIAN_POINT('Ctrl Pts',(2.3670767210127,-7.54861400357023,131.244958244254));
#54747=CARTESIAN_POINT('Ctrl Pts',(2.34173565613689,-7.556513724665,131.243896633074));
#54748=CARTESIAN_POINT('Ctrl Pts',(2.30893497647872,-7.56655803536547,131.24251717119));
#54749=CARTESIAN_POINT('Ctrl Pts',(2.301511101712,-7.56881945063003,131.242204600444));
#54750=CARTESIAN_POINT('Ctrl Pts',(2.28951274441062,-7.5724550317202,131.241698842399));
#54751=CARTESIAN_POINT('Ctrl Pts',(2.28494031214915,-7.57383598871878,131.241505966682));
#54752=CARTESIAN_POINT('Ctrl Pts',(2.27621020899762,-7.57646401205051,131.241137444508));
#54753=CARTESIAN_POINT('Ctrl Pts',(2.27205275564896,-7.57771179953933,131.240961831523));
#54754=CARTESIAN_POINT('Ctrl Pts',(2.26263461859717,-7.5805300424112,131.240563739826));
#54755=CARTESIAN_POINT('Ctrl Pts',(2.2573733266131,-7.58209844338886,131.240341165324));
#54756=CARTESIAN_POINT('Ctrl Pts',(2.2436528585288,-7.58617299361049,131.239760236373));
#54757=CARTESIAN_POINT('Ctrl Pts',(2.23519113137637,-7.58867046615007,131.239401472826));
#54758=CARTESIAN_POINT('Ctrl Pts',(2.18420495671738,-7.60362632226738,131.23723669737));
#54759=CARTESIAN_POINT('Ctrl Pts',(2.14158123999707,-7.61574121246456,131.235414232346));
#54760=CARTESIAN_POINT('Ctrl Pts',(1.37911887385481,-7.82554800652509,131.202554128601));
#54761=CARTESIAN_POINT('Ctrl Pts',(0.634987577964584,-7.92073081713082,
131.166722058371));
#54762=CARTESIAN_POINT('Ctrl Pts',(-0.397712696560308,-7.90618200270992,
131.119963531086));
#54763=CARTESIAN_POINT('Ctrl Pts',(-0.683569875026899,-7.88661151090959,
131.107286691559));
#54764=CARTESIAN_POINT('Ctrl Pts',(-1.10081546267506,-7.83518350010563,
131.089340236663));
#54765=CARTESIAN_POINT('Ctrl Pts',(-1.233441738958,-7.8154026753967,131.083717454687));
#54766=CARTESIAN_POINT('Ctrl Pts',(-1.43349669254303,-7.78034529779056,
131.075361766605));
#54767=CARTESIAN_POINT('Ctrl Pts',(-1.5013298142648,-7.76754110587916,131.072550574063));
#54768=CARTESIAN_POINT('Ctrl Pts',(-1.58185370165547,-7.75124713669702,
131.069239008941));
#54769=CARTESIAN_POINT('Ctrl Pts',(-1.59471308578156,-7.74861171332221,
131.068710940988));
#54770=CARTESIAN_POINT('Ctrl Pts',(-1.614516634146,-7.7445017549083,131.067898901919));
#54771=CARTESIAN_POINT('Ctrl Pts',(-1.62146544308083,-7.74304986494043,
131.067614193809));
#54772=CARTESIAN_POINT('Ctrl Pts',(-1.63413641041717,-7.74038457748103,
131.067095446513));
#54773=CARTESIAN_POINT('Ctrl Pts',(-1.63985919138712,-7.73917418383735,
131.066861309592));
#54774=CARTESIAN_POINT('Ctrl Pts',(-1.6523363781673,-7.73652074240015,131.066351160731));
#54775=CARTESIAN_POINT('Ctrl Pts',(-1.6590902503675,-7.7350751932775,131.066075230638));
#54776=CARTESIAN_POINT('Ctrl Pts',(-1.67749774714395,-7.73111017012517,
131.0653237668));
#54777=CARTESIAN_POINT('Ctrl Pts',(-1.68914760465236,-7.72857318821637,
131.06484880544));
#54778=CARTESIAN_POINT('Ctrl Pts',(-1.74492752582118,-7.71629388370907,
131.062577667096));
#54779=CARTESIAN_POINT('Ctrl Pts',(-1.78897972468597,-7.7061997769764,131.060793023287));
#54780=CARTESIAN_POINT('Ctrl Pts',(-1.84706304523951,-7.69236568150757,
131.058451378223));
#54781=CARTESIAN_POINT('Ctrl Pts',(-1.86117336115243,-7.68896386997159,
131.057883410271));
#54782=CARTESIAN_POINT('Ctrl Pts',(-2.71240001714543,-7.48126383329723,
131.023673000603));
#54783=CARTESIAN_POINT('Ctrl Pts',(-3.51042653431377,-7.14165685064727,
130.995560409281));
#54784=CARTESIAN_POINT('Ctrl Pts',(-4.40954899709344,-6.57123057393559,
130.958885717486));
#54785=CARTESIAN_POINT('Ctrl Pts',(-4.57683320094183,-6.4558334586399,130.951772417187));
#54786=CARTESIAN_POINT('Ctrl Pts',(-4.89572206163713,-6.21722635110868,
130.937284777857));
#54787=CARTESIAN_POINT('Ctrl Pts',(-5.04757169919715,-6.09458844169352,
130.92993623124));
#54788=CARTESIAN_POINT('Ctrl Pts',(-5.21396155370323,-5.94972071977245,
130.921173455877));
#54789=CARTESIAN_POINT('Ctrl Pts',(-5.23311934502349,-5.93287734738094,
130.920153436527));
#54790=CARTESIAN_POINT('Ctrl Pts',(-5.25694017960767,-5.9117291218545,130.918870767154));
#54791=CARTESIAN_POINT('Ctrl Pts',(-5.26168014864321,-5.90751075116037,
130.918614820894));
#54792=CARTESIAN_POINT('Ctrl Pts',(-5.26917320794426,-5.90082607495836,
130.918209072388));
#54793=CARTESIAN_POINT('Ctrl Pts',(-5.27192966505674,-5.89836352464966,
130.918059565217));
#54794=CARTESIAN_POINT('Ctrl Pts',(-5.27711113120327,-5.89372799774494,
130.917778064739));
#54795=CARTESIAN_POINT('Ctrl Pts',(-5.27953652128446,-5.89155545869114,
130.91764610613));
#54796=CARTESIAN_POINT('Ctrl Pts',(-5.28499159555949,-5.88666301156981,
130.917348882059));
#54797=CARTESIAN_POINT('Ctrl Pts',(-5.28802052075513,-5.88394226253862,
130.917183550488));
#54798=CARTESIAN_POINT('Ctrl Pts',(-5.29572919494782,-5.87700714265529,
130.916762021924));
#54799=CARTESIAN_POINT('Ctrl Pts',(-5.30040600605356,-5.87278952726674,
130.916505571665));
#54800=CARTESIAN_POINT('Ctrl Pts',(-5.32636533793939,-5.84932276106918,
130.915078178322));
#54801=CARTESIAN_POINT('Ctrl Pts',(-5.34754778819162,-5.82996372960949,
130.91389875151));
#54802=CARTESIAN_POINT('Ctrl Pts',(-5.6946911491533,-5.50921931710964,130.894334496078));
#54803=CARTESIAN_POINT('Ctrl Pts',(-5.99479350416303,-5.18106042245828,
130.8740210156));
#54804=CARTESIAN_POINT('Ctrl Pts',(-6.5200741493786,-4.49956539958774,130.834228668107));
#54805=CARTESIAN_POINT('Ctrl Pts',(-6.74794193065218,-4.15003275107279,
130.814844099563));
#54806=CARTESIAN_POINT('Ctrl Pts',(-7.03508379043539,-3.62287872985283,
130.788037293962));
#54807=CARTESIAN_POINT('Ctrl Pts',(-7.11729875571675,-3.45857170326395,
130.779987059471));
#54808=CARTESIAN_POINT('Ctrl Pts',(-7.25185074359103,-3.16450617368557,
130.766146800626));
#54809=CARTESIAN_POINT('Ctrl Pts',(-7.30660454619088,-3.03594651390896,
130.760279047811));
#54810=CARTESIAN_POINT('Ctrl Pts',(-7.38440199271126,-2.83896508320385,
130.751563044479));
#54811=CARTESIAN_POINT('Ctrl Pts',(-7.40996021439371,-2.77157094916318,
130.748628567891));
#54812=CARTESIAN_POINT('Ctrl Pts',(-7.43910990870253,-2.69141957275958,
130.745193644116));
#54813=CARTESIAN_POINT('Ctrl Pts',(-7.4435943489459,-2.67899210917003,130.744662612598));
#54814=CARTESIAN_POINT('Ctrl Pts',(-7.4504348339017,-2.65988570112069,130.74384855905));
#54815=CARTESIAN_POINT('Ctrl Pts',(-7.45281306624921,-2.6532147589541,130.743564778228));
#54816=CARTESIAN_POINT('Ctrl Pts',(-7.45695171924324,-2.64155636517062,
130.74306960412));
#54817=CARTESIAN_POINT('Ctrl Pts',(-7.45871610049223,-2.63657033016418,
130.742858075597));
#54818=CARTESIAN_POINT('Ctrl Pts',(-7.4624012307939,-2.62612307113866,130.742415373882));
#54819=CARTESIAN_POINT('Ctrl Pts',(-7.46432098856182,-2.62066149932168,
130.742184234618));
#54820=CARTESIAN_POINT('Ctrl Pts',(-7.46963049808029,-2.60550316436887,
130.741543532976));
#54821=CARTESIAN_POINT('Ctrl Pts',(-7.47300736680033,-2.59580188269205,
130.741134410099));
#54822=CARTESIAN_POINT('Ctrl Pts',(-7.48628578863159,-2.5574141320149,130.739519155188));
#54823=CARTESIAN_POINT('Ctrl Pts',(-7.49604119900371,-2.52867718805475,
130.738317999717));
#54824=CARTESIAN_POINT('Ctrl Pts',(-7.64727756504756,-2.07460648163473,
130.719462981015));
#54825=CARTESIAN_POINT('Ctrl Pts',(-7.75253102546044,-1.63803713484436,
130.703121639252));
#54826=CARTESIAN_POINT('Ctrl Pts',(-7.88062165178306,-0.799703456417926,
130.673462881414));
#54827=CARTESIAN_POINT('Ctrl Pts',(-7.91095997801479,-0.400537241286116,
130.660034885164));
#54828=CARTESIAN_POINT('Ctrl Pts',(-7.91103291491228,0.328689150824926,
130.634747395728));
#54829=CARTESIAN_POINT('Ctrl Pts',(-7.89048220500111,0.657826822631501,
130.623038747333));
#54830=CARTESIAN_POINT('Ctrl Pts',(-7.83991796357951,1.06089848483932,130.6073645755));
#54831=CARTESIAN_POINT('Ctrl Pts',(-7.82924963479842,1.13695589894975,130.604347262515));
#54832=CARTESIAN_POINT('Ctrl Pts',(-7.81600004916629,1.22235711517645,130.600880103638));
#54833=CARTESIAN_POINT('Ctrl Pts',(-7.81450671352799,1.23186789399559,130.600492872467));
#54834=CARTESIAN_POINT('Ctrl Pts',(-7.81230726535053,1.24571082433252,130.599927613742));
#54835=CARTESIAN_POINT('Ctrl Pts',(-7.81161489773633,1.2500451813399,130.599750390828));
#54836=CARTESIAN_POINT('Ctrl Pts',(-7.81038073212566,1.25773023339407,130.599435751197));
#54837=CARTESIAN_POINT('Ctrl Pts',(-7.8098403834645,1.26108116530687,130.599298418585));
#54838=CARTESIAN_POINT('Ctrl Pts',(-7.80871313508163,1.26804320058586,130.599012802242));
#54839=CARTESIAN_POINT('Ctrl Pts',(-7.80812588674762,1.27165424591941,130.598864498432));
#54840=CARTESIAN_POINT('Ctrl Pts',(-7.80660454369678,1.28096834298144,130.598481559491));
#54841=CARTESIAN_POINT('Ctrl Pts',(-7.80566670570576,1.28667077237749,130.59824671014));
#54842=CARTESIAN_POINT('Ctrl Pts',(-7.80172808803881,1.31045635015706,130.597265468251));
#54843=CARTESIAN_POINT('Ctrl Pts',(-7.79867073197085,1.32852994290822,130.596515875738));
#54844=CARTESIAN_POINT('Ctrl Pts',(-7.77742721374019,1.45151065805286,130.591388921731));
#54845=CARTESIAN_POINT('Ctrl Pts',(-7.75718827594154,1.55604803244397,130.586900046625));
#54846=CARTESIAN_POINT('Ctrl Pts',(-7.70222767587984,1.81211778496722,130.575636306599));
#54847=CARTESIAN_POINT('Ctrl Pts',(-7.66513785409964,1.96309440088421,130.568762424454));
#54848=CARTESIAN_POINT('Ctrl Pts',(-7.48713718941258,2.6053527430499,130.538793985833));
#54849=CARTESIAN_POINT('Ctrl Pts',(-7.3032496197308,3.08344847744397,130.51472866198));
#54850=CARTESIAN_POINT('Ctrl Pts',(-6.86133372848045,3.96647821342088,130.469937158483));
#54851=CARTESIAN_POINT('Ctrl Pts',(-6.61007948701673,4.37239069874427,130.449186903871));
#54852=CARTESIAN_POINT('Ctrl Pts',(-6.30555883645787,4.77752756079774,130.428587305544));
#54853=CARTESIAN_POINT('Ctrl Pts',(-6.28718655365735,4.80167961241627,130.427359353216));
#54854=CARTESIAN_POINT('Ctrl Pts',(-6.26117714035271,4.83546615375253,130.425641564277));
#54855=CARTESIAN_POINT('Ctrl Pts',(-6.25365594172405,4.84518931222048,130.425147215988));
#54856=CARTESIAN_POINT('Ctrl Pts',(-6.24174007671733,4.86051978374536,130.424367769685));
#54857=CARTESIAN_POINT('Ctrl Pts',(-6.23736046119012,4.866138739391,130.424082083511));
#54858=CARTESIAN_POINT('Ctrl Pts',(-6.22925650876816,4.87650702598924,130.423554919828));
#54859=CARTESIAN_POINT('Ctrl Pts',(-6.22553431762297,4.881258022975,130.423313358516));
#54860=CARTESIAN_POINT('Ctrl Pts',(-6.21728122239431,4.89176746076434,130.422779006194));
#54861=CARTESIAN_POINT('Ctrl Pts',(-6.2127477451879,4.89752387881474,130.42248631656));
#54862=CARTESIAN_POINT('Ctrl Pts',(-6.1998036349346,4.91391286838042,130.421652988074));
#54863=CARTESIAN_POINT('Ctrl Pts',(-6.19137364097122,4.92453015322171,130.421113111792));
#54864=CARTESIAN_POINT('Ctrl Pts',(-6.13831449288885,4.99100470561949,130.417732766416));
#54865=CARTESIAN_POINT('Ctrl Pts',(-6.09295647148239,5.04627729650937,130.41492124437));
#54866=CARTESIAN_POINT('Ctrl Pts',(-5.95725269975102,5.20714624530884,130.406730687115));
#54867=CARTESIAN_POINT('Ctrl Pts',(-5.86486542671557,5.31098742954592,130.401434120583));
#54868=CARTESIAN_POINT('Ctrl Pts',(-5.50603241222408,5.69351859760438,130.381813610588));
#54869=CARTESIAN_POINT('Ctrl Pts',(-5.22206775622077,5.95504643575549,130.368202391086));
#54870=CARTESIAN_POINT('Ctrl Pts',(-4.80019551598562,6.29011228114838,130.349482684246));
#54871=CARTESIAN_POINT('Ctrl Pts',(-4.67749188618746,6.38188523948141,130.344192836534));
#54872=CARTESIAN_POINT('Ctrl Pts',(-4.41120547188366,6.56923954120295,130.332904058251));
#54873=CARTESIAN_POINT('Ctrl Pts',(-4.26700664810291,6.66380479476013,130.326902525107));
#54874=CARTESIAN_POINT('Ctrl Pts',(-4.10284402528909,6.76394767028824,130.320080444955));
#54875=CARTESIAN_POINT('Ctrl Pts',(-4.08581278607769,6.77424911373059,130.319372789222));
#54876=CARTESIAN_POINT('Ctrl Pts',(-3.81139426529799,6.93882140184577,130.307969700936));
#54877=CARTESIAN_POINT('Ctrl Pts',(-3.5454922719141,7.07837721351181,130.296912953092));
#54878=CARTESIAN_POINT('Ctrl Pts',(-3.25463932061844,7.21052158760868,130.284179645582));
#54879=CARTESIAN_POINT('Ctrl Pts',(-3.23691660724795,7.21849496352832,130.283401292647));
#54880=CARTESIAN_POINT('Ctrl Pts',(-3.21347062439935,7.22893950760221,130.28236811055));
#54881=CARTESIAN_POINT('Ctrl Pts',(-3.2077734325387,7.23146938481679,130.282116785247));
#54882=CARTESIAN_POINT('Ctrl Pts',(-3.19893421058472,7.23538200102203,130.281726425675));
#54883=CARTESIAN_POINT('Ctrl Pts',(-3.1957942504147,7.23676943762263,130.281587674613));
#54884=CARTESIAN_POINT('Ctrl Pts',(-3.18953558221783,7.23953005254834,130.281310943462));
#54885=CARTESIAN_POINT('Ctrl Pts',(-3.18641689944599,7.2409032554512,130.281172965483));
#54886=CARTESIAN_POINT('Ctrl Pts',(-3.17938646988891,7.24399343765884,130.280861735138));
#54887=CARTESIAN_POINT('Ctrl Pts',(-3.17547422640833,7.24570926045485,130.280688413514));
#54888=CARTESIAN_POINT('Ctrl Pts',(-3.16392437808449,7.25076361555622,130.280176347699));
#54889=CARTESIAN_POINT('Ctrl Pts',(-3.15628290402593,7.25409323814436,130.279837070396));
#54890=CARTESIAN_POINT('Ctrl Pts',(-3.0973794629864,7.27964856541783,130.277218099187));
#54891=CARTESIAN_POINT('Ctrl Pts',(-3.04588968978225,7.30134223921569,130.274907249107));
#54892=CARTESIAN_POINT('Ctrl Pts',(-2.87136915736464,7.37270392794885,130.267013586535));
#54893=CARTESIAN_POINT('Ctrl Pts',(-2.74732391538786,7.41982023551406,130.261301297803));
#54894=CARTESIAN_POINT('Ctrl Pts',(-2.27203882899092,7.58679602875068,130.239191723613));
#54895=CARTESIAN_POINT('Ctrl Pts',(-1.9137103059457,7.68500675676215,130.222089342572));
#54896=CARTESIAN_POINT('Ctrl Pts',(-0.906523780322296,7.88622173017763,
130.174927234953));
#54897=CARTESIAN_POINT('Ctrl Pts',(-0.249631199968885,7.93424366056588,
130.145415133292));
#54898=CARTESIAN_POINT('Ctrl Pts',(0.450221938594702,7.89830405165142,130.116818826349));
#54899=CARTESIAN_POINT('Ctrl Pts',(0.49470468697603,7.89564272514561,130.115012083063));
#54900=CARTESIAN_POINT('Ctrl Pts',(0.55122710415142,7.89178154158142,130.112729866365));
#54901=CARTESIAN_POINT('Ctrl Pts',(0.563289279236045,7.89092975573633,130.112243613629));
#54902=CARTESIAN_POINT('Ctrl Pts',(0.582408222969144,7.88953558534941,130.111474122293));
#54903=CARTESIAN_POINT('Ctrl Pts',(0.58946627508628,7.88901138302808,130.111190319687));
#54904=CARTESIAN_POINT('Ctrl Pts',(0.602602291767799,7.88801804253934,130.110662618495));
#54905=CARTESIAN_POINT('Ctrl Pts',(0.608680432799848,7.8875513495894,130.110418644177));
#54906=CARTESIAN_POINT('Ctrl Pts',(0.622142988460595,7.8865020110791,130.109878697659));
#54907=CARTESIAN_POINT('Ctrl Pts',(0.629527140494808,7.88591601835874,130.109582829671));
#54908=CARTESIAN_POINT('Ctrl Pts',(0.650795692714577,7.88419812178436,130.108731474332));
#54909=CARTESIAN_POINT('Ctrl Pts',(0.664677971958839,7.88303991194524,130.108176805025));
#54910=CARTESIAN_POINT('Ctrl Pts',(0.756990123922037,7.87509265190044,130.104495190106));
#54911=CARTESIAN_POINT('Ctrl Pts',(0.835319224920858,7.86716979354909,130.101403665925));
#54912=CARTESIAN_POINT('Ctrl Pts',(1.05408590595373,7.84173769891461,130.092853915453));
#54913=CARTESIAN_POINT('Ctrl Pts',(1.19419307205132,7.82162722728017,130.087476680529));
#54914=CARTESIAN_POINT('Ctrl Pts',(1.49027988480946,7.77098607757518,130.076281392198));
#54915=CARTESIAN_POINT('Ctrl Pts',(1.64603128935182,7.73949238604636,130.070492881113));
#54916=CARTESIAN_POINT('Ctrl Pts',(2.06726376488785,7.64102493061572,130.055004966588));
#54917=CARTESIAN_POINT('Ctrl Pts',(2.33038643058641,7.56492872936868,130.045519425484));
#54918=CARTESIAN_POINT('Ctrl Pts',(2.8478452158403,7.38571008781671,130.026672806573));
#54919=CARTESIAN_POINT('Ctrl Pts',(3.1018167686513,7.28269619177499,130.017323336003));
#54920=CARTESIAN_POINT('Ctrl Pts',(3.66125196792386,7.02120026050839,129.995643578202));
#54921=CARTESIAN_POINT('Ctrl Pts',(3.96273547279232,6.85556009797179,129.98318309493));
#54922=CARTESIAN_POINT('Ctrl Pts',(4.27192873229387,6.65845917864147,129.968605280587));
#54923=CARTESIAN_POINT('Ctrl Pts',(4.29133686943987,6.64596731711211,129.96768228304));
#54924=CARTESIAN_POINT('Ctrl Pts',(4.31614169682477,6.62984797163986,129.966492066511));
#54925=CARTESIAN_POINT('Ctrl Pts',(4.32158913210057,6.62629841215792,129.966230024657));
#54926=CARTESIAN_POINT('Ctrl Pts',(4.32993920728474,6.62084281036624,129.965827338139));
#54927=CARTESIAN_POINT('Ctrl Pts',(4.33284498851648,6.61894155917422,129.965687016161));
#54928=CARTESIAN_POINT('Ctrl Pts',(4.33827209714199,6.61538549947473,129.965424582212));
#54929=CARTESIAN_POINT('Ctrl Pts',(4.34079373370236,6.61373116001208,129.965302502059));
#54930=CARTESIAN_POINT('Ctrl Pts',(4.3464254523047,6.61003181854868,129.965029531019));
#54931=CARTESIAN_POINT('Ctrl Pts',(4.34953503656226,6.60798606386961,129.964878588751));
#54932=CARTESIAN_POINT('Ctrl Pts',(4.35791601134747,6.60246385158004,129.964471171882));
#54933=CARTESIAN_POINT('Ctrl Pts',(4.36318464149177,6.5989833047822,129.964214414518));
#54934=CARTESIAN_POINT('Ctrl Pts',(4.37481178386018,6.59128220451629,129.963646381333));
#54935=CARTESIAN_POINT('Ctrl Pts',(4.38116835252576,6.58705876016172,129.963334908169));
#54936=CARTESIAN_POINT('Ctrl Pts',(4.40028359449438,6.57431826218581,129.962395484877));
#54937=CARTESIAN_POINT('Ctrl Pts',(4.41302355311181,6.56577333129612,129.961765651342));
#54938=CARTESIAN_POINT('Ctrl Pts',(4.5586595980414,6.46747712409643,129.954523808993));
#54939=CARTESIAN_POINT('Ctrl Pts',(4.68881475888441,6.37374677186225,129.947651275249));
#54940=CARTESIAN_POINT('Ctrl Pts',(5.1233848425342,6.04027707809516,129.923574407558));
#54941=CARTESIAN_POINT('Ctrl Pts',(5.41299301948203,5.7821711650125,129.905577592736));
#54942=CARTESIAN_POINT('Ctrl Pts',(6.14848771365607,5.02280815117252,129.856663723811));
#54943=CARTESIAN_POINT('Ctrl Pts',(6.55155729124435,4.48440551749035,129.826341119464));
#54944=CARTESIAN_POINT('Ctrl Pts',(6.90486569511002,3.86120498475101,129.797100233172));
#54945=CARTESIAN_POINT('Ctrl Pts',(6.92739532360677,3.82063716295443,129.795219334459));
#54946=CARTESIAN_POINT('Ctrl Pts',(6.95529007101208,3.76935067364485,129.792869415242));
#54947=CARTESIAN_POINT('Ctrl Pts',(6.96098927351625,3.75881534642264,129.792388164429));
#54948=CARTESIAN_POINT('Ctrl Pts',(6.96992703207091,3.74220330565532,129.791631638365));
#54949=CARTESIAN_POINT('Ctrl Pts',(6.97318160791635,3.73613525940729,129.791355778087));
#54950=CARTESIAN_POINT('Ctrl Pts',(6.97891353453246,3.72541469644168,129.79086926035));
#54951=CARTESIAN_POINT('Ctrl Pts',(6.98139416334596,3.72076394294004,129.790658483422));
#54952=CARTESIAN_POINT('Ctrl Pts',(6.98706046349019,3.710114985596,129.790176506358));
#54953=CARTESIAN_POINT('Ctrl Pts',(6.99024306444631,3.70411514765395,129.789905418144));
#54954=CARTESIAN_POINT('Ctrl Pts',(6.99897160518982,3.68760879346859,129.78916089943));
#54955=CARTESIAN_POINT('Ctrl Pts',(7.00450162070745,3.67709385127044,129.788688048122));
#54956=CARTESIAN_POINT('Ctrl Pts',(7.03357417576426,3.62151082991424,129.786195990742));
#54957=CARTESIAN_POINT('Ctrl Pts',(7.0567057497454,3.57622852511627,129.784191699709));
#54958=CARTESIAN_POINT('Ctrl Pts',(7.33623988730976,3.01573928471543,129.759693960859));
#54959=CARTESIAN_POINT('Ctrl Pts',(7.53613457561179,2.47423775956985,129.739426712922));
#54960=CARTESIAN_POINT('Ctrl Pts',(7.78175836120098,1.4901746636461,129.704630106344));
#54961=CARTESIAN_POINT('Ctrl Pts',(7.85240419935489,1.05645206810225,129.689882829755));
#54962=CARTESIAN_POINT('Ctrl Pts',(7.89189627365271,0.553392608066614,129.671517693239));
#54963=CARTESIAN_POINT('Ctrl Pts',(7.89623517872882,0.4875857633679,129.669089836548));
#54964=CARTESIAN_POINT('Ctrl Pts',(7.90142894480188,0.390298131621056,129.665453328132));
#54965=CARTESIAN_POINT('Ctrl Pts',(7.90291947863621,0.358853281744243,129.664270674074));
#54966=CARTESIAN_POINT('Ctrl Pts',(7.90914218715489,0.208622464443032,129.658582233375));
#54967=CARTESIAN_POINT('Ctrl Pts',(7.91138390237421,0.0897536189072339,
129.653967339659));
#54968=CARTESIAN_POINT('Ctrl Pts',(7.91090739964824,-0.0397183049235798,
129.648773925764));
#54969=CARTESIAN_POINT('Ctrl Pts',(7.91084705873395,-0.0503213750072018,
129.64834739304));
#54970=CARTESIAN_POINT('Ctrl Pts',(7.91073288312687,-0.0651466138367077,
129.647749269595));
#54971=CARTESIAN_POINT('Ctrl Pts',(7.91069698433689,-0.069368950915418,
129.647578721792));
#54972=CARTESIAN_POINT('Ctrl Pts',(7.91062905017654,-0.0766715024336212,
129.647283413328));
#54973=CARTESIAN_POINT('Ctrl Pts',(7.91059859616372,-0.0797517341501573,
129.647158745351));
#54974=CARTESIAN_POINT('Ctrl Pts',(7.91053171446854,-0.0861390295293632,
129.646900006965));
#54975=CARTESIAN_POINT('Ctrl Pts',(7.91049501205948,-0.089446085388177,
129.646765920428));
#54976=CARTESIAN_POINT('Ctrl Pts',(7.91040463386372,-0.0971539956987106,
129.646453109994));
#54977=CARTESIAN_POINT('Ctrl Pts',(7.91034935952926,-0.101554814625001,
129.646274292468));
#54978=CARTESIAN_POINT('Ctrl Pts',(7.91017303965176,-0.114718269392096,
129.645738774668));
#54979=CARTESIAN_POINT('Ctrl Pts',(7.91004110655744,-0.123480726956874,
129.645381437396));
#54980=CARTESIAN_POINT('Ctrl Pts',(7.90969290272184,-0.144307972731015,
129.644530074622));
#54981=CARTESIAN_POINT('Ctrl Pts',(7.90946358783047,-0.156372491319765,
129.644035299601));
#54982=CARTESIAN_POINT('Ctrl Pts',(7.90692252491599,-0.275692275676478,
129.639126315437));
#54983=CARTESIAN_POINT('Ctrl Pts',(7.90245697727143,-0.382886144758461,
129.634591676301));
#54984=CARTESIAN_POINT('Ctrl Pts',(7.88285869803527,-0.698722364194374,
129.620930994689));
#54985=CARTESIAN_POINT('Ctrl Pts',(7.8616296712863,-0.906886636209906,129.611541876902));
#54986=CARTESIAN_POINT('Ctrl Pts',(7.79915128432483,-1.34617114277955,129.591241951095));
#54987=CARTESIAN_POINT('Ctrl Pts',(7.75581255659185,-1.57680218338523,129.580295971233));
#54988=CARTESIAN_POINT('Ctrl Pts',(7.6428324482774,-2.05886745411721,129.557190648255));
#54989=CARTESIAN_POINT('Ctrl Pts',(7.57087182499121,-2.30948694244284,129.545047239426));
#54990=CARTESIAN_POINT('Ctrl Pts',(7.33052846009506,-3.0134381865324,129.511055926809));
#54991=CARTESIAN_POINT('Ctrl Pts',(7.13279493832639,-3.4555468762655,129.489921457265));
#54992=CARTESIAN_POINT('Ctrl Pts',(6.87913559696617,-3.90673603390423,129.468867828611));
#54993=CARTESIAN_POINT('Ctrl Pts',(6.86216484522073,-3.93646880807375,129.467482476924));
#54994=CARTESIAN_POINT('Ctrl Pts',(6.83956830570848,-3.97546775100461,129.465667932728));
#54995=CARTESIAN_POINT('Ctrl Pts',(6.83411585527522,-3.98483361329514,129.465232352156));
#54996=CARTESIAN_POINT('Ctrl Pts',(6.82564832217963,-3.99931008925879,129.464559385364));
#54997=CARTESIAN_POINT('Ctrl Pts',(6.82264671667153,-4.00442854697359,129.464321501119));
#54998=CARTESIAN_POINT('Ctrl Pts',(6.81694308592173,-4.01412957738808,129.463870745154));
#54999=CARTESIAN_POINT('Ctrl Pts',(6.8142421923661,-4.0187128094301,129.463657831735));
#55000=CARTESIAN_POINT('Ctrl Pts',(6.80798760732958,-4.02930197904195,129.463166016779));
#55001=CARTESIAN_POINT('Ctrl Pts',(6.80443058532779,-4.03530594994363,129.462887238866));
#55002=CARTESIAN_POINT('Ctrl Pts',(6.79444293932496,-4.05211354913787,129.462107036371));
#55003=CARTESIAN_POINT('Ctrl Pts',(6.78799448524417,-4.0629065877836,129.461606273661));
#55004=CARTESIAN_POINT('Ctrl Pts',(6.75076134636459,-4.12488912559466,129.458731849942));
#55005=CARTESIAN_POINT('Ctrl Pts',(6.71942301739954,-4.17574467222141,129.456378840039));
#55006=CARTESIAN_POINT('Ctrl Pts',(6.62796946964134,-4.32045875950526,129.449695682521));
#55007=CARTESIAN_POINT('Ctrl Pts',(6.56644195907552,-4.4134096102045,129.445418581052));
#55008=CARTESIAN_POINT('Ctrl Pts',(6.3816689699917,-4.68012761580694,129.433164291611));
#55009=CARTESIAN_POINT('Ctrl Pts',(6.2533426760697,-4.85025826413037,129.425373838104));
#55010=CARTESIAN_POINT('Ctrl Pts',(6.04927732170652,-5.09921762141308,129.413868457297));
#55011=CARTESIAN_POINT('Ctrl Pts',(5.97852144814181,-5.18199366637929,129.410023598275));
#55012=CARTESIAN_POINT('Ctrl Pts',(5.85666426283911,-5.31873303507879,129.403610540762));
#55013=CARTESIAN_POINT('Ctrl Pts',(5.80647125119308,-5.37348389081887,129.401025310812));
#55014=CARTESIAN_POINT('Ctrl Pts',(5.73447987952777,-5.44982582348347,129.397387155292));
#55015=CARTESIAN_POINT('Ctrl Pts',(5.71331582082688,-5.47200907647653,129.396325896581));
#55016=CARTESIAN_POINT('Ctrl Pts',(5.67239885792624,-5.51440030161698,129.394289106614));
#55017=CARTESIAN_POINT('Ctrl Pts',(5.65266559469655,-5.5346265608705,129.393313387513));
#55018=CARTESIAN_POINT('Ctrl Pts',(5.26090063342465,-5.93189818182047,129.374064368405));
#55019=CARTESIAN_POINT('Ctrl Pts',(4.8520701733755,-6.27071072240029,129.356212789774));
#55020=CARTESIAN_POINT('Ctrl Pts',(4.39788981038583,-6.57592550202536,129.335461655056));
#55021=CARTESIAN_POINT('Ctrl Pts',(4.38324372108593,-6.58569703731295,129.334791500982));
#55022=CARTESIAN_POINT('Ctrl Pts',(4.35852925151662,-6.60206700003122,129.333658794064));
#55023=CARTESIAN_POINT('Ctrl Pts',(4.34847816834512,-6.60869151393633,129.333197620576));
#55024=CARTESIAN_POINT('Ctrl Pts',(4.26209319297185,-6.66534412411727,129.329229279156));
#55025=CARTESIAN_POINT('Ctrl Pts',(4.18492255806142,-6.71406531869149,129.32564926758));
#55026=CARTESIAN_POINT('Ctrl Pts',(4.09667450041951,-6.76766745399532,129.321511150001));
#55027=CARTESIAN_POINT('Ctrl Pts',(4.08641375227872,-6.7738679772388,129.3210294072));
#55028=CARTESIAN_POINT('Ctrl Pts',(4.07132982387217,-6.78293638129537,129.320320382868));
#55029=CARTESIAN_POINT('Ctrl Pts',(4.06651759015735,-6.78582251286835,129.320094058331));
#55030=CARTESIAN_POINT('Ctrl Pts',(4.05796264947474,-6.79094096032369,129.319691495099));
#55031=CARTESIAN_POINT('Ctrl Pts',(4.05422115726168,-6.79317531048874,129.319515361595));
#55032=CARTESIAN_POINT('Ctrl Pts',(4.04650864681758,-6.79777243830464,129.319152141992));
#55033=CARTESIAN_POINT('Ctrl Pts',(4.04253740141914,-6.80013483026173,129.318965036301));
#55034=CARTESIAN_POINT('Ctrl Pts',(4.03247077087613,-6.80611127569958,129.318490546266));
#55035=CARTESIAN_POINT('Ctrl Pts',(4.02637260348466,-6.80972061634238,129.318202924359));
#55036=CARTESIAN_POINT('Ctrl Pts',(4.01303271792971,-6.81759195112436,129.31757335311));
#55037=CARTESIAN_POINT('Ctrl Pts',(4.00578904836507,-6.82185060715984,129.317231238989));
#55038=CARTESIAN_POINT('Ctrl Pts',(3.984889500332,-6.83409298249173,129.316243469407));
#55039=CARTESIAN_POINT('Ctrl Pts',(3.97121649103379,-6.84204726668123,129.315596390136));
#55040=CARTESIAN_POINT('Ctrl Pts',(3.92507886680906,-6.86870297690741,129.313410254035));
#55041=CARTESIAN_POINT('Ctrl Pts',(3.89250557087163,-6.887214604848,129.311862416122));
#55042=CARTESIAN_POINT('Ctrl Pts',(3.75518395834791,-6.96397005377833,129.305322151524));
#55043=CARTESIAN_POINT('Ctrl Pts',(3.64925306414891,-7.020059534667,129.300240884743));
#55044=CARTESIAN_POINT('Ctrl Pts',(3.29646283485409,-7.19671561998329,129.283287143524));
#55045=CARTESIAN_POINT('Ctrl Pts',(3.04459970065764,-7.30683158574461,129.271140629791));
#55046=CARTESIAN_POINT('Ctrl Pts',(2.23340153544673,-7.61225475989284,129.232694668417));
#55047=CARTESIAN_POINT('Ctrl Pts',(1.65754935171165,-7.75803801676341,129.206541513892));
#55048=CARTESIAN_POINT('Ctrl Pts',(0.921091465282835,-7.85864757810112,
129.175609146083));
#55049=CARTESIAN_POINT('Ctrl Pts',(0.770826777392061,-7.87480663680732,
129.169413399779));
#55050=CARTESIAN_POINT('Ctrl Pts',(0.595787264230321,-7.88857132780115,
129.162317635424));
#55051=CARTESIAN_POINT('Ctrl Pts',(0.571378065165727,-7.89037687147383,
129.16133084789));
#55052=CARTESIAN_POINT('Ctrl Pts',(0.534988279795762,-7.89289886986167,
129.159863660815));
#55053=CARTESIAN_POINT('Ctrl Pts',(0.52301387961296,-7.89370138225325,129.159381504125));
#55054=CARTESIAN_POINT('Ctrl Pts',(0.50165419328376,-7.89508407105961,129.158522559316));
#55055=CARTESIAN_POINT('Ctrl Pts',(0.492269619898394,-7.89567476790448,
129.158145558017));
#55056=CARTESIAN_POINT('Ctrl Pts',(0.472564442680712,-7.89687981035193,
129.157354750841));
#55057=CARTESIAN_POINT('Ctrl Pts',(0.462243636710388,-7.89749065923035,
129.156941016903));
#55058=CARTESIAN_POINT('Ctrl Pts',(0.4352207889315,-7.89903688412155,129.155858943012));
#55059=CARTESIAN_POINT('Ctrl Pts',(0.418516899953101,-7.89993952123505,
129.15519127125));
#55060=CARTESIAN_POINT('Ctrl Pts',(0.34508054095335,-7.90367427224265,129.152261190549));
#55061=CARTESIAN_POINT('Ctrl Pts',(0.288320950494298,-7.90594831276918,
129.150010282648));
#55062=CARTESIAN_POINT('Ctrl Pts',(0.0248547349322873,-7.91366281803928,
129.139624025146));
#55063=CARTESIAN_POINT('Ctrl Pts',(-0.181994581528782,-7.91160919168103,
129.131649478971));
#55064=CARTESIAN_POINT('Ctrl Pts',(-0.50846275614695,-7.89555600854718,
129.119278936484));
#55065=CARTESIAN_POINT('Ctrl Pts',(-0.628244752409664,-7.88692895884645,
129.114785522644));
#55066=CARTESIAN_POINT('Ctrl Pts',(-0.832733076930153,-7.86751280488607,
129.107168119196));
#55067=CARTESIAN_POINT('Ctrl Pts',(-0.917545013881621,-7.85807314090975,
129.104024560447));
#55068=CARTESIAN_POINT('Ctrl Pts',(-1.06895012503899,-7.83873691797351,
129.098429753467));
#55069=CARTESIAN_POINT('Ctrl Pts',(-1.1356007192113,-7.82935897305758,129.095972757889));
#55070=CARTESIAN_POINT('Ctrl Pts',(-1.25714099059186,-7.81067320804819,
129.091496724122));
#55071=CARTESIAN_POINT('Ctrl Pts',(-1.31206748912966,-7.80163433965268,
129.089475559399));
#55072=CARTESIAN_POINT('Ctrl Pts',(-1.4899928020783,-7.77042225616164,129.082926607717));
#55073=CARTESIAN_POINT('Ctrl Pts',(-1.61256261272887,-7.74591392162776,
129.078412733197));
#55074=CARTESIAN_POINT('Ctrl Pts',(-2.05378137362495,-7.6467634549912,129.062055053318));
#55075=CARTESIAN_POINT('Ctrl Pts',(-2.36829112373877,-7.55527562981762,
129.050198239783));
#55076=CARTESIAN_POINT('Ctrl Pts',(-2.82376859410245,-7.39153819703612,
129.031823584912));
#55077=CARTESIAN_POINT('Ctrl Pts',(-2.96970486199796,-7.33412264768154,
129.025743108026));
#55078=CARTESIAN_POINT('Ctrl Pts',(-3.12658481318704,-7.26695127595329,
129.018909481708));
#55079=CARTESIAN_POINT('Ctrl Pts',(-3.13932289118435,-7.26145751364896,
129.01835244914));
#55080=CARTESIAN_POINT('Ctrl Pts',(-3.15715369779857,-7.25371163856656,
129.01756959496));
#55081=CARTESIAN_POINT('Ctrl Pts',(-3.16225864733913,-7.25148758904731,
129.017345105355));
#55082=CARTESIAN_POINT('Ctrl Pts',(-3.17109868464323,-7.24762518121592,
129.01695573737));
#55083=CARTESIAN_POINT('Ctrl Pts',(-3.17483486542168,-7.24598931908854,
129.016790979019));
#55084=CARTESIAN_POINT('Ctrl Pts',(-3.18233818183134,-7.24269712408581,
129.016459703236));
#55085=CARTESIAN_POINT('Ctrl Pts',(-3.18610529319005,-7.24104073979634,
129.01629318334));
#55086=CARTESIAN_POINT('Ctrl Pts',(-3.19503256705952,-7.23710713672802,
129.015898088563));
#55087=CARTESIAN_POINT('Ctrl Pts',(-3.20019158523816,-7.23482733937533,
129.015669387445));
#55088=CARTESIAN_POINT('Ctrl Pts',(-3.21594190812643,-7.22784704556899,
129.014970002825));
#55089=CARTESIAN_POINT('Ctrl Pts',(-3.22652529393118,-7.22312880931818,
129.014498439677));
#55090=CARTESIAN_POINT('Ctrl Pts',(-3.25091391035351,-7.21219169231584,
129.013407957208));
#55091=CARTESIAN_POINT('Ctrl Pts',(-3.26471169690569,-7.20595641051553,
129.012788203914));
#55092=CARTESIAN_POINT('Ctrl Pts',(-3.30987569331427,-7.18539025451225,
129.010750098722));
#55093=CARTESIAN_POINT('Ctrl Pts',(-3.34116575711271,-7.17089405819668,
129.009322975773));
#55094=CARTESIAN_POINT('Ctrl Pts',(-3.44542471623478,-7.12176196274324,
129.004515166055));
#55095=CARTESIAN_POINT('Ctrl Pts',(-3.51795535294535,-7.08621438474711,
129.001085133643));
#55096=CARTESIAN_POINT('Ctrl Pts',(-3.72555200901987,-6.98049765596603,
128.991047145746));
#55097=CARTESIAN_POINT('Ctrl Pts',(-3.85915065363965,-6.90753485709335,
128.984313902631));
#55098=CARTESIAN_POINT('Ctrl Pts',(-4.8020564877276,-6.35668629550347,128.935231515196));
#55099=CARTESIAN_POINT('Ctrl Pts',(-5.52289895765142,-5.74156978568193,
128.890439753823));
#55100=CARTESIAN_POINT('Ctrl Pts',(-6.15415533931288,-4.97125639215908,
128.849629002045));
#55101=CARTESIAN_POINT('Ctrl Pts',(-6.18897452030067,-4.92784056284967,
128.847367171728));
#55102=CARTESIAN_POINT('Ctrl Pts',(-6.23056801416275,-4.87484159219013,
128.844651692421));
#55103=CARTESIAN_POINT('Ctrl Pts',(-6.23778238747645,-4.86560676751734,
128.844180188424));
#55104=CARTESIAN_POINT('Ctrl Pts',(-6.24957389195036,-4.85044361505746,
128.84340870318));
#55105=CARTESIAN_POINT('Ctrl Pts',(-6.25416315872756,-4.8445247732076,128.843108230985));
#55106=CARTESIAN_POINT('Ctrl Pts',(-6.26237244798331,-4.83390603094904,
128.842570367938));
#55107=CARTESIAN_POINT('Ctrl Pts',(-6.26599559911505,-4.82920856304417,
128.842332850796));
#55108=CARTESIAN_POINT('Ctrl Pts',(-6.27366293469632,-4.81924459568909,
128.841829932976));
#55109=CARTESIAN_POINT('Ctrl Pts',(-6.27770578057585,-4.8139770693335,128.841564586344));
#55110=CARTESIAN_POINT('Ctrl Pts',(-6.28845733872629,-4.79993201519237,
128.840858473963));
#55111=CARTESIAN_POINT('Ctrl Pts',(-6.29515431560334,-4.79114549930291,
128.84041818067));
#55112=CARTESIAN_POINT('Ctrl Pts',(-6.3262598330114,-4.75015686839619,128.838370944721));
#55113=CARTESIAN_POINT('Ctrl Pts',(-6.35044003915959,-4.71778180092387,
128.836773168659));
#55114=CARTESIAN_POINT('Ctrl Pts',(-6.52854172573438,-4.47546966424367,
128.824955111149));
#55115=CARTESIAN_POINT('Ctrl Pts',(-6.67227129524531,-4.25822686897696,
128.815146732692));
#55116=CARTESIAN_POINT('Ctrl Pts',(-7.16149193801664,-3.43300768199062,
128.780242608167));
#55117=CARTESIAN_POINT('Ctrl Pts',(-7.43665934655047,-2.78720803995153,
128.757676826845));
#55118=CARTESIAN_POINT('Ctrl Pts',(-7.62986155918095,-2.09038704010946,
128.73236860291));
#55119=CARTESIAN_POINT('Ctrl Pts',(-7.63621363906149,-2.06706232111607,
128.731520024128));
#55120=CARTESIAN_POINT('Ctrl Pts',(-7.68145996812508,-1.89786347245794,
128.725351856212));
#55121=CARTESIAN_POINT('Ctrl Pts',(-7.71627710689242,-1.75093618387331,
128.719928564604));
#55122=CARTESIAN_POINT('Ctrl Pts',(-7.75115366938685,-1.58239851251141,
128.713546804146));
#55123=CARTESIAN_POINT('Ctrl Pts',(-7.75535617579685,-1.56167180775897,
128.712759220317));
#55124=CARTESIAN_POINT('Ctrl Pts',(-7.76385738555075,-1.5188632522641,128.711126440375));
#55125=CARTESIAN_POINT('Ctrl Pts',(-7.76814510519658,-1.49677944015832,
128.710280779733));
#55126=CARTESIAN_POINT('Ctrl Pts',(-7.77419697540246,-1.46488285624314,
128.709054155996));
#55127=CARTESIAN_POINT('Ctrl Pts',(-7.77603688367703,-1.45508445691838,
128.708676638923));
#55128=CARTESIAN_POINT('Ctrl Pts',(-7.77981816489373,-1.43473530957747,
128.707891104335));
#55129=CARTESIAN_POINT('Ctrl Pts',(-7.78175660734259,-1.42418404351131,
128.707482951751));
#55130=CARTESIAN_POINT('Ctrl Pts',(-7.78529349746118,-1.40470934399531,
128.706728008242));
#55131=CARTESIAN_POINT('Ctrl Pts',(-7.78689808210129,-1.39578703270446,
128.706381509813));
#55132=CARTESIAN_POINT('Ctrl Pts',(-7.78999616521076,-1.378388487765,128.70570459182));
#55133=CARTESIAN_POINT('Ctrl Pts',(-7.79149117478306,-1.36991253355285,
128.705374246068));
#55134=CARTESIAN_POINT('Ctrl Pts',(-7.79482982655388,-1.35080178897157,
128.704628086421));
#55135=CARTESIAN_POINT('Ctrl Pts',(-7.79666553954444,-1.34016564673749,
128.704211882274));
#55136=CARTESIAN_POINT('Ctrl Pts',(-7.81081944440454,-1.25714436603091,
128.700955717339));
#55137=CARTESIAN_POINT('Ctrl Pts',(-7.82215074580334,-1.18459673614096,
128.698066172737));
#55138=CARTESIAN_POINT('Ctrl Pts',(-7.83379587279434,-1.10256617792574,
128.694739142725));
#55139=CARTESIAN_POINT('Ctrl Pts',(-7.83510478100933,-1.0932259704374,128.69435944617));
#55140=CARTESIAN_POINT('Ctrl Pts',(-7.83698441685395,-1.0796363430689,128.693805706632));
#55141=CARTESIAN_POINT('Ctrl Pts',(-7.83756840187929,-1.07538873390447,
128.693632444242));
#55142=CARTESIAN_POINT('Ctrl Pts',(-7.83859400836142,-1.06788378460026,
128.693325984708));
#55143=CARTESIAN_POINT('Ctrl Pts',(-7.83903705233508,-1.06462664691495,
128.693192872231));
#55144=CARTESIAN_POINT('Ctrl Pts',(-7.83995417095694,-1.05785263174646,
128.692915805569));
#55145=CARTESIAN_POINT('Ctrl Pts',(-7.84042790936712,-1.0543357108317,128.692771831662));
#55146=CARTESIAN_POINT('Ctrl Pts',(-7.84138198588751,-1.04721667166443,
128.692480140976));
#55147=CARTESIAN_POINT('Ctrl Pts',(-7.84186220867543,-1.04361453903094,
128.692332417475));
#55148=CARTESIAN_POINT('Ctrl Pts',(-7.8430327658275,-1.03478780781344,128.691970111676));
#55149=CARTESIAN_POINT('Ctrl Pts',(-7.84372036102039,-1.02956285427189,
128.691755370107));
#55150=CARTESIAN_POINT('Ctrl Pts',(-7.84559523237534,-1.01520503777121,
128.691164524982));
#55151=CARTESIAN_POINT('Ctrl Pts',(-7.84677177881892,-1.00607080702518,
128.690787804594));
#55152=CARTESIAN_POINT('Ctrl Pts',(-7.88984058046698,-0.667030463361971,
128.676774516862));
#55153=CARTESIAN_POINT('Ctrl Pts',(-7.9109004823013,-0.33484439240435,128.66198909247));
#55154=CARTESIAN_POINT('Ctrl Pts',(-7.91099964813049,-0.00235950828826645,
128.646812588333));
#55155=CARTESIAN_POINT('',(-7.89935487361401,-0.000512643485807648,126.642299148188));
#55156=CARTESIAN_POINT('Ctrl Pts',(-7.91099958186279,-0.00257211328256086,
128.642116733665));
#55157=CARTESIAN_POINT('Ctrl Pts',(-7.91106172871082,0.188571757426559,
128.634395854378));
#55158=CARTESIAN_POINT('Ctrl Pts',(-7.90419210364439,0.38000650194112,128.62667497509));
#55159=CARTESIAN_POINT('Ctrl Pts',(-7.89035363924545,0.571174620975065,
128.618954095803));
#55160=CARTESIAN_POINT('Ctrl Pts',(-7.87652865224551,0.762156559740664,
128.611240735946));
#55161=CARTESIAN_POINT('Ctrl Pts',(-7.85574836118812,0.952872032041322,
128.603527376088));
#55162=CARTESIAN_POINT('Ctrl Pts',(-7.82802767564603,1.14276144024897,128.595814016231));
#55163=CARTESIAN_POINT('Ctrl Pts',(-7.8003282871574,1.33250496155664,128.58810658234));
#55164=CARTESIAN_POINT('Ctrl Pts',(-7.76569917123154,1.52142332597649,128.580399148449));
#55165=CARTESIAN_POINT('Ctrl Pts',(-7.72420720923037,1.7089599143554,128.572691714558));
#55166=CARTESIAN_POINT('Ctrl Pts',(-7.68273860412503,1.89639093355058,128.56498861938));
#55167=CARTESIAN_POINT('Ctrl Pts',(-7.63441492322061,2.08244137308628,128.557285524202));
#55168=CARTESIAN_POINT('Ctrl Pts',(-7.57935450900709,2.26656264568044,128.549582429024));
#55169=CARTESIAN_POINT('Ctrl Pts',(-7.52430732046374,2.45063969181429,128.541881184152));
#55170=CARTESIAN_POINT('Ctrl Pts',(-7.46252671801311,2.63278814539991,128.53417993928));
#55171=CARTESIAN_POINT('Ctrl Pts',(-7.39418155640331,2.81247224180881,128.526478694408));
#55172=CARTESIAN_POINT('Ctrl Pts',(-7.32584333515808,2.99213809152539,128.518778231587));
#55173=CARTESIAN_POINT('Ctrl Pts',(-7.25094200948829,3.16933974335435,128.511077768767));
#55174=CARTESIAN_POINT('Ctrl Pts',(-7.16969543935455,3.34355922736515,128.503377305946));
#55175=CARTESIAN_POINT('Ctrl Pts',(-7.08844202745983,3.51779338237148,128.495676194671));
#55176=CARTESIAN_POINT('Ctrl Pts',(-7.00084246024951,3.68904454119845,128.487975083396));
#55177=CARTESIAN_POINT('Ctrl Pts',(-6.90716162491653,3.85681724836431,128.480273972121));
#55178=CARTESIAN_POINT('Ctrl Pts',(-6.81345549385595,4.0246352575675,128.472570781389));
#55179=CARTESIAN_POINT('Ctrl Pts',(-6.71366500237783,4.18897262927833,128.464867590657));
#55180=CARTESIAN_POINT('Ctrl Pts',(-6.60809962107566,4.34936091833499,128.457164399926));
#55181=CARTESIAN_POINT('Ctrl Pts',(-6.50242721631475,4.50991181097648,128.449453399606));
#55182=CARTESIAN_POINT('Ctrl Pts',(-6.39096842749255,4.6665053217451,128.441742399287));
#55183=CARTESIAN_POINT('Ctrl Pts',(-6.27407502337237,4.81870351869618,128.434031398967));
#55184=CARTESIAN_POINT('Ctrl Pts',(-6.15712015557712,4.97098174292163,128.42631634413));
#55185=CARTESIAN_POINT('Ctrl Pts',(-6.03472521100803,5.11885977170499,128.418601289292));
#55186=CARTESIAN_POINT('Ctrl Pts',(-5.90728030952362,5.26193503805534,128.410886234455));
#55187=CARTESIAN_POINT('Ctrl Pts',(-5.77965213476975,5.40521605505981,128.403160084914));
#55188=CARTESIAN_POINT('Ctrl Pts',(-5.64695974637582,5.54368025222585,128.395433935374));
#55189=CARTESIAN_POINT('Ctrl Pts',(-5.50962884540655,5.6769631834163,128.387707785833));
#55190=CARTESIAN_POINT('Ctrl Pts',(-5.39040784340672,5.79267002356551,128.381000487743));
#55191=CARTESIAN_POINT('Ctrl Pts',(-5.26769167971134,5.90447255479126,128.374293189652));
#55192=CARTESIAN_POINT('Ctrl Pts',(-5.14177698783451,6.01215854809032,128.367585891562));
#55193=CARTESIAN_POINT('Ctrl Pts',(-4.99326218119857,6.13917283239523,128.359674717226));
#55194=CARTESIAN_POINT('Ctrl Pts',(-4.83983861260918,6.26085156460908,128.35176354289));
#55195=CARTESIAN_POINT('Ctrl Pts',(-4.68192541788834,6.37679350311197,128.343852368553));
#55196=CARTESIAN_POINT('Ctrl Pts',(-4.52418342157298,6.4926097455004,128.335949770957));
#55197=CARTESIAN_POINT('Ctrl Pts',(-4.36196176958607,6.60270138012032,128.328047173361));
#55198=CARTESIAN_POINT('Ctrl Pts',(-4.19571460999561,6.70670559302176,128.320144575765));
#55199=CARTESIAN_POINT('Ctrl Pts',(-4.02961682378772,6.81061635794419,128.312249078667));
#55200=CARTESIAN_POINT('Ctrl Pts',(-3.85950102570916,6.90845041525919,128.30435358157));
#55201=CARTESIAN_POINT('Ctrl Pts',(-3.68585267577465,6.9998865028288,128.296458084472));
#55202=CARTESIAN_POINT('Ctrl Pts',(-3.51232812523016,7.09125740272533,128.288568216324));
#55203=CARTESIAN_POINT('Ctrl Pts',(-3.33527634435184,7.17623926057323,128.280678348175));
#55204=CARTESIAN_POINT('Ctrl Pts',(-3.15521012463939,7.25455512553134,128.272788480027));
#55205=CARTESIAN_POINT('Ctrl Pts',(-2.97523887235613,7.33282968648267,128.264902773017));
#55206=CARTESIAN_POINT('Ctrl Pts',(-2.79225666464164,7.40444512278129,128.257017066007));
#55207=CARTESIAN_POINT('Ctrl Pts',(-2.60679940000116,7.469171164738,128.249131358998));
#55208=CARTESIAN_POINT('Ctrl Pts',(-2.42140554399758,7.53387507658241,128.241248348145));
#55209=CARTESIAN_POINT('Ctrl Pts',(-2.23353864282103,7.59169417522488,128.233365337292));
#55210=CARTESIAN_POINT('Ctrl Pts',(-2.0437532717983,7.64244683095759,128.22548232644));
#55211=CARTESIAN_POINT('Ctrl Pts',(-1.85396506851317,7.69320024409768,128.217599197945));
#55212=CARTESIAN_POINT('Ctrl Pts',(-1.66225866908416,7.73688690636788,128.20971606945));
#55213=CARTESIAN_POINT('Ctrl Pts',(-1.46920302329791,7.77337529496243,128.201832940955));
#55214=CARTESIAN_POINT('Ctrl Pts',(-1.27613544068857,7.80986593967044,128.193949325039));
#55215=CARTESIAN_POINT('Ctrl Pts',(-1.08171878440958,7.83915735916659,128.186065709122));
#55216=CARTESIAN_POINT('Ctrl Pts',(-0.886531428151984,7.86116931676826,
128.178182093206));
#55217=CARTESIAN_POINT('Ctrl Pts',(-0.691299193308703,7.88318633548426,
128.170296664644));
#55218=CARTESIAN_POINT('Ctrl Pts',(-0.495296248158198,7.89792051846848,
128.162411236081));
#55219=CARTESIAN_POINT('Ctrl Pts',(-0.299105555518819,7.90534356411268,
128.154525807519));
#55220=CARTESIAN_POINT('Ctrl Pts',(-0.102836774566898,7.91276956429617,
128.146637240379));
#55221=CARTESIAN_POINT('Ctrl Pts',(0.0936195583692437,7.91287861566962,
128.138748673239));
#55222=CARTESIAN_POINT('Ctrl Pts',(0.289680765627241,7.90569453331114,128.130860106098));
#55223=CARTESIAN_POINT('Ctrl Pts',(0.485950624630045,7.89850280552733,128.122963143808));
#55224=CARTESIAN_POINT('Ctrl Pts',(0.681824173259923,7.88400245382682,128.115066181517));
#55225=CARTESIAN_POINT('Ctrl Pts',(0.876723026443754,7.86226924843606,128.107169219226));
#55226=CARTESIAN_POINT('Ctrl Pts',(1.0717407419997,7.84052278868128,128.099267440839));
#55227=CARTESIAN_POINT('Ctrl Pts',(1.26578223682056,7.81153473195795,128.091365662452));
#55228=CARTESIAN_POINT('Ctrl Pts',(1.45827932920525,7.77543197501031,128.083463884065));
#55229=CARTESIAN_POINT('Ctrl Pts',(1.65102538679948,7.73928252473168,128.07555188595));
#55230=CARTESIAN_POINT('Ctrl Pts',(1.84222271693521,7.69600007051652,128.067639887835));
#55231=CARTESIAN_POINT('Ctrl Pts',(2.03131720799035,7.64576166255019,128.05972788972));
#55232=CARTESIAN_POINT('Ctrl Pts',(2.1105458553854,7.62471228618686,128.056412843865));
#55233=CARTESIAN_POINT('Ctrl Pts',(2.18940556887713,7.60244236409492,128.05309779801));
#55234=CARTESIAN_POINT('Ctrl Pts',(2.26785664693886,7.5789674249818,128.049782752154));
#55235=CARTESIAN_POINT('Ctrl Pts',(2.45507563422432,7.52294583246921,128.041871585818));
#55236=CARTESIAN_POINT('Ctrl Pts',(2.64046920377942,7.45990767774175,128.033960419481));
#55237=CARTESIAN_POINT('Ctrl Pts',(2.82347302936848,7.38998789257661,128.026049253144));
#55238=CARTESIAN_POINT('Ctrl Pts',(3.00627848460446,7.32014389824494,128.018146662261));
#55239=CARTESIAN_POINT('Ctrl Pts',(3.1866990363679,7.24343325359218,128.010244071378));
#55240=CARTESIAN_POINT('Ctrl Pts',(3.36418369101412,7.16004113766915,128.002341480496));
#55241=CARTESIAN_POINT('Ctrl Pts',(3.54150890401893,7.07672393625562,127.99444598883));
#55242=CARTESIAN_POINT('Ctrl Pts',(3.715903163777,6.98673736627402,127.986550497164));
#55243=CARTESIAN_POINT('Ctrl Pts',(3.8868334398217,6.89031543625427,127.978655005498));
#55244=CARTESIAN_POINT('Ctrl Pts',(4.05764188186214,6.7939622329113,127.970765141503));
#55245=CARTESIAN_POINT('Ctrl Pts',(4.22499096021781,6.69118297700458,127.962875277508));
#55246=CARTESIAN_POINT('Ctrl Pts',(4.38837008345159,6.58225865570984,127.954985413513));
#55247=CARTESIAN_POINT('Ctrl Pts',(4.55166306643892,6.4733917638326,127.947099709381));
#55248=CARTESIAN_POINT('Ctrl Pts',(4.7109899789148,6.35838645340526,127.93921400525));
#55249=CARTESIAN_POINT('Ctrl Pts',(4.86586694901607,6.23756842322976,127.931328301118));
#55250=CARTESIAN_POINT('Ctrl Pts',(5.02069099100115,6.11679168176707,127.92344529187));
#55251=CARTESIAN_POINT('Ctrl Pts',(5.17106784993921,5.99020639148181,127.915562282623));
#55252=CARTESIAN_POINT('Ctrl Pts',(5.31654442003831,5.85818030020923,127.907679273375));
#55253=CARTESIAN_POINT('Ctrl Pts',(5.46202319627846,5.72615220677108,127.899796144582));
#55254=CARTESIAN_POINT('Ctrl Pts',(5.60260127418626,5.58868337294279,127.89191301579));
#55255=CARTESIAN_POINT('Ctrl Pts',(5.73785987772008,5.44618077405168,127.884029886997));
#55256=CARTESIAN_POINT('Ctrl Pts',(5.873126864792,5.30366934262839,127.876146269595));
#55257=CARTESIAN_POINT('Ctrl Pts',(6.00307348253585,5.15612377428628,127.868262652194));
#55258=CARTESIAN_POINT('Ctrl Pts',(6.12731895789229,5.00398674940829,127.860379034793));
#55259=CARTESIAN_POINT('Ctrl Pts',(6.2515930191803,4.85181472141595,127.852493603558));
#55260=CARTESIAN_POINT('Ctrl Pts',(6.37016310612351,4.69504939904889,127.844608172324));
#55261=CARTESIAN_POINT('Ctrl Pts',(6.48268961331282,4.53416545545551,127.836722741089));
#55262=CARTESIAN_POINT('Ctrl Pts',(6.59526092552886,4.37321745220568,127.828834170088));
#55263=CARTESIAN_POINT('Ctrl Pts',(6.70178366549696,4.20814784245497,127.820945599088));
#55264=CARTESIAN_POINT('Ctrl Pts',(6.80196218870793,4.03945929344358,127.813057028087));
#55265=CARTESIAN_POINT('Ctrl Pts',(6.90224734612939,3.8705911852845,127.805160060161));
#55266=CARTESIAN_POINT('Ctrl Pts',(6.99617462204756,3.69809674021043,127.797263092235));
#55267=CARTESIAN_POINT('Ctrl Pts',(7.08349436800469,3.52250316372403,127.789366124309));
#55268=CARTESIAN_POINT('Ctrl Pts',(7.17086737866326,3.34680247584693,127.781464339264));
#55269=CARTESIAN_POINT('Ctrl Pts',(7.25162468227645,3.16799920115032,127.773562554219));
#55270=CARTESIAN_POINT('Ctrl Pts',(7.32556513212973,2.98663966606704,127.765660769173));
#55271=CARTESIAN_POINT('Ctrl Pts',(7.39960122658241,2.80504553598045,127.757748762888));
#55272=CARTESIAN_POINT('Ctrl Pts',(7.46680273664315,2.6208888638439,127.749836756604));
#55273=CARTESIAN_POINT('Ctrl Pts',(7.52701829413885,2.43473131981726,127.741924750319));
#55274=CARTESIAN_POINT('Ctrl Pts',(7.5522479675282,2.35673330352235,127.738609704461));
#55275=CARTESIAN_POINT('Ctrl Pts',(7.57625185913851,2.27838416024166,127.735294658604));
#55276=CARTESIAN_POINT('Ctrl Pts',(7.59902151349563,2.19972567322168,127.731979612747));
#55277=CARTESIAN_POINT('Ctrl Pts',(7.65287352100478,2.0136922197831,127.724139270877));
#55278=CARTESIAN_POINT('Ctrl Pts',(7.69997090489175,1.82540023104041,127.716298929008));
#55279=CARTESIAN_POINT('Ctrl Pts',(7.74011829435845,1.63538673999076,127.708458587139));
#55280=CARTESIAN_POINT('Ctrl Pts',(7.78022079784872,1.44558568967996,127.700627011005));
#55281=CARTESIAN_POINT('Ctrl Pts',(7.81338870739113,1.25406730994041,127.692795434872));
#55282=CARTESIAN_POINT('Ctrl Pts',(7.83947589528888,1.06138526802695,127.684963858738));
#55283=CARTESIAN_POINT('Ctrl Pts',(7.86553898941218,0.868881184645354,127.677139515743));
#55284=CARTESIAN_POINT('Ctrl Pts',(7.88453433858239,0.675215925305001,127.669315172747));
#55285=CARTESIAN_POINT('Ctrl Pts',(7.89636645732686,0.480955061937415,127.661490829751));
#55286=CARTESIAN_POINT('Ctrl Pts',(7.90818994755206,0.28683586242901,127.653672192622));
#55287=CARTESIAN_POINT('Ctrl Pts',(7.91286059039629,0.0921222733201361,
127.645853555494));
#55288=CARTESIAN_POINT('Ctrl Pts',(7.91033447821782,-0.102613072843991,
127.638034918365));
#55289=CARTESIAN_POINT('Ctrl Pts',(7.90780971744413,-0.297244240626218,
127.630220464005));
#55290=CARTESIAN_POINT('Ctrl Pts',(7.89809587570351,-0.491896791618777,
127.622406009645));
#55291=CARTESIAN_POINT('Ctrl Pts',(7.88120108631204,-0.685995945406346,
127.614591555286));
#55292=CARTESIAN_POINT('Ctrl Pts',(7.86431205381443,-0.880028959971861,
127.606779763698));
#55293=CARTESIAN_POINT('Ctrl Pts',(7.84024697948718,-1.07350860319827,127.598967972111));
#55294=CARTESIAN_POINT('Ctrl Pts',(7.8090660238239,-1.26586288181586,127.591156180524));
#55295=CARTESIAN_POINT('Ctrl Pts',(7.77788360884144,-1.45822616292499,127.583344023333));
#55296=CARTESIAN_POINT('Ctrl Pts',(7.73958469440379,-1.64946362564282,127.575531866141));
#55297=CARTESIAN_POINT('Ctrl Pts',(7.69428104737915,-1.83901064813178,127.56771970895));
#55298=CARTESIAN_POINT('Ctrl Pts',(7.64897369674031,-2.02857316626157,127.559906913107));
#55299=CARTESIAN_POINT('Ctrl Pts',(7.59666055379395,-2.21644462644084,127.552094117265));
#55300=CARTESIAN_POINT('Ctrl Pts',(7.53750401571364,-2.40207289920618,127.544281321422));
#55301=CARTESIAN_POINT('Ctrl Pts',(7.47833223243184,-2.58774901013972,127.536466512148));
#55302=CARTESIAN_POINT('Ctrl Pts',(7.41231364743956,-2.77118044686703,127.528651702874));
#55303=CARTESIAN_POINT('Ctrl Pts',(7.33965986070732,-2.95183233418192,127.5208368936));
#55304=CARTESIAN_POINT('Ctrl Pts',(7.26697456525496,-3.13256256716894,127.513018695175));
#55305=CARTESIAN_POINT('Ctrl Pts',(7.18764846688821,-3.3105105234454,127.50520049675));
#55306=CARTESIAN_POINT('Ctrl Pts',(7.10194048161173,-3.48516318063366,127.497382298325));
#55307=CARTESIAN_POINT('Ctrl Pts',(7.01613273270517,-3.6600191325678,127.489554999559));
#55308=CARTESIAN_POINT('Ctrl Pts',(6.92392841514536,-3.83157180867922,127.481727700794));
#55309=CARTESIAN_POINT('Ctrl Pts',(6.8256319507697,-3.99933362857262,127.473900402028));
#55310=CARTESIAN_POINT('Ctrl Pts',(6.72727131806158,-4.1672049640656,127.46606799357));
#55311=CARTESIAN_POINT('Ctrl Pts',(6.62281080130682,-4.33128021613375,127.458235585112));
#55312=CARTESIAN_POINT('Ctrl Pts',(6.51259701665135,-4.4911024368972,127.450403176654));
#55313=CARTESIAN_POINT('Ctrl Pts',(6.40222505968386,-4.65115402506918,127.442559527586));
#55314=CARTESIAN_POINT('Ctrl Pts',(6.28608355310373,-4.80694011032984,127.434715878518));
#55315=CARTESIAN_POINT('Ctrl Pts',(6.16455883936316,-4.95803744600921,127.426872229451));
#55316=CARTESIAN_POINT('Ctrl Pts',(6.09899207259603,-5.03955966040235,127.422640310747));
#55317=CARTESIAN_POINT('Ctrl Pts',(6.03185890404331,-5.11971762872589,127.418408392043));
#55318=CARTESIAN_POINT('Ctrl Pts',(5.96322422567988,-5.19844956061561,127.41417647334));
#55319=CARTESIAN_POINT('Ctrl Pts',(5.83481144673563,-5.34575390306584,127.406258720187));
#55320=CARTESIAN_POINT('Ctrl Pts',(5.70075682129387,-5.48850438542768,127.398340967034));
#55321=CARTESIAN_POINT('Ctrl Pts',(5.56141446608958,-5.62624120851298,127.390423213881));
#55322=CARTESIAN_POINT('Ctrl Pts',(5.42223220522564,-5.7638197818988,127.382514557657));
#55323=CARTESIAN_POINT('Ctrl Pts',(5.27777455793322,-5.89639592985943,127.374605901433));
#55324=CARTESIAN_POINT('Ctrl Pts',(5.1284360564711,-6.02354253032941,127.366697245209));
#55325=CARTESIAN_POINT('Ctrl Pts',(4.97924148956077,-6.15056658511443,127.358796211459));
#55326=CARTESIAN_POINT('Ctrl Pts',(4.82517570004318,-6.27217129531622,127.350895177709));
#55327=CARTESIAN_POINT('Ctrl Pts',(4.66667045601083,-6.38796586207187,127.342994143959));
#55328=CARTESIAN_POINT('Ctrl Pts',(4.50828865030388,-6.50367025207977,127.335099263257));
#55329=CARTESIAN_POINT('Ctrl Pts',(4.34547455493314,-6.61357331112474,127.327204382555));
#55330=CARTESIAN_POINT('Ctrl Pts',(4.17869366249202,-6.71732389237329,127.319309501853));
#55331=CARTESIAN_POINT('Ctrl Pts',(4.01201179833126,-6.82101287039201,127.311419308837));
#55332=CARTESIAN_POINT('Ctrl Pts',(3.84136812198953,-6.91855646840522,127.303529115822));
#55333=CARTESIAN_POINT('Ctrl Pts',(3.66725803943821,-7.00964617310859,127.295638922806));
#55334=CARTESIAN_POINT('Ctrl Pts',(3.4932191321903,-7.10069864081066,127.28775195526));
#55335=CARTESIAN_POINT('Ctrl Pts',(3.31571694760427,-7.18530231387692,127.279864987715));
#55336=CARTESIAN_POINT('Ctrl Pts',(3.13527272864077,-7.26319391982904,127.271978020169));
#55337=CARTESIAN_POINT('Ctrl Pts',(2.95484418002647,-7.34107876142665,127.264091737553));
#55338=CARTESIAN_POINT('Ctrl Pts',(2.77147441962109,-7.41225255487031,127.256205454936));
#55339=CARTESIAN_POINT('Ctrl Pts',(2.58570644708443,-7.47649939273093,127.24831917232));
#55340=CARTESIAN_POINT('Ctrl Pts',(2.39993880106107,-7.54074611766872,127.240432903565));
#55341=CARTESIAN_POINT('Ctrl Pts',(2.21177327678238,-7.5980657981353,127.23254663481));
#55342=CARTESIAN_POINT('Ctrl Pts',(2.02176998328062,-7.64829177886837,127.224660366055));
#55343=CARTESIAN_POINT('Ctrl Pts',(1.83173517819691,-7.69852608945761,127.216772789381));
#55344=CARTESIAN_POINT('Ctrl Pts',(1.63986232970381,-7.74166426807933,127.208885212708));
#55345=CARTESIAN_POINT('Ctrl Pts',(1.44672398292726,-7.77759028987919,127.200997636034));
#55346=CARTESIAN_POINT('Ctrl Pts',(1.25352123350256,-7.81352829133498,127.193107429221));
#55347=CARTESIAN_POINT('Ctrl Pts',(1.05905248352351,-7.84224928124183,127.185217222408));
#55348=CARTESIAN_POINT('Ctrl Pts',(0.863897930628899,-7.86368878869549,
127.177327015595));
#55349=CARTESIAN_POINT('Ctrl Pts',(0.668554924532715,-7.88514899945204,
127.169429189514));
#55350=CARTESIAN_POINT('Ctrl Pts',(0.472525135347926,-7.89931364542681,
127.161531363434));
#55351=CARTESIAN_POINT('Ctrl Pts',(0.276392376396081,-7.90617026469011,
127.153633537353));
#55352=CARTESIAN_POINT('Ctrl Pts',(0.080151015028995,-7.91303068059308,
127.145731338097));
#55353=CARTESIAN_POINT('Ctrl Pts',(-0.116193085992988,-7.91257500240236,
127.137829138841));
#55354=CARTESIAN_POINT('Ctrl Pts',(-0.312058386067501,-7.90484285509111,
127.129926939585));
#55355=CARTESIAN_POINT('Ctrl Pts',(-0.508160110409938,-7.89710137449179,
127.122015201775));
#55356=CARTESIAN_POINT('Ctrl Pts',(-0.703781536764284,-7.88206590697657,
127.114103463965));
#55357=CARTESIAN_POINT('Ctrl Pts',(-0.89834741166975,-7.85982779251214,
127.106191726155));
#55358=CARTESIAN_POINT('Ctrl Pts',(-0.978832218720607,-7.85062869553424,
127.102918928747));
#55359=CARTESIAN_POINT('Ctrl Pts',(-1.05913653073782,-7.84019770321675,
127.099646131339));
#55360=CARTESIAN_POINT('Ctrl Pts',(-1.13922025614804,-7.82854381146213,
127.096373333932));
#55361=CARTESIAN_POINT('Ctrl Pts',(-1.34268065491317,-7.79893597976579,
127.08805847767));
#55362=CARTESIAN_POINT('Ctrl Pts',(-1.54516044360248,-7.76136674831017,
127.079743621408));
#55363=CARTESIAN_POINT('Ctrl Pts',(-1.74602739208576,-7.71591273577444,
127.071428765146));
#55364=CARTESIAN_POINT('Ctrl Pts',(-1.94664697990449,-7.67051469827508,
127.063124148341));
#55365=CARTESIAN_POINT('Ctrl Pts',(-2.14565740416364,-7.61725130988443,
127.054819531536));
#55366=CARTESIAN_POINT('Ctrl Pts',(-2.34243424426202,-7.55625057891205,
127.04651491473));
#55367=CARTESIAN_POINT('Ctrl Pts',(-2.5389817401369,-7.49532094454468,127.03821997699));
#55368=CARTESIAN_POINT('Ctrl Pts',(-2.73330056505798,-7.42667204064051,
127.029925039251));
#55369=CARTESIAN_POINT('Ctrl Pts',(-2.924778318474,-7.35048248673408,127.021630101511));
#55370=CARTESIAN_POINT('Ctrl Pts',(-3.11596908234092,-7.27440712680231,
127.01334759634));
#55371=CARTESIAN_POINT('Ctrl Pts',(-3.30432700101088,-7.19081377987862,
127.005065091169));
#55372=CARTESIAN_POINT('Ctrl Pts',(-3.48925653830335,-7.0999302679609,126.996782585999));
#55373=CARTESIAN_POINT('Ctrl Pts',(-3.67401619147872,-7.00913024549223,
126.988507689489));
#55374=CARTESIAN_POINT('Ctrl Pts',(-3.85535348153576,-6.91105354190999,
126.980232792979));
#55375=CARTESIAN_POINT('Ctrl Pts',(-4.03269282144953,-6.80597602169075,
126.971957896468));
#55376=CARTESIAN_POINT('Ctrl Pts',(-4.20982930841732,-6.70101869637324,
126.963692465355));
#55377=CARTESIAN_POINT('Ctrl Pts',(-4.38297671897432,-6.5890766830643,126.955427034241));
#55378=CARTESIAN_POINT('Ctrl Pts',(-4.55158379852518,-6.47047184716873,
126.947161603127));
#55379=CARTESIAN_POINT('Ctrl Pts',(-4.6174716881255,-6.42412372018398,126.943931656827));
#55380=CARTESIAN_POINT('Ctrl Pts',(-4.68266649919513,-6.37675862865773,
126.940701710528));
#55381=CARTESIAN_POINT('Ctrl Pts',(-4.74713639940072,-6.32839766492947,
126.937471764228));
#55382=CARTESIAN_POINT('Ctrl Pts',(-4.91213757985737,-6.20462492636871,
126.929205194083));
#55383=CARTESIAN_POINT('Ctrl Pts',(-5.07220235932771,-6.07446541213496,
126.920938623938));
#55384=CARTESIAN_POINT('Ctrl Pts',(-5.22685289177513,-5.93834403245063,
126.912672053793));
#55385=CARTESIAN_POINT('Ctrl Pts',(-5.38164199289033,-5.80210068643394,
126.904398076705));
#55386=CARTESIAN_POINT('Ctrl Pts',(-5.53100694168514,-5.65988500454373,
126.896124099618));
#55387=CARTESIAN_POINT('Ctrl Pts',(-5.67450643526183,-5.51215907936011,
126.88785012253));
#55388=CARTESIAN_POINT('Ctrl Pts',(-5.81814382043432,-5.36429120131619,
126.879568194809));
#55389=CARTESIAN_POINT('Ctrl Pts',(-5.95590429362663,-5.21090271949208,
126.871286267088));
#55390=CARTESIAN_POINT('Ctrl Pts',(-6.08738599883386,-5.05248975270623,
126.863004339367));
#55391=CARTESIAN_POINT('Ctrl Pts',(-6.21908565043997,-4.89381419778622,
126.854708683376));
#55392=CARTESIAN_POINT('Ctrl Pts',(-6.34448553839401,-4.73009773313712,
126.846413027385));
#55393=CARTESIAN_POINT('Ctrl Pts',(-6.46322521665564,-4.561868125975,126.838117371394));
#55394=CARTESIAN_POINT('Ctrl Pts',(-6.58207221260689,-4.39348647180526,
126.829814217735));
#55395=CARTESIAN_POINT('Ctrl Pts',(-6.69424681966151,-4.22058377639063,
126.821511064077));
#55396=CARTESIAN_POINT('Ctrl Pts',(-6.7994332954081,-4.04371461175189,126.813207910418));
#55397=CARTESIAN_POINT('Ctrl Pts',(-6.9047801423241,-3.86657578587996,126.804892097466));
#55398=CARTESIAN_POINT('Ctrl Pts',(-7.00311741704465,-3.68545865853627,
126.796576284514));
#55399=CARTESIAN_POINT('Ctrl Pts',(-7.09417562213484,-3.50094176505519,
126.788260471562));
#55400=CARTESIAN_POINT('Ctrl Pts',(-7.12954515401619,-3.42927028701362,
126.785030379216));
#55401=CARTESIAN_POINT('Ctrl Pts',(-7.16381696594036,-3.35708607204337,
126.78180028687));
#55402=CARTESIAN_POINT('Ctrl Pts',(-7.19697725308157,-3.28442375746895,
126.778570194524));
#55403=CARTESIAN_POINT('Ctrl Pts',(-7.28407650476369,-3.09356795462343,
126.770085990964));
#55404=CARTESIAN_POINT('Ctrl Pts',(-7.36365819743208,-2.89907415392788,
126.761601787403));
#55405=CARTESIAN_POINT('Ctrl Pts',(-7.43542987574275,-2.70153725921229,
126.753117583843));
#55406=CARTESIAN_POINT('Ctrl Pts',(-7.50707789014547,-2.50434072416134,
126.74464799872));
#55407=CARTESIAN_POINT('Ctrl Pts',(-7.57094264450145,-2.30411180287135,
126.736178413597));
#55408=CARTESIAN_POINT('Ctrl Pts',(-7.62677904215236,-2.10146673592174,
126.727708828474));
#55409=CARTESIAN_POINT('Ctrl Pts',(-7.68247546284319,-1.89932968241211,
126.719260475859));
#55410=CARTESIAN_POINT('Ctrl Pts',(-7.73018361712663,-1.69478882443706,
126.710812123245));
#55411=CARTESIAN_POINT('Ctrl Pts',(-7.76970775347896,-1.48847654517262,
126.70236377063));
#55412=CARTESIAN_POINT('Ctrl Pts',(-7.80917011504265,-1.28248672450233,
126.693928622483));
#55413=CARTESIAN_POINT('Ctrl Pts',(-7.84047392002923,-1.07473126313879,
126.685493474337));
#55414=CARTESIAN_POINT('Ctrl Pts',(-7.86347335872907,-0.865856648965776,
126.67705832619));
#55415=CARTESIAN_POINT('Ctrl Pts',(-7.88642176547576,-0.657445493038951,
126.668641894243));
#55416=CARTESIAN_POINT('Ctrl Pts',(-7.9011025401978,-0.447920401316483,
126.660225462296));
#55417=CARTESIAN_POINT('Ctrl Pts',(-7.90742101320104,-0.237936798303012,
126.651809030349));
#55418=CARTESIAN_POINT('Ctrl Pts',(-7.90979270182071,-0.159117798628721,
126.648649856312));
#55419=CARTESIAN_POINT('Ctrl Pts',(-7.9109867088849,-0.0802343115594641,
126.645490682274));
#55420=CARTESIAN_POINT('Ctrl Pts',(-7.91099988964655,-0.00132136755638792,
126.642331508237));
#55421=CARTESIAN_POINT('',(-7.91057951044591,-1.0961900785361E-6,124.642534073604));
#55422=CARTESIAN_POINT('Ctrl Pts',(-7.89590378815153,-0.000272972207095395,
126.642289558051));
#55423=CARTESIAN_POINT('Ctrl Pts',(-7.89525879231852,0.244182270797831,
126.632484421598));
#55424=CARTESIAN_POINT('Ctrl Pts',(-7.88346689406167,0.489073252446727,
126.622890110621));
#55425=CARTESIAN_POINT('Ctrl Pts',(-7.86064702013486,0.733159060168601,
126.613430455262));
#55426=CARTESIAN_POINT('Ctrl Pts',(-7.83768760356675,0.978737443108859,
126.603912954478));
#55427=CARTESIAN_POINT('Ctrl Pts',(-7.8035656702398,1.22350018880843,126.594531761177));
#55428=CARTESIAN_POINT('Ctrl Pts',(-7.75843803336029,1.46622231357713,126.58520929961));
#55429=CARTESIAN_POINT('Ctrl Pts',(-7.71215904724558,1.71513705005877,126.575648992464));
#55430=CARTESIAN_POINT('Ctrl Pts',(-7.65430637076432,1.96190507839382,126.566150452148));
#55431=CARTESIAN_POINT('Ctrl Pts',(-7.58507521641603,2.20525554097891,126.556630012532));
#55432=CARTESIAN_POINT('Ctrl Pts',(-7.517710985487,2.44204368805782,126.547366306057));
#55433=CARTESIAN_POINT('Ctrl Pts',(-7.43957455068223,2.67559611108232,126.538081865451));
#55434=CARTESIAN_POINT('Ctrl Pts',(-7.35085768859411,2.90479295349016,126.528699612255));
#55435=CARTESIAN_POINT('Ctrl Pts',(-7.25845279536768,3.14351769253126,126.518927331265));
#55436=CARTESIAN_POINT('Ctrl Pts',(-7.15457041498237,3.37751673678469,126.509048936354));
#55437=CARTESIAN_POINT('Ctrl Pts',(-7.03942703122764,3.60558499376228,126.498977331278));
#55438=CARTESIAN_POINT('Ctrl Pts',(-6.92428364747292,3.83365325073987,126.488905726203));
#55439=CARTESIAN_POINT('Ctrl Pts',(-6.79788019574378,4.0557908697991,126.478640910961));
#55440=CARTESIAN_POINT('Ctrl Pts',(-6.6604189393482,4.27085362223415,126.46809578931));
#55441=CARTESIAN_POINT('Ctrl Pts',(-6.53065020558335,4.47388116465065,126.458140787297));
#55442=CARTESIAN_POINT('Ctrl Pts',(-6.3910274142673,4.67060441864484,126.447935973715));
#55443=CARTESIAN_POINT('Ctrl Pts',(-6.24257616274397,4.86064634215427,126.437408071393));
#55444=CARTESIAN_POINT('Ctrl Pts',(-6.10913696387804,5.03147037875764,126.427944797509));
#55445=CARTESIAN_POINT('Ctrl Pts',(-5.96856459495533,5.19689684478606,126.418220475277));
#55446=CARTESIAN_POINT('Ctrl Pts',(-5.82157948367676,5.35667837550104,126.408181885613));
#55447=CARTESIAN_POINT('Ctrl Pts',(-5.74017026894573,5.44517501867041,126.402621909541));
#55448=CARTESIAN_POINT('Ctrl Pts',(-5.65669728192142,5.53177480412959,126.397073971827));
#55449=CARTESIAN_POINT('Ctrl Pts',(-5.57106832213004,5.61622362318462,126.391705186412));
#55450=CARTESIAN_POINT('Ctrl Pts',(-5.48571564414274,5.70039996815918,126.386353723381));
#55451=CARTESIAN_POINT('Ctrl Pts',(-5.39822060300345,5.78243891205619,126.381180258445));
#55452=CARTESIAN_POINT('Ctrl Pts',(-5.30852766599007,5.86205167675951,126.37635029318));
#55453=CARTESIAN_POINT('Ctrl Pts',(-5.1012393575636,6.0460438156505,126.365187816368));
#55454=CARTESIAN_POINT('Ctrl Pts',(-4.88405257074258,6.2192397713721,126.354216226508));
#55455=CARTESIAN_POINT('Ctrl Pts',(-4.65847571308924,6.38096910882099,126.343375235685));
#55456=CARTESIAN_POINT('Ctrl Pts',(-4.43090782437457,6.54412593372466,126.332438557965));
#55457=CARTESIAN_POINT('Ctrl Pts',(-4.19480129197745,6.69561356116855,126.321634794895));
#55458=CARTESIAN_POINT('Ctrl Pts',(-3.95165450541081,6.8347617989245,126.310902048054));
#55459=CARTESIAN_POINT('Ctrl Pts',(-3.70677037942015,6.97490428267748,126.300092613282));
#55460=CARTESIAN_POINT('Ctrl Pts',(-3.45474506663523,7.10253126782972,126.289355213218));
#55461=CARTESIAN_POINT('Ctrl Pts',(-3.1970568016103,7.21696440524782,126.278626613105));
#55462=CARTESIAN_POINT('Ctrl Pts',(-2.93964967973582,7.33127269378013,126.267909718113));
#55463=CARTESIAN_POINT('Ctrl Pts',(-2.67659177292291,7.43241685886757,126.25720160388));
#55464=CARTESIAN_POINT('Ctrl Pts',(-2.40930549423133,7.51971345444516,126.246439242392));
#55465=CARTESIAN_POINT('Ctrl Pts',(-2.14547058041334,7.60588282267298,126.235815851137));
#55466=CARTESIAN_POINT('Ctrl Pts',(-1.87751538500848,7.67856087462327,126.22513960453));
#55467=CARTESIAN_POINT('Ctrl Pts',(-1.60676274543931,7.73706912373422,126.214349884736));
#55468=CARTESIAN_POINT('Ctrl Pts',(-1.34509704141678,7.79361373293583,126.203922286945));
#55469=CARTESIAN_POINT('Ctrl Pts',(-1.08081792752042,7.83692446044875,126.193388704872));
#55470=CARTESIAN_POINT('Ctrl Pts',(-0.81508448245884,7.86635676154958,126.182694421459));
#55471=CARTESIAN_POINT('Ctrl Pts',(-0.549351037397265,7.89578906265042,
126.172000138045));
#55472=CARTESIAN_POINT('Ctrl Pts',(-0.282162777800421,7.91134390915374,
126.161145153291));
#55473=CARTESIAN_POINT('Ctrl Pts',(-0.0146508286642535,7.9123310740961,
126.150074750138));
#55474=CARTESIAN_POINT('Ctrl Pts',(0.251092225934842,7.91331171151444,126.139077548857));
#55475=CARTESIAN_POINT('Ctrl Pts',(0.517155297956743,7.89991576666261,126.127867768622));
#55476=CARTESIAN_POINT('Ctrl Pts',(0.782460672384277,7.87279628714158,126.116391770645));
#55477=CARTESIAN_POINT('Ctrl Pts',(1.03037699804824,7.84745431383524,126.105667949999));
#55478=CARTESIAN_POINT('Ctrl Pts',(1.2767839336486,7.8097077836232,126.095037915708));
#55479=CARTESIAN_POINT('Ctrl Pts',(1.52075398454111,7.7602225636823,126.084495441738));
#55480=CARTESIAN_POINT('Ctrl Pts',(1.7767834028631,7.70829130396147,126.073431856398));
#55481=CARTESIAN_POINT('Ctrl Pts',(2.03012966018809,7.64343225965122,126.062464701477));
#55482=CARTESIAN_POINT('Ctrl Pts',(2.2797351064227,7.56635891108657,126.051586781298));
#55483=CARTESIAN_POINT('Ctrl Pts',(2.53575241247222,7.4873057038533,126.040429429318));
#55484=CARTESIAN_POINT('Ctrl Pts',(2.78783504942617,7.39540241387966,126.029365955485));
#55485=CARTESIAN_POINT('Ctrl Pts',(3.03484557046376,7.29136263958527,126.018388595228));
#55486=CARTESIAN_POINT('Ctrl Pts',(3.28564332865553,7.18572769721033,126.00724292689));
#55487=CARTESIAN_POINT('Ctrl Pts',(3.53121315723989,7.06758092367902,125.99618603301));
#55488=CARTESIAN_POINT('Ctrl Pts',(3.77035524889978,6.93761615226074,125.985209786367));
#55489=CARTESIAN_POINT('Ctrl Pts',(4.00938538319851,6.80771222547567,125.974238678391));
#55490=CARTESIAN_POINT('Ctrl Pts',(4.24199470785378,6.66600088648738,125.963348142159));
#55491=CARTESIAN_POINT('Ctrl Pts',(4.46696222334666,6.51312867884672,125.952530061859));
#55492=CARTESIAN_POINT('Ctrl Pts',(4.68565687270186,6.36451907282034,125.942013626752));
#55493=CARTESIAN_POINT('Ctrl Pts',(4.89713060704942,6.20536172926908,125.931565663272));
#55494=CARTESIAN_POINT('Ctrl Pts',(5.10022868738935,6.0362150263091,125.921178715744));
#55495=CARTESIAN_POINT('Ctrl Pts',(5.29824962882789,5.87129673015732,125.911051425891));
#55496=CARTESIAN_POINT('Ctrl Pts',(5.48830900713355,5.6968817792442,125.900982139511));
#55497=CARTESIAN_POINT('Ctrl Pts',(5.66929564701769,5.51346125802735,125.89096394621));
#55498=CARTESIAN_POINT('Ctrl Pts',(5.84313639376888,5.33728272684824,125.881341301105));
#55499=CARTESIAN_POINT('Ctrl Pts',(6.00860702598225,5.15279527887537,125.871765794112));
#55500=CARTESIAN_POINT('Ctrl Pts',(6.16467841740571,4.96041613331724,125.862231301475));
#55501=CARTESIAN_POINT('Ctrl Pts',(6.23236974654909,4.8769773945226,125.858095998564));
#55502=CARTESIAN_POINT('Ctrl Pts',(6.29829234471388,4.79205392592341,125.853968410999));
#55503=CARTESIAN_POINT('Ctrl Pts',(6.36235925507139,4.70567896073921,125.84984803915));
#55504=CARTESIAN_POINT('Ctrl Pts',(6.46054940887198,4.57329906183929,125.843533079628));
#55505=CARTESIAN_POINT('Ctrl Pts',(6.55444152696451,4.43787560876014,125.837090858175));
#55506=CARTESIAN_POINT('Ctrl Pts',(6.64372079618492,4.29954037237058,125.830546692025));
#55507=CARTESIAN_POINT('Ctrl Pts',(6.78171323046985,4.08572571882934,125.820431853215));
#55508=CARTESIAN_POINT('Ctrl Pts',(6.90868661329275,3.86495256094039,125.81007347237));
#55509=CARTESIAN_POINT('Ctrl Pts',(7.02445911752514,3.63839446700022,125.799565031978));
#55510=CARTESIAN_POINT('Ctrl Pts',(7.14067492739179,3.41096885723494,125.789016353614));
#55511=CARTESIAN_POINT('Ctrl Pts',(7.24560298045697,3.17771376223105,125.778316464314));
#55512=CARTESIAN_POINT('Ctrl Pts',(7.33904695897157,2.9398675721495,125.767559924547));
#55513=CARTESIAN_POINT('Ctrl Pts',(7.43277384202596,2.70130129535914,125.756770819024));
#55514=CARTESIAN_POINT('Ctrl Pts',(7.51494603697236,2.45811614005707,125.745924719492));
#55515=CARTESIAN_POINT('Ctrl Pts',(7.58536736127838,2.21161406445729,125.73511704788));
#55516=CARTESIAN_POINT('Ctrl Pts',(7.63190133520942,2.04872702316763,125.727975405572));
#55517=CARTESIAN_POINT('Ctrl Pts',(7.67330437430786,1.88439274736401,125.720850542754));
#55518=CARTESIAN_POINT('Ctrl Pts',(7.70952348573126,1.71899887370687,125.713769991952));
#55519=CARTESIAN_POINT('Ctrl Pts',(7.7592398181954,1.49197020052525,125.704050840823));
#55520=CARTESIAN_POINT('Ctrl Pts',(7.7991789160809,1.26291754830903,125.694426102973));
#55521=CARTESIAN_POINT('Ctrl Pts',(7.82932224132061,1.03264414334578,125.684900439759));
#55522=CARTESIAN_POINT('Ctrl Pts',(7.85973059201407,0.800346133825817,125.675291025228));
#55523=CARTESIAN_POINT('Ctrl Pts',(7.88017019939908,0.566804925514715,125.665782435155));
#55524=CARTESIAN_POINT('Ctrl Pts',(7.89056995547163,0.332838287613528,125.656379454933));
#55525=CARTESIAN_POINT('Ctrl Pts',(7.90088891275422,0.10068940592751,125.647049529254));
#55526=CARTESIAN_POINT('Ctrl Pts',(7.90132332167632,-0.131879176590046,
125.637823578772));
#55527=CARTESIAN_POINT('Ctrl Pts',(7.89175331818299,-0.364062246507516,
125.628706278206));
#55528=CARTESIAN_POINT('Ctrl Pts',(7.88242822988306,-0.590303295451428,
125.619822307277));
#55529=CARTESIAN_POINT('Ctrl Pts',(7.86360401924518,-0.816179005692197,
125.611041496294));
#55530=CARTESIAN_POINT('Ctrl Pts',(7.83512431819111,-1.04092707177344,125.602368170178));
#55531=CARTESIAN_POINT('Ctrl Pts',(7.81326926485723,-1.21339661285348,125.595712341716));
#55532=CARTESIAN_POINT('Ctrl Pts',(7.78572729891087,-1.3852018418126,125.58911980983));
#55533=CARTESIAN_POINT('Ctrl Pts',(7.75240995369105,-1.55598728154999,125.582592528981));
#55534=CARTESIAN_POINT('Ctrl Pts',(7.704696574801,-1.80056710450204,125.573244886719));
#55535=CARTESIAN_POINT('Ctrl Pts',(7.64563886056102,-2.04301353573977,125.563753397419));
#55536=CARTESIAN_POINT('Ctrl Pts',(7.5750843874418,-2.28203217332167,125.554127720513));
#55537=CARTESIAN_POINT('Ctrl Pts',(7.50559804389413,-2.5174322894454,125.544647767467));
#55538=CARTESIAN_POINT('Ctrl Pts',(7.42496042501464,-2.74950672460934,125.535037659012));
#55539=CARTESIAN_POINT('Ctrl Pts',(7.33307592637004,-2.97702152106806,125.525306622484));
#55540=CARTESIAN_POINT('Ctrl Pts',(7.29528362711784,-3.07059886435126,125.521304225453));
#55541=CARTESIAN_POINT('Ctrl Pts',(7.25558928898099,-3.16340496065179,125.517281371078));
#55542=CARTESIAN_POINT('Ctrl Pts',(7.21398876103173,-3.2553546114445,125.513238701394));
#55543=CARTESIAN_POINT('Ctrl Pts',(7.11242351002883,-3.479844295176,125.503368760279));
#55544=CARTESIAN_POINT('Ctrl Pts',(6.99949282415126,-3.69922720361958,125.493380707321));
#55545=CARTESIAN_POINT('Ctrl Pts',(6.87617750823767,-3.91272100540851,125.483283885776));
#55546=CARTESIAN_POINT('Ctrl Pts',(6.75156946206384,-4.128452890082,125.473081217957));
#55547=CARTESIAN_POINT('Ctrl Pts',(6.61635857760223,-4.33817092337202,125.462767489129));
#55548=CARTESIAN_POINT('Ctrl Pts',(6.47160077363162,-4.54109904828406,125.45235233948));
#55549=CARTESIAN_POINT('Ctrl Pts',(6.32732674454847,-4.74334899538394,125.441971996852));
#55550=CARTESIAN_POINT('Ctrl Pts',(6.17357025888858,-4.93885379496384,125.43149091016));
#55551=CARTESIAN_POINT('Ctrl Pts',(6.01140929001699,-5.12688461360331,125.420918623264));
#55552=CARTESIAN_POINT('Ctrl Pts',(5.88420144238739,-5.27438617266281,125.412625148763));
#55553=CARTESIAN_POINT('Ctrl Pts',(5.75182250090869,-5.41728916979181,125.404275552543));
#55554=CARTESIAN_POINT('Ctrl Pts',(5.61480240349224,-5.55526214589234,125.395874441697));
#55555=CARTESIAN_POINT('Ctrl Pts',(5.47545207294324,-5.69558156026265,125.387330457307));
#55556=CARTESIAN_POINT('Ctrl Pts',(5.3309152373884,-5.83058168527743,125.378979025504));
#55557=CARTESIAN_POINT('Ctrl Pts',(5.18166485115756,-5.96008197030643,125.370759811148));
#55558=CARTESIAN_POINT('Ctrl Pts',(5.0313840659925,-6.0904763029761,125.362483852754));
#55559=CARTESIAN_POINT('Ctrl Pts',(4.87632421001643,-6.21529523085981,125.354341943722));
#55560=CARTESIAN_POINT('Ctrl Pts',(4.71691597298543,-6.33434478870322,125.346272490636));
#55561=CARTESIAN_POINT('Ctrl Pts',(4.55734288271084,-6.45351746255446,125.338194692463));
#55562=CARTESIAN_POINT('Ctrl Pts',(4.39341211775056,-6.56690949397952,125.330189500176));
#55563=CARTESIAN_POINT('Ctrl Pts',(4.22550754581221,-6.67430688684188,125.322195129067));
#55564=CARTESIAN_POINT('Ctrl Pts',(4.16655942901025,-6.7120120784611,125.319388456703));
#55565=CARTESIAN_POINT('Ctrl Pts',(4.10712109687097,-6.74897816105583,125.316583118135));
#55566=CARTESIAN_POINT('Ctrl Pts',(4.04720786296046,-6.78519506688655,125.313776439721));
#55567=CARTESIAN_POINT('Ctrl Pts',(3.87147408838441,-6.89142424447699,125.305544065011));
#55568=CARTESIAN_POINT('Ctrl Pts',(3.69128912667578,-6.99090306358223,125.297551796561));
#55569=CARTESIAN_POINT('Ctrl Pts',(3.50736398910526,-7.08321704061147,125.289710530334));
#55570=CARTESIAN_POINT('Ctrl Pts',(3.32364035610237,-7.1754298803613,125.281877854836));
#55571=CARTESIAN_POINT('Ctrl Pts',(3.13618541275297,-7.26049381834744,125.274195850871));
#55572=CARTESIAN_POINT('Ctrl Pts',(2.94569003733961,-7.33804445665589,125.266575706942));
#55573=CARTESIAN_POINT('Ctrl Pts',(2.75565232501483,-7.4154087803907,125.258973870327));
#55574=CARTESIAN_POINT('Ctrl Pts',(2.56258934948931,-7.48529620126047,125.251433596868));
#55575=CARTESIAN_POINT('Ctrl Pts',(2.36715993274988,-7.54738903389064,125.243866713637));
#55576=CARTESIAN_POINT('Ctrl Pts',(2.17117638430508,-7.60965792807701,125.236278374834));
#55577=CARTESIAN_POINT('Ctrl Pts',(1.97281347304944,-7.66408835342329,125.228663275142));
#55578=CARTESIAN_POINT('Ctrl Pts',(1.77270010343906,-7.71039893332288,125.220932489474));
#55579=CARTESIAN_POINT('Ctrl Pts',(1.57258673382868,-7.75670951322246,125.213201703805));
#55580=CARTESIAN_POINT('Ctrl Pts',(1.37072331133005,-7.79490072675831,125.20535523216));
#55581=CARTESIAN_POINT('Ctrl Pts',(1.16769634284776,-7.82472364305471,125.197304149447));
#55582=CARTESIAN_POINT('Ctrl Pts',(0.965813858357259,-7.85437844449156,
125.18929845152));
#55583=CARTESIAN_POINT('Ctrl Pts',(0.762781187986504,-7.87575977590004,
125.181090442852));
#55584=CARTESIAN_POINT('Ctrl Pts',(0.559208285894424,-7.88926781703919,
125.172592693732));
#55585=CARTESIAN_POINT('Ctrl Pts',(0.356459147674568,-7.90272119748351,
125.164129331009));
#55586=CARTESIAN_POINT('Ctrl Pts',(0.15317432145551,-7.90836561736718,125.155378567978));
#55587=CARTESIAN_POINT('Ctrl Pts',(-0.0500937518569253,-7.90660820598672,
125.146254031998));
#55588=CARTESIAN_POINT('Ctrl Pts',(-0.149919802184598,-7.90574513175153,
125.141772923022));
#55589=CARTESIAN_POINT('Ctrl Pts',(-0.249742595932376,-7.90309696089872,
125.137201665795));
#55590=CARTESIAN_POINT('Ctrl Pts',(-0.349501308744162,-7.89871215899861,
125.132530029736));
#55591=CARTESIAN_POINT('Ctrl Pts',(-0.536340080188239,-7.8904998337094,
125.123780490801));
#55592=CARTESIAN_POINT('Ctrl Pts',(-0.722728550015766,-7.87503750680139,
125.11536121481));
#55593=CARTESIAN_POINT('Ctrl Pts',(-0.90822169714376,-7.85269664800584,
125.107185686861));
#55594=CARTESIAN_POINT('Ctrl Pts',(-1.09477681054902,-7.83022788562456,
125.09896335322));
#55595=CARTESIAN_POINT('Ctrl Pts',(-1.2804265969939,-7.80080201738374,125.090987566571));
#55596=CARTESIAN_POINT('Ctrl Pts',(-1.46476571484636,-7.76477314121034,
125.083170317571));
#55597=CARTESIAN_POINT('Ctrl Pts',(-1.65058136729158,-7.72845567798809,
125.075290453328));
#55598=CARTESIAN_POINT('Ctrl Pts',(-1.83506559767051,-7.68542941634956,
125.06757167664));
#55599=CARTESIAN_POINT('Ctrl Pts',(-2.01784670126836,-7.63602668685808,
125.059923846344));
#55600=CARTESIAN_POINT('Ctrl Pts',(-2.11626352911673,-7.60942623512704,
125.055805941469));
#55601=CARTESIAN_POINT('Ctrl Pts',(-2.21418730376919,-7.58097656982377,
125.051708605274));
#55602=CARTESIAN_POINT('Ctrl Pts',(-2.31156460429401,-7.55072534553676,
125.04761776636));
#55603=CARTESIAN_POINT('Ctrl Pts',(-2.54981033105506,-7.47671194737491,
125.037609018068));
#55604=CARTESIAN_POINT('Ctrl Pts',(-2.78498729435328,-7.3914957108001,125.02782080113));
#55605=CARTESIAN_POINT('Ctrl Pts',(-3.01591873950803,-7.29560419056322,
125.018171102507));
#55606=CARTESIAN_POINT('Ctrl Pts',(-3.24777425835197,-7.19932895978053,
125.008482790551));
#55607=CARTESIAN_POINT('Ctrl Pts',(-3.47535007178051,-7.09229375475358,
124.998934107693));
#55608=CARTESIAN_POINT('Ctrl Pts',(-3.69750661335462,-6.97504307815172,
124.98944205242));
#55609=CARTESIAN_POINT('Ctrl Pts',(-3.91984755346553,-6.85769507894549,
124.979942118374));
#55610=CARTESIAN_POINT('Ctrl Pts',(-4.13676027527797,-6.73011552110335,
124.970498905959));
#55611=CARTESIAN_POINT('Ctrl Pts',(-4.34715435964132,-6.59284735276243,
124.961029206809));
#55612=CARTESIAN_POINT('Ctrl Pts',(-4.55706810742043,-6.45589257214487,
124.951581127293));
#55613=CARTESIAN_POINT('Ctrl Pts',(-4.76049319839731,-6.3092941786778,124.942106681844));
#55614=CARTESIAN_POINT('Ctrl Pts',(-4.95639607436519,-6.15357587240645,
124.9325232307));
#55615=CARTESIAN_POINT('Ctrl Pts',(-5.15135536486482,-5.99860759867143,
124.92298593919));
#55616=CARTESIAN_POINT('Ctrl Pts',(-5.33886515785193,-5.8346077715742,124.913340689529));
#55617=CARTESIAN_POINT('Ctrl Pts',(-5.51795063617884,-5.6620657728485,124.903506030338));
#55618=CARTESIAN_POINT('Ctrl Pts',(-5.6654274504436,-5.51997751121685,124.895407192731));
#55619=CARTESIAN_POINT('Ctrl Pts',(-5.8071922583387,-5.37209604074902,124.887179906759));
#55620=CARTESIAN_POINT('Ctrl Pts',(-5.94271957325834,-5.21867595122357,
124.878778685289));
#55621=CARTESIAN_POINT('Ctrl Pts',(-6.10495330646991,-5.03502357171522,
124.868721955962));
#55622=CARTESIAN_POINT('Ctrl Pts',(-6.25824881491363,-4.8434361227992,124.858415987131));
#55623=CARTESIAN_POINT('Ctrl Pts',(-6.40246678594291,-4.64499312136272,
124.847782754194));
#55624=CARTESIAN_POINT('Ctrl Pts',(-6.48344627840437,-4.53356586008476,
124.84181211267));
#55625=CARTESIAN_POINT('Ctrl Pts',(-6.56156416342577,-4.41997629990883,
124.835738287774));
#55626=CARTESIAN_POINT('Ctrl Pts',(-6.63679849650785,-4.30440884672953,
124.829547466172));
#55627=CARTESIAN_POINT('Ctrl Pts',(-6.72011499660551,-4.17642637742798,
124.822691585786));
#55628=CARTESIAN_POINT('Ctrl Pts',(-6.79965595586647,-4.04601823311049,
124.815814270083));
#55629=CARTESIAN_POINT('Ctrl Pts',(-6.87518476737688,-3.91329963578802,
124.809047070757));
#55630=CARTESIAN_POINT('Ctrl Pts',(-6.95065926439568,-3.78067647943699,
124.80228473788));
#55631=CARTESIAN_POINT('Ctrl Pts',(-7.02212695112648,-3.64574585579345,
124.795632363062));
#55632=CARTESIAN_POINT('Ctrl Pts',(-7.08931967748596,-3.50866362545707,
124.789221214395));
#55633=CARTESIAN_POINT('Ctrl Pts',(-7.11346374519179,-3.45940646877021,
124.786917524459));
#55634=CARTESIAN_POINT('Ctrl Pts',(-7.13705558281161,-3.40987191498426,
124.784644980414));
#55635=CARTESIAN_POINT('Ctrl Pts',(-7.16008190363514,-3.36006860698215,
124.782409672347));
#55636=CARTESIAN_POINT('Ctrl Pts',(-7.26384175661325,-3.13564786883096,
124.772337058573));
#55637=CARTESIAN_POINT('Ctrl Pts',(-7.35716995380072,-2.90649307648692,
124.762305051782));
#55638=CARTESIAN_POINT('Ctrl Pts',(-7.4398793877542,-2.67359956042123,124.752302142289));
#55639=CARTESIAN_POINT('Ctrl Pts',(-7.52394297711727,-2.43689300877343,
124.742135460741));
#55640=CARTESIAN_POINT('Ctrl Pts',(-7.59703764473626,-2.19632357951533,
124.731998837077));
#55641=CARTESIAN_POINT('Ctrl Pts',(-7.65892336395348,-1.95290543871292,
124.72188018698));
#55642=CARTESIAN_POINT('Ctrl Pts',(-7.67718095646074,-1.88109195282541,
124.718894971771));
#55643=CARTESIAN_POINT('Ctrl Pts',(-7.69446264413822,-1.80903036140325,
124.715911320936));
#55644=CARTESIAN_POINT('Ctrl Pts',(-7.7107614762586,-1.73674635135296,124.712928924174));
#55645=CARTESIAN_POINT('Ctrl Pts',(-7.76604171847109,-1.49158292159577,
124.702813621792));
#55646=CARTESIAN_POINT('Ctrl Pts',(-7.81001965507663,-1.24386161844227,
124.692712745543));
#55647=CARTESIAN_POINT('Ctrl Pts',(-7.84250939741529,-0.994603241615372,
124.682614188839));
#55648=CARTESIAN_POINT('Ctrl Pts',(-7.87446930152253,-0.749409735976667,
124.672680318004));
#55649=CARTESIAN_POINT('Ctrl Pts',(-7.89531272647988,-0.502728051252808,
124.662748691678));
#55650=CARTESIAN_POINT('Ctrl Pts',(-7.9048127147597,-0.255527884110175,
124.652807785965));
#55651=CARTESIAN_POINT('Ctrl Pts',(-7.90808419112052,-0.170400462962063,
124.649384472473));
#55652=CARTESIAN_POINT('Ctrl Pts',(-7.91001002324155,-0.0852115949657462,
124.645960058556));
#55653=CARTESIAN_POINT('Ctrl Pts',(-7.91057951044591,-1.09619007819858E-6,
124.642534073604));
#55654=CARTESIAN_POINT('',(-7.911,6.17617068598975E-12,120.642331508237));
#55655=CARTESIAN_POINT('Ctrl Pts',(-7.91099999999379,-9.9090788532874E-6,
124.642291611247));
#55656=CARTESIAN_POINT('Ctrl Pts',(-7.91100077170824,0.616095093624387,
124.619899103357));
#55657=CARTESIAN_POINT('Ctrl Pts',(-7.83902979552628,1.23004343623821,124.598290807754));
#55658=CARTESIAN_POINT('Ctrl Pts',(-7.69060049730395,1.85452253341298,124.572895390152));
#55659=CARTESIAN_POINT('Ctrl Pts',(-7.68449683023176,1.8796537662833,124.571867207376));
#55660=CARTESIAN_POINT('Ctrl Pts',(-7.67537217560989,1.91643623128281,124.570352751203));
#55661=CARTESIAN_POINT('Ctrl Pts',(-7.67244761460173,1.92811137169331,124.569870627421));
#55662=CARTESIAN_POINT('Ctrl Pts',(-7.66712052415858,1.94917360889316,124.568998235471));
#55663=CARTESIAN_POINT('Ctrl Pts',(-7.66472736624521,1.95856306753437,124.568608382226));
#55664=CARTESIAN_POINT('Ctrl Pts',(-7.66102280173064,1.97298699868632,124.568008014787));
#55665=CARTESIAN_POINT('Ctrl Pts',(-7.65972366394776,1.97802463518305,124.567798055208));
#55666=CARTESIAN_POINT('Ctrl Pts',(-7.65734992081426,1.98719183732612,124.567415471357));
#55667=CARTESIAN_POINT('Ctrl Pts',(-7.65627694102972,1.99132182488932,124.567242921453));
#55668=CARTESIAN_POINT('Ctrl Pts',(-7.65393547617231,2.00030444776745,124.566867214661));
#55669=CARTESIAN_POINT('Ctrl Pts',(-7.65266571716323,2.00515674657815,124.566663999038));
#55670=CARTESIAN_POINT('Ctrl Pts',(-7.64920601422565,2.01832661625434,124.56611171833));
#55671=CARTESIAN_POINT('Ctrl Pts',(-7.64700712327769,2.02664181186375,124.565762235964));
#55672=CARTESIAN_POINT('Ctrl Pts',(-7.63657216286874,2.06584326514629,124.564110865558));
#55673=CARTESIAN_POINT('Ctrl Pts',(-7.6281625923931,2.09668266809594,124.562800737611));
#55674=CARTESIAN_POINT('Ctrl Pts',(-7.48845729261123,2.59703936891187,124.541354085422));
#55675=CARTESIAN_POINT('Ctrl Pts',(-7.31423891381664,3.05342230686368,124.518990924046));
#55676=CARTESIAN_POINT('Ctrl Pts',(-7.06745681925023,3.55529748413452,124.493215560518));
#55677=CARTESIAN_POINT('Ctrl Pts',(-7.03486673291457,3.61935576461539,124.489901059271));
#55678=CARTESIAN_POINT('Ctrl Pts',(-6.95920363056495,3.76319336261129,124.482412807041));
#55679=CARTESIAN_POINT('Ctrl Pts',(-6.91562269220845,3.84269468159141,124.478241508865));
#55680=CARTESIAN_POINT('Ctrl Pts',(-6.78625666644176,4.06935516682283,124.466277698181));
#55681=CARTESIAN_POINT('Ctrl Pts',(-6.69707152517261,4.21451856458861,124.458528238528));
#55682=CARTESIAN_POINT('Ctrl Pts',(-6.37126356878239,4.70833282361316,124.431997655447));
#55683=CARTESIAN_POINT('Ctrl Pts',(-6.11152425154984,5.04090670998819,124.413872811678));
#55684=CARTESIAN_POINT('Ctrl Pts',(-5.81428038503819,5.36454946432255,124.39611853848));
#55685=CARTESIAN_POINT('Ctrl Pts',(-5.8020149435884,5.37781274786763,124.395390625951));
#55686=CARTESIAN_POINT('Ctrl Pts',(-5.7841947673019,5.39695073677408,124.394339813085));
#55687=CARTESIAN_POINT('Ctrl Pts',(-5.77867633361254,5.40285907581428,124.394015335394));
#55688=CARTESIAN_POINT('Ctrl Pts',(-5.76903586370807,5.41314902737378,124.393450105277));
#55689=CARTESIAN_POINT('Ctrl Pts',(-5.76491787374394,5.41753441138149,124.393209176539));
#55690=CARTESIAN_POINT('Ctrl Pts',(-5.75695672290038,5.42599314896151,124.392744386498));
#55691=CARTESIAN_POINT('Ctrl Pts',(-5.75311423215649,5.43006712609012,124.392520496135));
#55692=CARTESIAN_POINT('Ctrl Pts',(-5.74400106406117,5.43970877482316,124.391990546226));
#55693=CARTESIAN_POINT('Ctrl Pts',(-5.7387266078904,5.44527287646475,124.391684652842));
#55694=CARTESIAN_POINT('Ctrl Pts',(-5.72020758113734,5.46475207823111,124.390613528363));
#55695=CARTESIAN_POINT('Ctrl Pts',(-5.70692037056824,5.47862664712957,124.389850177573));
#55696=CARTESIAN_POINT('Ctrl Pts',(-5.5453225682028,5.64614205297307,124.380628484054));
#55697=CARTESIAN_POINT('Ctrl Pts',(-5.39089492648068,5.79377104313747,124.372450516427));
#55698=CARTESIAN_POINT('Ctrl Pts',(-4.87541783818458,6.24807648957828,124.346929873478));
#55699=CARTESIAN_POINT('Ctrl Pts',(-4.49275309126979,6.52865706021101,124.330663986209));
#55700=CARTESIAN_POINT('Ctrl Pts',(-3.98659592446996,6.83409126212303,124.31058699436));
#55701=CARTESIAN_POINT('Ctrl Pts',(-3.88456682397703,6.89259682255909,124.306602508755));
#55702=CARTESIAN_POINT('Ctrl Pts',(-3.68721300581236,6.9999891420614,124.298958209091));
#55703=CARTESIAN_POINT('Ctrl Pts',(-3.59212552978188,7.04925680904181,124.295301980547));
#55704=CARTESIAN_POINT('Ctrl Pts',(-3.25682776757225,7.21443835311452,124.282419437024));
#55705=CARTESIAN_POINT('Ctrl Pts',(-3.01179252639721,7.32011873371692,124.273025544921));
#55706=CARTESIAN_POINT('Ctrl Pts',(-2.63708880669378,7.45972017139538,124.258085556628));
#55707=CARTESIAN_POINT('Ctrl Pts',(-2.51112437378818,7.50306026981479,124.252968597139));
#55708=CARTESIAN_POINT('Ctrl Pts',(-2.36427861709037,7.54947290627293,124.246833707374));
#55709=CARTESIAN_POINT('Ctrl Pts',(-2.34440048449791,7.55566945375918,124.245999684416));
#55710=CARTESIAN_POINT('Ctrl Pts',(-2.31884807796263,7.56352427993053,124.244922762561));
#55711=CARTESIAN_POINT('Ctrl Pts',(-2.31319592572444,7.56525482390469,124.244684246638));
#55712=CARTESIAN_POINT('Ctrl Pts',(-2.30409854152164,7.56802906111833,124.244299850877));
#55713=CARTESIAN_POINT('Ctrl Pts',(-2.30065451735323,7.56907674361673,124.244154215097));
#55714=CARTESIAN_POINT('Ctrl Pts',(-2.29407626692484,7.57107296257164,124.243875824814));
#55715=CARTESIAN_POINT('Ctrl Pts',(-2.29094217432202,7.57202190150692,124.243743095974));
#55716=CARTESIAN_POINT('Ctrl Pts',(-2.28375498802345,7.57419316339067,124.24343850323));
#55717=CARTESIAN_POINT('Ctrl Pts',(-2.27970150359107,7.57541417851784,124.243266559717));
#55718=CARTESIAN_POINT('Ctrl Pts',(-2.2691112945865,7.57859495568256,124.242816930959));
#55719=CARTESIAN_POINT('Ctrl Pts',(-2.26257302429417,7.58054951033666,124.242538931718));
#55720=CARTESIAN_POINT('Ctrl Pts',(-2.22148671867581,7.59277398570733,124.240789496881));
#55721=CARTESIAN_POINT('Ctrl Pts',(-2.1868718733217,7.6028160157105,124.239304536962));
#55722=CARTESIAN_POINT('Ctrl Pts',(-1.61369271236818,7.76486145960954,124.214548021526));
#55723=CARTESIAN_POINT('Ctrl Pts',(-1.06059668918216,7.85952508999731,124.18833111026));
#55724=CARTESIAN_POINT('Ctrl Pts',(-0.203109163965433,7.91406844103551,
124.148570421414));
#55725=CARTESIAN_POINT('Ctrl Pts',(0.0968240754261465,7.91608321280031,
124.134803966405));
#55726=CARTESIAN_POINT('Ctrl Pts',(0.444946279826982,7.89862835436435,124.119259843359));
#55727=CARTESIAN_POINT('Ctrl Pts',(0.493709201092214,7.89573039008704,124.117092089108));
#55728=CARTESIAN_POINT('Ctrl Pts',(0.605850564029667,7.88802292399882,124.112130231664));
#55729=CARTESIAN_POINT('Ctrl Pts',(0.669204500677268,7.88290086957189,124.109344270367));
#55730=CARTESIAN_POINT('Ctrl Pts',(0.999083139047645,7.85222515977152,124.094932921075));
#55731=CARTESIAN_POINT('Ctrl Pts',(1.26425908898607,7.81391547534457,124.083680554268));
#55732=CARTESIAN_POINT('Ctrl Pts',(1.54519317138068,7.75864954809616,124.072119948267));
#55733=CARTESIAN_POINT('Ctrl Pts',(1.56337236757229,7.75500687257187,124.071373449657));
#55734=CARTESIAN_POINT('Ctrl Pts',(1.58950608629844,7.74967467213716,124.070302567913));
#55735=CARTESIAN_POINT('Ctrl Pts',(1.59747100329485,7.74803675239752,124.069976491257));
#55736=CARTESIAN_POINT('Ctrl Pts',(1.61129472320905,7.74517179575376,124.069411081564));
#55737=CARTESIAN_POINT('Ctrl Pts',(1.61715467749298,7.7439503859496,124.069171563865));
#55738=CARTESIAN_POINT('Ctrl Pts',(1.62842222555588,7.74158850610722,124.068711329701));
#55739=CARTESIAN_POINT('Ctrl Pts',(1.63383001993956,7.74044901854383,124.068490581123));
#55740=CARTESIAN_POINT('Ctrl Pts',(1.64656966863446,7.73775067524648,124.067970867144));
#55741=CARTESIAN_POINT('Ctrl Pts',(1.6539005166104,7.73618706259885,124.067672058329));
#55742=CARTESIAN_POINT('Ctrl Pts',(1.67924594526784,7.7307434076153,124.066639837052));
#55743=CARTESIAN_POINT('Ctrl Pts',(1.6972492490136,7.72681082801006,124.065908153714));
#55744=CARTESIAN_POINT('Ctrl Pts',(1.8982753896191,7.68216288477946,124.057754864898));
#55745=CARTESIAN_POINT('Ctrl Pts',(2.07981512192932,7.63501479599362,124.050549286224));
#55746=CARTESIAN_POINT('Ctrl Pts',(2.65554284825593,7.46342956325596,124.028075424218));
#55747=CARTESIAN_POINT('Ctrl Pts',(3.04172714893981,7.31454807896272,124.013616363521));
#55748=CARTESIAN_POINT('Ctrl Pts',(3.70556229176986,6.99691531539792,123.988336358649));
#55749=CARTESIAN_POINT('Ctrl Pts',(3.98780137093101,6.83998888561804,123.977422504333));
#55750=CARTESIAN_POINT('Ctrl Pts',(4.48204975463995,6.52417039791635,123.956850845358));
#55751=CARTESIAN_POINT('Ctrl Pts',(4.69717222860623,6.37103794993058,123.947333995196));
#55752=CARTESIAN_POINT('Ctrl Pts',(4.9488906743264,6.1721667442069,123.934992719629));
#55753=CARTESIAN_POINT('Ctrl Pts',(4.99317280140977,6.13639848137497,123.9327735766));
#55754=CARTESIAN_POINT('Ctrl Pts',(5.0607393016651,6.08060699341461,123.929306321449));
#55755=CARTESIAN_POINT('Ctrl Pts',(5.08430017988199,6.0609203360521,123.928081773871));
#55756=CARTESIAN_POINT('Ctrl Pts',(5.11293829151014,6.03670682308196,123.926573502344));
#55757=CARTESIAN_POINT('Ctrl Pts',(5.11812535075823,6.0323096849034,123.926299516304));
#55758=CARTESIAN_POINT('Ctrl Pts',(5.12625974439981,6.02539600793448,123.925868581109));
#55759=CARTESIAN_POINT('Ctrl Pts',(5.12921088905831,6.02288399979204,123.925711976545));
#55760=CARTESIAN_POINT('Ctrl Pts',(5.13445529031209,6.01841332638514,123.92543321453));
#55761=CARTESIAN_POINT('Ctrl Pts',(5.13674927696884,6.01645551474748,123.925311121298));
#55762=CARTESIAN_POINT('Ctrl Pts',(5.14204549564431,6.01193019971306,123.925028875424));
#55763=CARTESIAN_POINT('Ctrl Pts',(5.14504692311312,6.00936176015015,123.924868652703));
#55764=CARTESIAN_POINT('Ctrl Pts',(5.15328495714737,6.00230145439448,123.92442814762));
#55765=CARTESIAN_POINT('Ctrl Pts',(5.15851760302444,5.99780499330445,123.924147523613));
#55766=CARTESIAN_POINT('Ctrl Pts',(5.18589919665489,5.97421339785629,123.922674777655));
#55767=CARTESIAN_POINT('Ctrl Pts',(5.20794776572334,5.95500262204447,123.921474158988));
#55768=CARTESIAN_POINT('Ctrl Pts',(5.23904542034123,5.92760263595197,123.919760500473));
#55769=CARTESIAN_POINT('Ctrl Pts',(5.24818307620973,5.91951385856859,123.919254458469));
#55770=CARTESIAN_POINT('Ctrl Pts',(5.27100527749317,5.89921695402138,123.917984371663));
#55771=CARTESIAN_POINT('Ctrl Pts',(5.28466610461629,5.88698237291208,123.917218525034));
#55772=CARTESIAN_POINT('Ctrl Pts',(5.30010485133022,5.87305845161526,123.916346764332));
#55773=CARTESIAN_POINT('Ctrl Pts',(5.30192476912948,5.87141556642451,123.916243902561));
#55774=CARTESIAN_POINT('Ctrl Pts',(5.3048351506227,5.8687858359032,123.916079250216));
#55775=CARTESIAN_POINT('Ctrl Pts',(5.30592610448748,5.86779953105878,123.916017494983));
#55776=CARTESIAN_POINT('Ctrl Pts',(5.30785786185848,5.866052096988,123.915908081987));
#55777=CARTESIAN_POINT('Ctrl Pts',(5.30869877710007,5.86529109083975,123.915860432249));
#55778=CARTESIAN_POINT('Ctrl Pts',(5.31033717022359,5.86380774721387,123.915767553123));
#55779=CARTESIAN_POINT('Ctrl Pts',(5.31113466448161,5.86308542778319,123.915722324908));
#55780=CARTESIAN_POINT('Ctrl Pts',(5.31286271665923,5.86151962645638,123.915624281056));
#55781=CARTESIAN_POINT('Ctrl Pts',(5.31379322101497,5.86067608571681,123.915571461599));
#55782=CARTESIAN_POINT('Ctrl Pts',(5.6857690934152,5.52330313541561,123.894446205186));
#55783=CARTESIAN_POINT('Ctrl Pts',(6.02398907474198,5.15231401385136,123.871208182852));
#55784=CARTESIAN_POINT('Ctrl Pts',(6.57527815338424,4.41853722665878,123.828827043769));
#55785=CARTESIAN_POINT('Ctrl Pts',(6.79898926746699,4.06590042785956,123.809711049112));
#55786=CARTESIAN_POINT('Ctrl Pts',(7.09309535526644,3.5095575321169,123.782180581988));
#55787=CARTESIAN_POINT('Ctrl Pts',(7.18472708804641,3.31793632075104,123.773120485363));
#55788=CARTESIAN_POINT('Ctrl Pts',(7.30586444551254,3.03598487377043,123.760403725367));
#55789=CARTESIAN_POINT('Ctrl Pts',(7.34162584189052,2.94845557139175,123.756538116745));
#55790=CARTESIAN_POINT('Ctrl Pts',(7.38109670292707,2.84667283325192,123.752135182576));
#55791=CARTESIAN_POINT('Ctrl Pts',(7.38634509750873,2.83302680202614,123.751546772124));
#55792=CARTESIAN_POINT('Ctrl Pts',(7.39424746612072,2.81230909735581,123.750656285061));
#55793=CARTESIAN_POINT('Ctrl Pts',(7.39692917813153,2.80524807876505,123.750353289898));
#55794=CARTESIAN_POINT('Ctrl Pts',(7.40174037957929,2.79252519137455,123.749808237648));
#55795=CARTESIAN_POINT('Ctrl Pts',(7.40387349353825,2.78686470483313,123.749566060814));
#55796=CARTESIAN_POINT('Ctrl Pts',(7.40812987002628,2.77553049488348,123.749081779572));
#55797=CARTESIAN_POINT('Ctrl Pts',(7.41025311199192,2.76985676807067,123.748839675958));
#55798=CARTESIAN_POINT('Ctrl Pts',(7.41616540501368,2.75400248471894,123.748164048706));
#55799=CARTESIAN_POINT('Ctrl Pts',(7.41994001405548,2.7438165371201,123.747731001661));
#55800=CARTESIAN_POINT('Ctrl Pts',(7.43505477364246,2.70276941688366,123.74599002222));
#55801=CARTESIAN_POINT('Ctrl Pts',(7.44622353626729,2.67184525910684,123.744687732599));
#55802=CARTESIAN_POINT('Ctrl Pts',(7.62433074617252,2.16890874868837,123.723656448207));
#55803=CARTESIAN_POINT('Ctrl Pts',(7.74629278605102,1.68214098881059,123.705524311749));
#55804=CARTESIAN_POINT('Ctrl Pts',(7.87007455811576,0.866569145374262,123.676663484459));
#55805=CARTESIAN_POINT('Ctrl Pts',(7.89897191501195,0.543373826803735,123.665578024828));
#55806=CARTESIAN_POINT('Ctrl Pts',(7.91666798732602,-0.0946874406580678,
123.643216466774));
#55807=CARTESIAN_POINT('Ctrl Pts',(7.90666549952213,-0.408915775281337,
123.631971970887));
#55808=CARTESIAN_POINT('Ctrl Pts',(7.8725152598048,-0.781700473469742,123.617568585183));
#55809=CARTESIAN_POINT('Ctrl Pts',(7.86633271057288,-0.841642158574129,
123.615219369987));
#55810=CARTESIAN_POINT('Ctrl Pts',(7.85577490281161,-0.933686722963544,
123.611553253189));
#55811=CARTESIAN_POINT('Ctrl Pts',(7.85188611331099,-0.965843998667573,
123.610261381146));
#55812=CARTESIAN_POINT('Ctrl Pts',(7.84689833289713,-1.00506648546604,123.608671231957));
#55813=CARTESIAN_POINT('Ctrl Pts',(7.8459870641719,-1.0121556576277,123.608383247767));
#55814=CARTESIAN_POINT('Ctrl Pts',(7.84454859224729,-1.02322750332178,123.607932561268));
#55815=CARTESIAN_POINT('Ctrl Pts',(7.84402795867968,-1.02721104113258,123.607770223999));
#55816=CARTESIAN_POINT('Ctrl Pts',(7.84310152080668,-1.03425774447642,123.60748272687));
#55817=CARTESIAN_POINT('Ctrl Pts',(7.84269695689589,-1.03732106405509,123.607357636677));
#55818=CARTESIAN_POINT('Ctrl Pts',(7.84175908128332,-1.04439065761155,123.607068696005));
#55819=CARTESIAN_POINT('Ctrl Pts',(7.84122449573997,-1.04839674832143,123.606904774762));
#55820=CARTESIAN_POINT('Ctrl Pts',(7.83974725213902,-1.05940261854323,123.606453921429));
#55821=CARTESIAN_POINT('Ctrl Pts',(7.83879829138257,-1.06640153414271,123.606166639636));
#55822=CARTESIAN_POINT('Ctrl Pts',(7.83407953580485,-1.10085735710837,123.604749557759));
#55823=CARTESIAN_POINT('Ctrl Pts',(7.83017488703788,-1.12829530602195,123.603612387179));
#55824=CARTESIAN_POINT('Ctrl Pts',(7.76131019396325,-1.5946258840028,123.584143694424));
#55825=CARTESIAN_POINT('Ctrl Pts',(7.65969031639534,-2.027275885833,123.563984035821));
#55826=CARTESIAN_POINT('Ctrl Pts',(7.37074422554263,-2.9147733859221,123.521172573966));
#55827=CARTESIAN_POINT('Ctrl Pts',(7.17619799029957,-3.36541643435674,123.498607944311));
#55828=CARTESIAN_POINT('Ctrl Pts',(6.84302540837918,-3.97477224277497,123.468324563319));
#55829=CARTESIAN_POINT('Ctrl Pts',(6.73790152207192,-4.1504821559099,123.45960813468));
#55830=CARTESIAN_POINT('Ctrl Pts',(6.57571754718104,-4.39913131483919,123.447315930482));
#55831=CARTESIAN_POINT('Ctrl Pts',(6.52401305311312,-4.47545215760701,123.443548526978));
#55832=CARTESIAN_POINT('Ctrl Pts',(6.46262897620268,-4.56273588221103,123.439245020194));
#55833=CARTESIAN_POINT('Ctrl Pts',(6.45423985936206,-4.57459504826287,123.438660412993));
#55834=CARTESIAN_POINT('Ctrl Pts',(6.44145058423301,-4.59256922897236,123.437774510486));
#55835=CARTESIAN_POINT('Ctrl Pts',(6.43707429860603,-4.59870114561147,123.437472310096));
#55836=CARTESIAN_POINT('Ctrl Pts',(6.42913649341898,-4.60978982194953,123.436925870435));
#55837=CARTESIAN_POINT('Ctrl Pts',(6.42557798634211,-4.61474872503483,123.436681516868));
#55838=CARTESIAN_POINT('Ctrl Pts',(6.41846158332143,-4.62464148933245,123.436194075358));
#55839=CARTESIAN_POINT('Ctrl Pts',(6.41490372869521,-4.62957537504377,123.4359509861));
#55840=CARTESIAN_POINT('Ctrl Pts',(6.40490390247358,-4.64340906072584,123.435269451836));
#55841=CARTESIAN_POINT('Ctrl Pts',(6.39844906542288,-4.65229956726581,123.434831498747));
#55842=CARTESIAN_POINT('Ctrl Pts',(6.37205586752091,-4.68849314962892,123.433048757232));
#55843=CARTESIAN_POINT('Ctrl Pts',(6.35196096816326,-4.71568191120208,123.431709979664));
#55844=CARTESIAN_POINT('Ctrl Pts',(6.04001201484681,-5.13214249092462,123.411207636524));
#55845=CARTESIAN_POINT('Ctrl Pts',(5.71302646410046,-5.49381704819989,123.393553679844));
#55846=CARTESIAN_POINT('Ctrl Pts',(4.98662054970738,-6.16180066265601,123.359112905146));
#55847=CARTESIAN_POINT('Ctrl Pts',(4.58712483576216,-6.46470545458634,123.342426188916));
#55848=CARTESIAN_POINT('Ctrl Pts',(4.02955933794191,-6.80960529652429,123.318908866944));
#55849=CARTESIAN_POINT('Ctrl Pts',(3.89501794876902,-6.88744540717358,123.313211719332));
#55850=CARTESIAN_POINT('Ctrl Pts',(3.66459793120062,-7.01184545719884,123.303279379229));
#55851=CARTESIAN_POINT('Ctrl Pts',(3.56991086900105,-7.06052330781336,123.299149722552));
#55852=CARTESIAN_POINT('Ctrl Pts',(3.45780710298393,-7.1153233937583,123.294172807741));
#55853=CARTESIAN_POINT('Ctrl Pts',(3.44131228576678,-7.12331570975056,123.293438314718));
#55854=CARTESIAN_POINT('Ctrl Pts',(3.41958066878851,-7.13375233977967,123.292467567576));
#55855=CARTESIAN_POINT('Ctrl Pts',(3.41436864218453,-7.13624839608318,123.292234516003));
#55856=CARTESIAN_POINT('Ctrl Pts',(3.40585257517752,-7.14031530259428,123.291853342184));
#55857=CARTESIAN_POINT('Ctrl Pts',(3.40255016415048,-7.14188957942224,123.291705433965));
#55858=CARTESIAN_POINT('Ctrl Pts',(3.39618174678333,-7.14492001800214,123.291420021603));
#55859=CARTESIAN_POINT('Ctrl Pts',(3.3931158922795,-7.14637649878061,123.29128253755));
#55860=CARTESIAN_POINT('Ctrl Pts',(3.38608315878731,-7.14971195982811,123.290966973913));
#55861=CARTESIAN_POINT('Ctrl Pts',(3.38211565300836,-7.15158961184786,123.290788810421));
#55862=CARTESIAN_POINT('Ctrl Pts',(3.36944076900796,-7.1575751898068,123.290219187289));
#55863=CARTESIAN_POINT('Ctrl Pts',(3.36072748439498,-7.16167050817418,123.289826926901));
#55864=CARTESIAN_POINT('Ctrl Pts',(3.28243091479241,-7.19829621187365,123.286296215133));
#55865=CARTESIAN_POINT('Ctrl Pts',(3.21238686256765,-7.22982648263096,123.283095831702));
#55866=CARTESIAN_POINT('Ctrl Pts',(3.04163948813402,-7.30371714833326,123.275214911289));
#55867=CARTESIAN_POINT('Ctrl Pts',(2.9404974910153,-7.34502060720955,123.270480922168));
#55868=CARTESIAN_POINT('Ctrl Pts',(2.78632583582631,-7.40428511840419,123.263203041203));
#55869=CARTESIAN_POINT('Ctrl Pts',(2.73390440513996,-7.42380066373664,123.260717761089));
#55870=CARTESIAN_POINT('Ctrl Pts',(2.59807059408156,-7.47273529687531,123.254258543009));
#55871=CARTESIAN_POINT('Ctrl Pts',(2.51436451923565,-7.50131416022644,123.250259457766));
#55872=CARTESIAN_POINT('Ctrl Pts',(2.07230157174148,-7.64401232509467,123.229103261318));
#55873=CARTESIAN_POINT('Ctrl Pts',(1.7066232729393,-7.73387346870796,123.21150578569));
#55874=CARTESIAN_POINT('Ctrl Pts',(1.027657488484,-7.85020177798744,123.179917548129));
#55875=CARTESIAN_POINT('Ctrl Pts',(0.71649905408271,-7.88469410262551,123.165841072037));
#55876=CARTESIAN_POINT('Ctrl Pts',(0.228787208891369,-7.90963911821695,
123.14468844352));
#55877=CARTESIAN_POINT('Ctrl Pts',(0.0532221101480262,-7.91276862218067,
123.137253380729));
#55878=CARTESIAN_POINT('Ctrl Pts',(-0.205490886865128,-7.90876824939127,
123.126567976629));
#55879=CARTESIAN_POINT('Ctrl Pts',(-0.288647972187168,-7.90617003649517,
123.123174393269));
#55880=CARTESIAN_POINT('Ctrl Pts',(-0.385474860921468,-7.90161495576565,
123.119269399932));
#55881=CARTESIAN_POINT('Ctrl Pts',(-0.399197658306523,-7.90093355305107,
123.118717050117));
#55882=CARTESIAN_POINT('Ctrl Pts',(-0.420103370630517,-7.89984087935348,
123.11787722653));
#55883=CARTESIAN_POINT('Ctrl Pts',(-0.42728758064708,-7.89945555623338,
123.117588918256));
#55884=CARTESIAN_POINT('Ctrl Pts',(-0.439764142176992,-7.89876930910933,
123.117088734832));
#55885=CARTESIAN_POINT('Ctrl Pts',(-0.445056729466244,-7.8984728654958,
123.116876715644));
#55886=CARTESIAN_POINT('Ctrl Pts',(-0.456071739729784,-7.89784479615776,
123.116435789805));
#55887=CARTESIAN_POINT('Ctrl Pts',(-0.461794109508233,-7.89751227011302,
123.116206912255));
#55888=CARTESIAN_POINT('Ctrl Pts',(-0.477485910769263,-7.89658330862678,
123.115579796605));
#55889=CARTESIAN_POINT('Ctrl Pts',(-0.487454597998916,-7.89597421227564,
123.115181966239));
#55890=CARTESIAN_POINT('Ctrl Pts',(-0.525695410727995,-7.89356496688971,
123.113658000531));
#55891=CARTESIAN_POINT('Ctrl Pts',(-0.553959104914379,-7.8916318263737,
123.112536148718));
#55892=CARTESIAN_POINT('Ctrl Pts',(-1.01258588467649,-7.85778729528332,
123.094403867211));
#55893=CARTESIAN_POINT('Ctrl Pts',(-1.43965336392091,-7.7908665892607,123.078604742236));
#55894=CARTESIAN_POINT('Ctrl Pts',(-2.39867216381311,-7.5589926621849,123.04398015812));
#55895=CARTESIAN_POINT('Ctrl Pts',(-2.92291016732958,-7.37214593848863,
123.02571224305));
#55896=CARTESIAN_POINT('Ctrl Pts',(-3.6637565331755,-7.01655022020611,122.996321897063));
#55897=CARTESIAN_POINT('Ctrl Pts',(-3.89824830688274,-6.88902937648518,
122.98641035275));
#55898=CARTESIAN_POINT('Ctrl Pts',(-4.13709715609504,-6.74303510914143,
122.975201569294));
#55899=CARTESIAN_POINT('Ctrl Pts',(-4.14834644434193,-6.73612033263785,
122.974670975217));
#55900=CARTESIAN_POINT('Ctrl Pts',(-4.16382220109497,-6.72655413790629,
122.973937253869));
#55901=CARTESIAN_POINT('Ctrl Pts',(-4.16806360752852,-6.7239268032817,122.973735772429));
#55902=CARTESIAN_POINT('Ctrl Pts',(-4.17520072783732,-6.71949637388267,
122.973396069169));
#55903=CARTESIAN_POINT('Ctrl Pts',(-4.17809777105323,-6.71769541225293,
122.973257994661));
#55904=CARTESIAN_POINT('Ctrl Pts',(-4.1838163211202,-6.7141353163762,122.972985078713));
#55905=CARTESIAN_POINT('Ctrl Pts',(-4.18663787430333,-6.71237628302267,
122.972850244168));
#55906=CARTESIAN_POINT('Ctrl Pts',(-4.19287210075292,-6.7084842358551,122.972551935545));
#55907=CARTESIAN_POINT('Ctrl Pts',(-4.19628424109712,-6.70635040568176,
122.972388404895));
#55908=CARTESIAN_POINT('Ctrl Pts',(-4.20831561679855,-6.69881363768957,
122.971810877096));
#55909=CARTESIAN_POINT('Ctrl Pts',(-4.21692602464757,-6.69339670002084,
122.971395911806));
#55910=CARTESIAN_POINT('Ctrl Pts',(-4.3067251245238,-6.63666067842869,122.967051140182));
#55911=CARTESIAN_POINT('Ctrl Pts',(-4.38698015261712,-6.58388562656992,
122.963022494602));
#55912=CARTESIAN_POINT('Ctrl Pts',(-4.46799128577512,-6.52847450135255,
122.958822245555));
#55913=CARTESIAN_POINT('Ctrl Pts',(-4.46973090975815,-6.52728358805647,
122.95873198606));
#55914=CARTESIAN_POINT('Ctrl Pts',(-4.47486210140349,-6.52376785921554,
122.958465568988));
#55915=CARTESIAN_POINT('Ctrl Pts',(-4.47825232899043,-6.52144109728049,
122.958289302421));
#55916=CARTESIAN_POINT('Ctrl Pts',(-4.48524972462477,-6.51663065457331,
122.957924992106));
#55917=CARTESIAN_POINT('Ctrl Pts',(-4.48885664675389,-6.51414661986824,
122.957736928731));
#55918=CARTESIAN_POINT('Ctrl Pts',(-4.50144104186227,-6.50546451514848,
122.95707983326));
#55919=CARTESIAN_POINT('Ctrl Pts',(-4.51040772566597,-6.49925089203213,
122.95660994656));
#55920=CARTESIAN_POINT('Ctrl Pts',(-4.54167226356457,-6.4774897122576,122.95496574359));
#55921=CARTESIAN_POINT('Ctrl Pts',(-4.56390263737819,-6.46184591355575,
122.953786269859));
#55922=CARTESIAN_POINT('Ctrl Pts',(-4.60732908589169,-6.43095028519993,
122.95146249307));
#55923=CARTESIAN_POINT('Ctrl Pts',(-4.62853118190996,-6.41570743964944,
122.950318646232));
#55924=CARTESIAN_POINT('Ctrl Pts',(-4.72320859996949,-6.34692731794189,
122.945170388786));
#55925=CARTESIAN_POINT('Ctrl Pts',(-4.79583164614981,-6.29223202403923,
122.941111666598));
#55926=CARTESIAN_POINT('Ctrl Pts',(-5.22253045967726,-5.95918930215106,
122.916680389774));
#55927=CARTESIAN_POINT('Ctrl Pts',(-5.55324910241791,-5.65227223508802,
122.89535686636));
#55928=CARTESIAN_POINT('Ctrl Pts',(-6.08953686390049,-5.06182358652705,
122.858407862712));
#55929=CARTESIAN_POINT('Ctrl Pts',(-6.30585488355206,-4.78964973631621,
122.842624683838));
#55930=CARTESIAN_POINT('Ctrl Pts',(-6.65567615128221,-4.2845351402578,122.815865347209));
#55931=CARTESIAN_POINT('Ctrl Pts',(-6.79654203363834,-4.0573762125847,122.804632354272));
#55932=CARTESIAN_POINT('Ctrl Pts',(-6.93478562452122,-3.80697073827943,
122.793071254846));
#55933=CARTESIAN_POINT('Ctrl Pts',(-6.94385658868818,-3.79040018237023,
122.792309882101));
#55934=CARTESIAN_POINT('Ctrl Pts',(-6.95679602863177,-3.76656047537226,
122.791219754553));
#55935=CARTESIAN_POINT('Ctrl Pts',(-6.96071261033063,-3.759317591738,122.790889248756));
#55936=CARTESIAN_POINT('Ctrl Pts',(-6.96748326292111,-3.7467498555765,122.790316956143));
#55937=CARTESIAN_POINT('Ctrl Pts',(-6.97034255148287,-3.74142783099522,
122.790074979957));
#55938=CARTESIAN_POINT('Ctrl Pts',(-6.97582342406232,-3.73119813385528,
122.7896105775));
#55939=CARTESIAN_POINT('Ctrl Pts',(-6.97844593176093,-3.7262909622612,122.78938811784));
#55940=CARTESIAN_POINT('Ctrl Pts',(-6.98460326355255,-3.71474021738282,
122.788865216846));
#55941=CARTESIAN_POINT('Ctrl Pts',(-6.98813379236155,-3.70809435321542,
122.788564930986));
#55942=CARTESIAN_POINT('Ctrl Pts',(-7.00026211755722,-3.68518516529812,
122.787531766979));
#55943=CARTESIAN_POINT('Ctrl Pts',(-7.00881269682523,-3.66889683744644,
122.786800593004));
#55944=CARTESIAN_POINT('Ctrl Pts',(-7.10153851085845,-3.49075271161947,
122.778840565128));
#55945=CARTESIAN_POINT('Ctrl Pts',(-7.18015041098444,-3.32605608849256,
122.771813868933));
#55946=CARTESIAN_POINT('Ctrl Pts',(-7.30469813288273,-3.04007721381244,
122.760104387756));
#55947=CARTESIAN_POINT('Ctrl Pts',(-7.35347459527433,-2.92011938333986,
122.755334783222));
#55948=CARTESIAN_POINT('Ctrl Pts',(-7.40426282111513,-2.78585910184103,
122.7501293237));
#55949=CARTESIAN_POINT('Ctrl Pts',(-7.40920455840562,-2.7726894295842,122.749620112209));
#55950=CARTESIAN_POINT('Ctrl Pts',(-7.446254215918,-2.67314617162757,122.745781519234));
#55951=CARTESIAN_POINT('Ctrl Pts',(-7.47688629920675,-2.58622968908943,
122.74248839436));
#55952=CARTESIAN_POINT('Ctrl Pts',(-7.69747606098773,-1.92361266243879,
122.717752633397));
#55953=CARTESIAN_POINT('Ctrl Pts',(-7.82219736372114,-1.32837152058472,
122.697793767267));
#55954=CARTESIAN_POINT('Ctrl Pts',(-7.89991731924511,-0.483608628044147,
122.667040804672));
#55955=CARTESIAN_POINT('Ctrl Pts',(-7.91101908225667,-0.241560065370663,
122.657921223825));
#55956=CARTESIAN_POINT('Ctrl Pts',(-7.91099898971197,0.0131177057046245,
122.647717697107));
#55957=CARTESIAN_POINT('Ctrl Pts',(-7.91096840802572,0.0256112072325062,
122.647215780486));
#55958=CARTESIAN_POINT('Ctrl Pts',(-7.91088074343932,0.0438113139206872,
122.646482655408));
#55959=CARTESIAN_POINT('Ctrl Pts',(-7.9108470804344,0.0495180560510775,
122.646252500751));
#55960=CARTESIAN_POINT('Ctrl Pts',(-7.91077671606195,0.0595975771277445,
122.645845502707));
#55961=CARTESIAN_POINT('Ctrl Pts',(-7.9107425639728,0.0639703761392062,
122.645668772545));
#55962=CARTESIAN_POINT('Ctrl Pts',(-7.91066440397266,0.0730173807747486,
122.645302797952));
#55963=CARTESIAN_POINT('Ctrl Pts',(-7.91061987890489,0.0776915794218354,
122.645113530867));
#55964=CARTESIAN_POINT('Ctrl Pts',(-7.91049517073094,0.089668804761709,
122.644628084037));
#55965=CARTESIAN_POINT('Ctrl Pts',(-7.9104090171749,0.0969717545807434,
122.644331645045));
#55966=CARTESIAN_POINT('Ctrl Pts',(-7.91001554117607,0.126821013156039,
122.643118223367));
#55967=CARTESIAN_POINT('Ctrl Pts',(-7.90962194002565,0.149365933678764,
122.642197560484));
#55968=CARTESIAN_POINT('Ctrl Pts',(-7.90629911262924,0.302241737802288,
122.635927560987));
#55969=CARTESIAN_POINT('Ctrl Pts',(-7.90024518235169,0.432480547795013,
122.630452965029));
#55970=CARTESIAN_POINT('Ctrl Pts',(-7.877415769931,0.752737674729313,122.616748103068));
#55971=CARTESIAN_POINT('Ctrl Pts',(-7.85698084752433,0.942412348686668,
122.608420909713));
#55972=CARTESIAN_POINT('Ctrl Pts',(-7.71230220748,1.9438579867356,122.563830673718));
#55973=CARTESIAN_POINT('Ctrl Pts',(-7.46904038444182,2.73349578421431,122.527179625295));
#55974=CARTESIAN_POINT('Ctrl Pts',(-7.08692234162318,3.51594849227904,122.491744644552));
#55975=CARTESIAN_POINT('Ctrl Pts',(-7.06482556210901,3.56014071777909,122.489743822403));
#55976=CARTESIAN_POINT('Ctrl Pts',(-7.03479674630671,3.61881584865546,122.487087263748));
#55977=CARTESIAN_POINT('Ctrl Pts',(-7.02723144802852,3.63348477180967,122.486423115339));
#55978=CARTESIAN_POINT('Ctrl Pts',(-7.01535042069485,3.65634588189986,122.485388019352));
#55979=CARTESIAN_POINT('Ctrl Pts',(-7.01106613528865,3.66455432219336,122.485016353029));
#55980=CARTESIAN_POINT('Ctrl Pts',(-7.0024648592051,3.68096356740355,122.484273341823));
#55981=CARTESIAN_POINT('Ctrl Pts',(-6.99814784646895,3.68916435096894,122.483901997374));
#55982=CARTESIAN_POINT('Ctrl Pts',(-6.98843768678979,3.70753181302431,122.483070256731));
#55983=CARTESIAN_POINT('Ctrl Pts',(-6.98303674050181,3.71769435651607,122.482610040309));
#55984=CARTESIAN_POINT('Ctrl Pts',(-6.96721239344636,3.74731366118479,122.481268643125));
#55985=CARTESIAN_POINT('Ctrl Pts',(-6.956729689726,3.76673867442626,122.480388835628));
#55986=CARTESIAN_POINT('Ctrl Pts',(-6.87969584823007,3.90806802665629,122.473986898395));
#55987=CARTESIAN_POINT('Ctrl Pts',(-6.81002478386326,4.02824710508736,122.468539409477));
#55988=CARTESIAN_POINT('Ctrl Pts',(-6.57231633488453,4.41447227471011,122.450992014207));
#55989=CARTESIAN_POINT('Ctrl Pts',(-6.39156777059872,4.67234231956193,122.439224261795));
#55990=CARTESIAN_POINT('Ctrl Pts',(-6.0061195887776,5.15787231355369,122.416484681092));
#55991=CARTESIAN_POINT('Ctrl Pts',(-5.8026226599834,5.38578599519231,122.405516736655));
#55992=CARTESIAN_POINT('Ctrl Pts',(-5.47051517116804,5.71700990823731,122.388514450244));
#55993=CARTESIAN_POINT('Ctrl Pts',(-5.35100357598925,5.82902202238421,122.382551593238));
#55994=CARTESIAN_POINT('Ctrl Pts',(-5.13530597928823,6.01895690236552,122.371922124156));
#55995=CARTESIAN_POINT('Ctrl Pts',(-5.0406068114037,6.09848271181901,122.367296989372));
#55996=CARTESIAN_POINT('Ctrl Pts',(-4.83044480169104,6.26673078797632,122.357043246888));
#55997=CARTESIAN_POINT('Ctrl Pts',(-4.71431939876835,6.35454963750633,122.35138416733));
#55998=CARTESIAN_POINT('Ctrl Pts',(-4.58475519957932,6.44702460868448,122.345009088054));
#55999=CARTESIAN_POINT('Ctrl Pts',(-4.573647696602,6.45490923941755,122.344462072423));
#56000=CARTESIAN_POINT('Ctrl Pts',(-4.55800643257105,6.46595150658281,122.343691031088));
#56001=CARTESIAN_POINT('Ctrl Pts',(-4.55348960134361,6.46913317030027,122.343468284786));
#56002=CARTESIAN_POINT('Ctrl Pts',(-4.54564168514022,6.47464896458877,122.343081108871));
#56003=CARTESIAN_POINT('Ctrl Pts',(-4.54231212270046,6.47698526509097,122.342916796037));
#56004=CARTESIAN_POINT('Ctrl Pts',(-4.53537718384896,6.4818434228822,122.342574453532));
#56005=CARTESIAN_POINT('Ctrl Pts',(-4.53177150336566,6.48436484165583,122.342396400234));
#56006=CARTESIAN_POINT('Ctrl Pts',(-4.52326980431445,6.49029944596295,122.34197643125));
#56007=CARTESIAN_POINT('Ctrl Pts',(-4.51837202765,6.49371009826778,122.341734377492));
#56008=CARTESIAN_POINT('Ctrl Pts',(-4.50232542696383,6.50485748524082,122.34094095447));
#56009=CARTESIAN_POINT('Ctrl Pts',(-4.49116059841535,6.51257104600539,122.340388308254));
#56010=CARTESIAN_POINT('Ctrl Pts',(-4.25703254554483,6.67343713728488,122.328785563534));
#56011=CARTESIAN_POINT('Ctrl Pts',(-4.02642181989327,6.81505428345463,122.317020456955));
#56012=CARTESIAN_POINT('Ctrl Pts',(-3.20754612325854,7.26184456429803,122.275176114511));
#56013=CARTESIAN_POINT('Ctrl Pts',(-2.5884750206989,7.50484344292046,122.243754729958));
#56014=CARTESIAN_POINT('Ctrl Pts',(-1.92317601439024,7.67371384821835,122.213486901719));
#56015=CARTESIAN_POINT('Ctrl Pts',(-1.90002473933197,7.67947890206059,122.212437475859));
#56016=CARTESIAN_POINT('Ctrl Pts',(-1.77601512153942,7.70976425557096,122.20683709894));
#56017=CARTESIAN_POINT('Ctrl Pts',(-1.67470558921842,7.73240304047764,122.202335790536));
#56018=CARTESIAN_POINT('Ctrl Pts',(-1.3733266573602,7.79354836239417,122.189173536629));
#56019=CARTESIAN_POINT('Ctrl Pts',(-1.17217746495979,7.8263293075822,122.18068661455));
#56020=CARTESIAN_POINT('Ctrl Pts',(-0.95117611264396,7.85363252483614,122.171684637346));
#56021=CARTESIAN_POINT('Ctrl Pts',(-0.932367800733935,7.85588760887096,
122.170921036352));
#56022=CARTESIAN_POINT('Ctrl Pts',(-0.90598174313536,7.85895515679507,122.169853283365));
#56023=CARTESIAN_POINT('Ctrl Pts',(-0.898410722442848,7.85982425055597,
122.169547313693));
#56024=CARTESIAN_POINT('Ctrl Pts',(-0.885285686308703,7.86131168970705,
122.169017585303));
#56025=CARTESIAN_POINT('Ctrl Pts',(-0.879732255837745,7.86193509177762,
122.168793664285));
#56026=CARTESIAN_POINT('Ctrl Pts',(-0.868191324210793,7.86321824127082,
122.168328768267));
#56027=CARTESIAN_POINT('Ctrl Pts',(-0.862203719349696,7.86387703565133,
122.168087824012));
#56028=CARTESIAN_POINT('Ctrl Pts',(-0.848131275867929,7.86540910988773,
122.167522129125));
#56029=CARTESIAN_POINT('Ctrl Pts',(-0.840045824628685,7.86627676477594,
122.167197559404));
#56030=CARTESIAN_POINT('Ctrl Pts',(-0.814138880182746,7.86901645652173,
122.166159045004));
#56031=CARTESIAN_POINT('Ctrl Pts',(-0.796312299321744,7.87084041489324,
122.165446645681));
#56032=CARTESIAN_POINT('Ctrl Pts',(-0.75465181987634,7.87495999643322,122.163786877156));
#56033=CARTESIAN_POINT('Ctrl Pts',(-0.730813335064466,7.87720802042438,
122.162841039141));
#56034=CARTESIAN_POINT('Ctrl Pts',(-0.489788201262861,7.89883370667428,
122.153316725506));
#56035=CARTESIAN_POINT('Ctrl Pts',(-0.271890820431771,7.90933313663197,
122.145028614522));
#56036=CARTESIAN_POINT('Ctrl Pts',(0.0663507461625947,7.91163458447523,
122.132559376718));
#56037=CARTESIAN_POINT('Ctrl Pts',(0.186533187647513,7.90971369851967,122.128205587216));
#56038=CARTESIAN_POINT('Ctrl Pts',(0.717179148423632,7.8891305639653,122.10924617128));
#56039=CARTESIAN_POINT('Ctrl Pts',(1.12587516059205,7.84124630562983,122.095381023819));
#56040=CARTESIAN_POINT('Ctrl Pts',(1.9985387475787,7.66934050286066,122.065174511261));
#56041=CARTESIAN_POINT('Ctrl Pts',(2.45867125354383,7.5344401071068,122.048855244614));
#56042=CARTESIAN_POINT('Ctrl Pts',(2.97557297852029,7.33047403139126,122.027412475692));
#56043=CARTESIAN_POINT('Ctrl Pts',(3.04698290774495,7.30108063940185,122.024377112767));
#56044=CARTESIAN_POINT('Ctrl Pts',(3.12586603544205,7.26725235127308,122.020930898447));
#56045=CARTESIAN_POINT('Ctrl Pts',(3.13377760587751,7.26384423872412,122.0205842109));
#56046=CARTESIAN_POINT('Ctrl Pts',(3.14559907277191,7.25872892972647,122.020064597731));
#56047=CARTESIAN_POINT('Ctrl Pts',(3.14951320023668,7.25703147321371,122.019892290609));
#56048=CARTESIAN_POINT('Ctrl Pts',(3.15625294838881,7.25410213792726,122.019595140919));
#56049=CARTESIAN_POINT('Ctrl Pts',(3.15907921921633,7.25287177526149,122.019470395469));
#56050=CARTESIAN_POINT('Ctrl Pts',(3.16493655608878,7.25031782304069,122.019211579493));
#56051=CARTESIAN_POINT('Ctrl Pts',(3.16796749746225,7.24899399048767,122.019077493817));
#56052=CARTESIAN_POINT('Ctrl Pts',(3.17507401028476,7.24588475116813,122.018762738764));
#56053=CARTESIAN_POINT('Ctrl Pts',(3.17914890382533,7.24409780753582,122.018581971494));
#56054=CARTESIAN_POINT('Ctrl Pts',(3.19233920023547,7.23830025671263,122.017995913402));
#56055=CARTESIAN_POINT('Ctrl Pts',(3.20144850619626,7.23427588885807,122.01758975346));
#56056=CARTESIAN_POINT('Ctrl Pts',(3.41222296996353,7.14068252060574,122.008159318141));
#56057=CARTESIAN_POINT('Ctrl Pts',(3.61004626403791,7.04273835772738,121.998619257022));
#56058=CARTESIAN_POINT('Ctrl Pts',(4.11488661174169,6.76592505130574,121.972971129971));
#56059=CARTESIAN_POINT('Ctrl Pts',(4.41441300108641,6.5744183991391,121.95644778251));
#56060=CARTESIAN_POINT('Ctrl Pts',(5.09911673693276,6.06869516498249,121.917037424049));
#56061=CARTESIAN_POINT('Ctrl Pts',(5.46961080371063,5.73702965473006,121.894374412123));
#56062=CARTESIAN_POINT('Ctrl Pts',(5.82116352830283,5.35709200687632,121.872242688405));
#56063=CARTESIAN_POINT('Ctrl Pts',(5.83564372284456,5.34131462683544,121.871329668968));
#56064=CARTESIAN_POINT('Ctrl Pts',(5.97007082082082,5.19364591571794,121.862840368074));
#56065=CARTESIAN_POINT('Ctrl Pts',(6.08559581346082,5.05778931317478,121.855447512981));
#56066=CARTESIAN_POINT('Ctrl Pts',(6.20773968387526,4.90389840289548,121.847514544748));
#56067=CARTESIAN_POINT('Ctrl Pts',(6.21899309682663,4.88961924859358,121.846782495844));
#56068=CARTESIAN_POINT('Ctrl Pts',(6.23478987736962,4.86943238194534,121.845753219815));
#56069=CARTESIAN_POINT('Ctrl Pts',(6.23937423024006,4.8635569034091,121.845454315077));
#56070=CARTESIAN_POINT('Ctrl Pts',(6.24733704117666,4.85332167850024,121.844934779275));
#56071=CARTESIAN_POINT('Ctrl Pts',(6.25071925119004,4.84896486520914,121.844713995054));
#56072=CARTESIAN_POINT('Ctrl Pts',(6.25776774235955,4.83986568142513,121.844253649861));
#56073=CARTESIAN_POINT('Ctrl Pts',(6.26143319628479,4.83512267271776,121.844014122655));
#56074=CARTESIAN_POINT('Ctrl Pts',(6.2699873445855,4.82402777193339,121.843454821852));
#56075=CARTESIAN_POINT('Ctrl Pts',(6.27487178740784,4.81767260175915,121.843135221216));
#56076=CARTESIAN_POINT('Ctrl Pts',(6.29069599459921,4.79701876512474,121.842099024715));
#56077=CARTESIAN_POINT('Ctrl Pts',(6.30159664599239,4.78269012651688,121.841384014736));
#56078=CARTESIAN_POINT('Ctrl Pts',(6.3270111805672,4.74904561638597,121.839714075018));
#56079=CARTESIAN_POINT('Ctrl Pts',(6.34148571191461,4.72970017280138,121.838760729592));
#56080=CARTESIAN_POINT('Ctrl Pts',(6.48880249365922,4.53091691157574,121.829034066761));
#56081=CARTESIAN_POINT('Ctrl Pts',(6.61408563806126,4.34599199150036,121.820566528056));
#56082=CARTESIAN_POINT('Ctrl Pts',(6.93768988768544,3.82185767977699,121.797905082628));
#56083=CARTESIAN_POINT('Ctrl Pts',(7.11883425924436,3.47280240196834,121.784298794586));
#56084=CARTESIAN_POINT('Ctrl Pts',(7.44091362066871,2.71997880553356,121.756241128683));
#56085=CARTESIAN_POINT('Ctrl Pts',(7.57658212731326,2.31534957153605,121.741857059236));
#56086=CARTESIAN_POINT('Ctrl Pts',(7.72735446450345,1.70656541446234,121.718929521799));
#56087=CARTESIAN_POINT('Ctrl Pts',(7.76823900840801,1.50957757846335,121.711313390728));
#56088=CARTESIAN_POINT('Ctrl Pts',(7.80359118598854,1.29924365815713,121.702775201048));
#56089=CARTESIAN_POINT('Ctrl Pts',(7.80558313897974,1.28722233456636,121.702285815255));
#56090=CARTESIAN_POINT('Ctrl Pts',(7.80827613409839,1.27073414123407,121.701612609798));
#56091=CARTESIAN_POINT('Ctrl Pts',(7.80900113784034,1.26627116880586,121.701430189888));
#56092=CARTESIAN_POINT('Ctrl Pts',(7.81023622266611,1.25862684197347,121.701117395825));
#56093=CARTESIAN_POINT('Ctrl Pts',(7.8107481864475,1.25544579693071,121.700987131961));
#56094=CARTESIAN_POINT('Ctrl Pts',(7.81174107534961,1.24925244726036,121.700733319945));
#56095=CARTESIAN_POINT('Ctrl Pts',(7.8122222018676,1.24624017503894,121.700609783458));
#56096=CARTESIAN_POINT('Ctrl Pts',(7.81336972546731,1.23902889752914,121.700313828573));
#56097=CARTESIAN_POINT('Ctrl Pts',(7.81403447957754,1.23482963505367,121.700141315867));
#56098=CARTESIAN_POINT('Ctrl Pts',(7.81601987538471,1.22222205494573,121.699622861715));
#56099=CARTESIAN_POINT('Ctrl Pts',(7.81733032918121,1.21381216314836,121.699276340863));
#56100=CARTESIAN_POINT('Ctrl Pts',(7.8286289516604,1.14052553452458,121.696250770049));
#56101=CARTESIAN_POINT('Ctrl Pts',(7.8378226091525,1.0755305889621,121.693527448176));
#56102=CARTESIAN_POINT('Ctrl Pts',(7.88313958171352,0.723634743299232,121.678595299931));
#56103=CARTESIAN_POINT('Ctrl Pts',(7.90431814033631,0.435048798668523,121.665683408695));
#56104=CARTESIAN_POINT('Ctrl Pts',(7.92028773737084,-0.430259446040728,
121.626222230339));
#56105=CARTESIAN_POINT('Ctrl Pts',(7.86791894076184,-1.0059962344632,121.599118911335));
#56106=CARTESIAN_POINT('Ctrl Pts',(7.72127117233947,-1.72978690912439,121.566453017165));
#56107=CARTESIAN_POINT('Ctrl Pts',(7.68421050449914,-1.88761859824214,121.559405528435));
#56108=CARTESIAN_POINT('Ctrl Pts',(7.59354626755409,-2.22656952633821,121.544461613735));
#56109=CARTESIAN_POINT('Ctrl Pts',(7.53825330531857,-2.4071352941949,121.536621868198));
#56110=CARTESIAN_POINT('Ctrl Pts',(7.47034455127823,-2.60350414456133,121.528223832656));
#56111=CARTESIAN_POINT('Ctrl Pts',(7.46407405902389,-2.6214270910041,121.527458495005));
#56112=CARTESIAN_POINT('Ctrl Pts',(7.45514821956075,-2.64664813121113,121.526383132741));
#56113=CARTESIAN_POINT('Ctrl Pts',(7.4525465863842,-2.65396508723531,121.52607134795));
#56114=CARTESIAN_POINT('Ctrl Pts',(7.44800286427662,-2.66668470085902,121.525529680322));
#56115=CARTESIAN_POINT('Ctrl Pts',(7.446065662357,-2.67208909135222,121.525299637277));
#56116=CARTESIAN_POINT('Ctrl Pts',(7.44201289248213,-2.68335684593689,121.52482023044));
#56117=CARTESIAN_POINT('Ctrl Pts',(7.43989627370082,-2.68921982948789,121.524570901358));
#56118=CARTESIAN_POINT('Ctrl Pts',(7.43493674177987,-2.70290694339625,121.523989126646));
#56119=CARTESIAN_POINT('Ctrl Pts',(7.43208840159596,-2.71072910677733,121.523656859655));
#56120=CARTESIAN_POINT('Ctrl Pts',(7.42281752280494,-2.73606450666283,121.522581366044));
#56121=CARTESIAN_POINT('Ctrl Pts',(7.41634536514838,-2.75355958576317,121.521839772259));
#56122=CARTESIAN_POINT('Ctrl Pts',(7.36285834336792,-2.89658528396057,121.515785700627));
#56123=CARTESIAN_POINT('Ctrl Pts',(7.31272061198845,-3.02092844213587,121.510577326969));
#56124=CARTESIAN_POINT('Ctrl Pts',(7.16793870968177,-3.3552337703441,121.496687269359));
#56125=CARTESIAN_POINT('Ctrl Pts',(7.06724763830835,-3.56243709419914,121.48820527525));
#56126=CARTESIAN_POINT('Ctrl Pts',(6.83539278860705,-3.99090536149231,121.470694839771));
#56127=CARTESIAN_POINT('Ctrl Pts',(6.70219325556437,-4.21076368456621,121.461728140067));
#56128=CARTESIAN_POINT('Ctrl Pts',(6.45665229432585,-4.5747955810532,121.446503393383));
#56129=CARTESIAN_POINT('Ctrl Pts',(6.34958781301564,-4.72227143418863,121.440218885865));
#56130=CARTESIAN_POINT('Ctrl Pts',(6.00223184329185,-5.16754041441322,121.420539185315));
#56131=CARTESIAN_POINT('Ctrl Pts',(5.7453854079956,-5.45167492711195,121.406962873621));
#56132=CARTESIAN_POINT('Ctrl Pts',(5.42462290209186,-5.75857304108338,121.389667667717));
#56133=CARTESIAN_POINT('Ctrl Pts',(5.37972980076654,-5.80053480440244,121.387239672802));
#56134=CARTESIAN_POINT('Ctrl Pts',(5.32745987636202,-5.84826293952433,121.384398229197));
#56135=CARTESIAN_POINT('Ctrl Pts',(5.32055515685786,-5.85454532526164,121.384022594869));
#56136=CARTESIAN_POINT('Ctrl Pts',(5.31032475933408,-5.86382059478943,121.383465583872));
#56137=CARTESIAN_POINT('Ctrl Pts',(5.30700761559721,-5.86682292091001,121.383284906498));
#56138=CARTESIAN_POINT('Ctrl Pts',(5.30112071032094,-5.87214204408134,121.382964132394));
#56139=CARTESIAN_POINT('Ctrl Pts',(5.29855197094898,-5.87445997368359,121.38282412016));
#56140=CARTESIAN_POINT('Ctrl Pts',(5.29313896155335,-5.87933802206616,121.382528985581));
#56141=CARTESIAN_POINT('Ctrl Pts',(5.29029436192597,-5.88189775566576,121.382373835826));
#56142=CARTESIAN_POINT('Ctrl Pts',(5.28276809049238,-5.88866044912273,121.381963201507));
#56143=CARTESIAN_POINT('Ctrl Pts',(5.2780832680002,-5.89285988282625,121.381707456557));
#56144=CARTESIAN_POINT('Ctrl Pts',(5.25683000380046,-5.91186544556353,121.380546624219));
#56145=CARTESIAN_POINT('Ctrl Pts',(5.24020437451017,-5.92660719388316,121.379636859479));
#56146=CARTESIAN_POINT('Ctrl Pts',(5.11568359582629,-6.03608470761905,121.372811990902));
#56147=CARTESIAN_POINT('Ctrl Pts',(5.00529424728843,-6.12793298147834,121.366700521332));
#56148=CARTESIAN_POINT('Ctrl Pts',(4.61161072482582,-6.43775638963521,121.344885223092));
#56149=CARTESIAN_POINT('Ctrl Pts',(4.31610407780815,-6.63949430205039,121.32849290198));
#56150=CARTESIAN_POINT('Ctrl Pts',(3.70230022648243,-7.00018620540454,121.295795048771));
#56151=CARTESIAN_POINT('Ctrl Pts',(3.38486776352805,-7.15907301267768,121.279530436843));
#56152=CARTESIAN_POINT('Ctrl Pts',(2.87541132958568,-7.37258806962727,121.255021681037));
#56153=CARTESIAN_POINT('Ctrl Pts',(2.69017660354091,-7.44217721421419,121.246414235522));
#56154=CARTESIAN_POINT('Ctrl Pts',(2.43550200956483,-7.5271004869822,121.235021806527));
#56155=CARTESIAN_POINT('Ctrl Pts',(2.3681869713717,-7.54854970042682,121.23205126208));
#56156=CARTESIAN_POINT('Ctrl Pts',(2.19563086339127,-7.60099735784208,121.224540417272));
#56157=CARTESIAN_POINT('Ctrl Pts',(2.09001450812166,-7.63071401228195,121.220041122402));
#56158=CARTESIAN_POINT('Ctrl Pts',(1.9677336511134,-7.66239003939273,121.214941806159));
#56159=CARTESIAN_POINT('Ctrl Pts',(1.95164283221605,-7.66650422926275,121.214272961597));
#56160=CARTESIAN_POINT('Ctrl Pts',(1.92790774631201,-7.67249338009361,121.213289545575));
#56161=CARTESIAN_POINT('Ctrl Pts',(1.92027349643221,-7.67440764132515,121.212973719226));
#56162=CARTESIAN_POINT('Ctrl Pts',(1.90666405947096,-7.67779858080349,121.21241156025));
#56163=CARTESIAN_POINT('Ctrl Pts',(1.90068998745135,-7.67927968333541,121.212165086533));
#56164=CARTESIAN_POINT('Ctrl Pts',(1.888205105117,-7.68235949610116,121.211650608599));
#56165=CARTESIAN_POINT('Ctrl Pts',(1.88169397724214,-7.68395690530725,121.211382646058));
#56166=CARTESIAN_POINT('Ctrl Pts',(1.86850471379202,-7.68717492699112,121.210840551327));
#56167=CARTESIAN_POINT('Ctrl Pts',(1.86182648098654,-7.68879511878323,121.210566432733));
#56168=CARTESIAN_POINT('Ctrl Pts',(1.8341065080344,-7.69548196946485,121.209430131718));
#56169=CARTESIAN_POINT('Ctrl Pts',(1.81304603809453,-7.7004709919821,121.208570424355));
#56170=CARTESIAN_POINT('Ctrl Pts',(1.59939765043249,-7.75015716026447,121.199885236114));
#56171=CARTESIAN_POINT('Ctrl Pts',(1.40521242755915,-7.78770784373213,121.192291093556));
#56172=CARTESIAN_POINT('Ctrl Pts',(0.918508583447293,-7.86302451954987,
121.173881856097));
#56173=CARTESIAN_POINT('Ctrl Pts',(0.624900715665895,-7.8917884899893,121.163336769281));
#56174=CARTESIAN_POINT('Ctrl Pts',(-0.412867854801866,-7.93516317003822,
121.127030017453));
#56175=CARTESIAN_POINT('Ctrl Pts',(-1.15664239592262,-7.86124231507165,
121.103009621466));
#56176=CARTESIAN_POINT('Ctrl Pts',(-1.92117657731123,-7.67430028416338,
121.072079164334));
#56177=CARTESIAN_POINT('Ctrl Pts',(-1.96324533251526,-7.6636461248158,121.070355601954));
#56178=CARTESIAN_POINT('Ctrl Pts',(-2.01239957239572,-7.65076623559946,
121.068314236314));
#56179=CARTESIAN_POINT('Ctrl Pts',(-2.0195729127643,-7.64887581806204,121.068015640901));
#56180=CARTESIAN_POINT('Ctrl Pts',(-2.03103035652773,-7.64583915331536,
121.067537602108));
#56181=CARTESIAN_POINT('Ctrl Pts',(-2.03531618608657,-7.64469938519352,
121.067358535107));
#56182=CARTESIAN_POINT('Ctrl Pts',(-2.04288747383055,-7.64267906816102,
121.067041753555));
#56183=CARTESIAN_POINT('Ctrl Pts',(-2.04617333010059,-7.64180000214327,
121.066904125886));
#56184=CARTESIAN_POINT('Ctrl Pts',(-2.05297345229626,-7.63997606325084,
121.066618995548));
#56185=CARTESIAN_POINT('Ctrl Pts',(-2.05648763451495,-7.63903088433876,
121.066471474856));
#56186=CARTESIAN_POINT('Ctrl Pts',(-2.06551375459497,-7.636596527822,121.066092129709));
#56187=CARTESIAN_POINT('Ctrl Pts',(-2.07102468903805,-7.63510381960646,
121.065860095625));
#56188=CARTESIAN_POINT('Ctrl Pts',(-2.0943338691581,-7.62876313199913,121.06487688757));
#56189=CARTESIAN_POINT('Ctrl Pts',(-2.11211658491264,-7.62385891792775,
121.064122381269));
#56190=CARTESIAN_POINT('Ctrl Pts',(-2.23506160015944,-7.5894893094451,121.058876221857));
#56191=CARTESIAN_POINT('Ctrl Pts',(-2.33961690560369,-7.55791234776072,
121.054264264876));
#56192=CARTESIAN_POINT('Ctrl Pts',(-2.66094247323907,-7.45356177994734,
121.039699538887));
#56193=CARTESIAN_POINT('Ctrl Pts',(-2.87522972530162,-7.37355007618528,
121.029431187133));
#56194=CARTESIAN_POINT('Ctrl Pts',(-3.30689585474702,-7.19069178779376,
121.008017501065));
#56195=CARTESIAN_POINT('Ctrl Pts',(-3.52367006988198,-7.0869849497371,120.996866064828));
#56196=CARTESIAN_POINT('Ctrl Pts',(-3.84324873672381,-6.91580307121205,
120.980102827979));
#56197=CARTESIAN_POINT('Ctrl Pts',(-3.94975566060977,-6.85553234873503,
120.974458274201));
#56198=CARTESIAN_POINT('Ctrl Pts',(-4.18465885537609,-6.71531200965327,
120.961921135795));
#56199=CARTESIAN_POINT('Ctrl Pts',(-4.31224909661232,-6.63410092024267,
120.955050887824));
#56200=CARTESIAN_POINT('Ctrl Pts',(-4.57673142187179,-6.45490208768314,
120.94073562544));
#56201=CARTESIAN_POINT('Ctrl Pts',(-4.71298454998941,-6.35610039430935,
120.933317018692));
#56202=CARTESIAN_POINT('Ctrl Pts',(-4.85431967852244,-6.24656806247061,
120.925595967097));
#56203=CARTESIAN_POINT('Ctrl Pts',(-4.8626381582432,-6.24009473032769,120.925141430621));
#56204=CARTESIAN_POINT('Ctrl Pts',(-5.04942175880539,-6.09414187730191,
120.914932986074));
#56205=CARTESIAN_POINT('Ctrl Pts',(-5.22183613861035,-5.94707189871628,
120.905468238983));
#56206=CARTESIAN_POINT('Ctrl Pts',(-5.401897692818,-5.77960185808028,120.895534300931));
#56207=CARTESIAN_POINT('Ctrl Pts',(-5.41603520152699,-5.7663557837307,120.894753958288));
#56208=CARTESIAN_POINT('Ctrl Pts',(-5.43569344783515,-5.74780100512732,
120.893668327003));
#56209=CARTESIAN_POINT('Ctrl Pts',(-5.44125529145944,-5.74253606927912,
120.893361109616));
#56210=CARTESIAN_POINT('Ctrl Pts',(-5.45084796561571,-5.7334290319795,120.892831130927));
#56211=CARTESIAN_POINT('Ctrl Pts',(-5.4548823963522,-5.72959074028389,120.892608201294));
#56212=CARTESIAN_POINT('Ctrl Pts',(-5.4632247945004,-5.72163712053802,120.892147155015));
#56213=CARTESIAN_POINT('Ctrl Pts',(-5.46753217341492,-5.71752117855677,
120.891909065839));
#56214=CARTESIAN_POINT('Ctrl Pts',(-5.47605691446778,-5.70935686787689,
120.891437782357));
#56215=CARTESIAN_POINT('Ctrl Pts',(-5.48027444664626,-5.70530868270013,
120.891204580167));
#56216=CARTESIAN_POINT('Ctrl Pts',(-5.49003737973757,-5.69591694759352,
120.890664660423));
#56217=CARTESIAN_POINT('Ctrl Pts',(-5.49557947735191,-5.6905699638392,120.890358096066));
#56218=CARTESIAN_POINT('Ctrl Pts',(-5.52582253257544,-5.66130625246897,
120.88868479371));
#56219=CARTESIAN_POINT('Ctrl Pts',(-5.55037536504422,-5.6372366006608,120.887324900041));
#56220=CARTESIAN_POINT('Ctrl Pts',(-5.77264199520862,-5.4164840876372,120.874999746493));
#56221=CARTESIAN_POINT('Ctrl Pts',(-5.95999096563526,-5.2096276781117,120.864515327959));
#56222=CARTESIAN_POINT('Ctrl Pts',(-6.23458264255635,-4.87219426990906,
120.848735903576));
#56223=CARTESIAN_POINT('Ctrl Pts',(-6.32952492460112,-4.74820113940357,
120.843189448095));
#56224=CARTESIAN_POINT('Ctrl Pts',(-6.87364290614378,-3.99224389957678,
120.810567887238));
#56225=CARTESIAN_POINT('Ctrl Pts',(-7.23151145011653,-3.29997431842656,
120.785931279604));
#56226=CARTESIAN_POINT('Ctrl Pts',(-7.49733648154149,-2.52503925339601,
120.753753275093));
#56227=CARTESIAN_POINT('Ctrl Pts',(-7.51133728667385,-2.48308066140297,
120.751996466743));
#56228=CARTESIAN_POINT('Ctrl Pts',(-7.52723972002103,-2.43405763749413,
120.7499246011));
#56229=CARTESIAN_POINT('Ctrl Pts',(-7.52948457516554,-2.42710453359414,
120.749630291228));
#56230=CARTESIAN_POINT('Ctrl Pts',(-7.53304477993711,-2.41602485548254,
120.749160581224));
#56231=CARTESIAN_POINT('Ctrl Pts',(-7.53436638296822,-2.41190028107878,
120.748985563481));
#56232=CARTESIAN_POINT('Ctrl Pts',(-7.53668909986274,-2.40463080423764,
120.748676810942));
#56233=CARTESIAN_POINT('Ctrl Pts',(-7.53769163516902,-2.40148635343119,
120.748543163705));
#56234=CARTESIAN_POINT('Ctrl Pts',(-7.53975971560277,-2.39498576823043,
120.748266674712));
#56235=CARTESIAN_POINT('Ctrl Pts',(-7.54082498410571,-2.3916295611969,120.748123816385));
#56236=CARTESIAN_POINT('Ctrl Pts',(-7.54356506636366,-2.38297669923729,
120.747755223943));
#56237=CARTESIAN_POINT('Ctrl Pts',(-7.54523653901415,-2.3776790005352,120.747529284077));
#56238=CARTESIAN_POINT('Ctrl Pts',(-7.55217770718717,-2.35559808235918,
120.746586451675));
#56239=CARTESIAN_POINT('Ctrl Pts',(-7.55739695902635,-2.33879918774146,
120.745866484908));
#56240=CARTESIAN_POINT('Ctrl Pts',(-7.59239735959962,-2.22480497897762,
120.740963531655));
#56241=CARTESIAN_POINT('Ctrl Pts',(-7.62035756342835,-2.12706459226016,
120.736674124732));
#56242=CARTESIAN_POINT('Ctrl Pts',(-7.82192065062473,-1.36739168276504,
120.702828987298));
#56243=CARTESIAN_POINT('Ctrl Pts',(-7.9108511900503,-0.686017634366207,
120.669782581568));
#56244=CARTESIAN_POINT('Ctrl Pts',(-7.91099981341223,-0.00171819428687214,
120.63838888384));
#56245=CARTESIAN_POINT('',(-7.91183059010191,0.0010273813645225,118.643768829136));
#56246=CARTESIAN_POINT('Ctrl Pts',(-7.911,6.17617068598975E-12,120.642331508237));
#56247=CARTESIAN_POINT('Ctrl Pts',(-7.91099999999828,2.20167589667282,120.553744072504));
#56248=CARTESIAN_POINT('Ctrl Pts',(-6.9421457667204,4.38610418339201,120.465156636771));
#56249=CARTESIAN_POINT('Ctrl Pts',(-3.67820201487755,7.34180684107895,120.287981765306));
#56250=CARTESIAN_POINT('Ctrl Pts',(-1.40868175871174,8.08992666571432,120.199394329573));
#56251=CARTESIAN_POINT('Ctrl Pts',(2.9730927052179,7.65454228025053,120.022219458108));
#56252=CARTESIAN_POINT('Ctrl Pts',(5.05102072676026,6.47444880833891,119.933632022375));
#56253=CARTESIAN_POINT('Ctrl Pts',(7.66951518848053,2.93425195367223,119.75645715091));
#56254=CARTESIAN_POINT('Ctrl Pts',(8.18956872247105,0.601881960094159,119.667869715177));
#56255=CARTESIAN_POINT('Ctrl Pts',(7.32306689761123,-3.71537198232875,119.490694843711));
#56256=CARTESIAN_POINT('Ctrl Pts',(5.94329958849879,-5.66643518936844,119.402107407979));
#56257=CARTESIAN_POINT('Ctrl Pts',(2.16154501637422,-7.92205913233111,119.224932536513));
#56258=CARTESIAN_POINT('Ctrl Pts',(-0.210816529304628,-8.20894963712988,
119.136345100781));
#56259=CARTESIAN_POINT('Ctrl Pts',(-4.42123908576775,-6.91982244717612,
118.959170229315));
#56260=CARTESIAN_POINT('Ctrl Pts',(-6.22631625634439,-5.35390358803224,
118.870582793582));
#56261=CARTESIAN_POINT('Ctrl Pts',(-7.65317280859622,-2.3133485751411,118.735440741312));
#56262=CARTESIAN_POINT('Ctrl Pts',(-7.91100000000081,-1.15702837836028,
118.688886124774));
#56263=CARTESIAN_POINT('Ctrl Pts',(-7.911,5.55555601522428E-12,118.642331508237));
#56264=CARTESIAN_POINT('',(-7.9109991690038,0.00362602002780672,116.642331508237));
#56265=CARTESIAN_POINT('Ctrl Pts',(-7.91099779079968,0.00591218762721216,
118.642331508237));
#56266=CARTESIAN_POINT('Ctrl Pts',(-7.91083671603242,0.221443596363675,
118.633703450411));
#56267=CARTESIAN_POINT('Ctrl Pts',(-7.90186360606107,0.436646946205818,
118.625075392585));
#56268=CARTESIAN_POINT('Ctrl Pts',(-7.88418278797969,0.650832363765712,
118.616447334758));
#56269=CARTESIAN_POINT('Ctrl Pts',(-7.86640982052795,0.866134078731944,
118.607774308985));
#56270=CARTESIAN_POINT('Ctrl Pts',(-7.83983822169058,1.08040700633278,118.599101283211));
#56271=CARTESIAN_POINT('Ctrl Pts',(-7.80462415415228,1.29296667104098,118.590428257438));
#56272=CARTESIAN_POINT('Ctrl Pts',(-7.76931804459715,1.50608192110483,118.581732562236));
#56273=CARTESIAN_POINT('Ctrl Pts',(-7.72532433869049,1.71747473790199,118.573036867034));
#56274=CARTESIAN_POINT('Ctrl Pts',(-7.67284929109888,1.92647469645552,118.564341171832));
#56275=CARTESIAN_POINT('Ctrl Pts',(-7.62016465055611,2.13630943115729,118.555610744762));
#56276=CARTESIAN_POINT('Ctrl Pts',(-7.55893089031879,2.34373195410072,118.546880317692));
#56277=CARTESIAN_POINT('Ctrl Pts',(-7.48940430250673,2.54808637875438,118.538149890622));
#56278=CARTESIAN_POINT('Ctrl Pts',(-7.42977915574986,2.72333822044306,118.530662783723));
#56279=CARTESIAN_POINT('Ctrl Pts',(-7.36405581900405,2.89633391464973,118.523175676823));
#56280=CARTESIAN_POINT('Ctrl Pts',(-7.29242264774207,3.06667457137181,118.515688569924));
#56281=CARTESIAN_POINT('Ctrl Pts',(-7.216669252574,3.24681294657604,118.507770816771));
#56282=CARTESIAN_POINT('Ctrl Pts',(-7.13413070695464,3.42439597308405,118.499853063618));
#56283=CARTESIAN_POINT('Ctrl Pts',(-7.04499911081336,3.59887600906713,118.491935310466));
#56284=CARTESIAN_POINT('Ctrl Pts',(-6.95596992046277,3.77315558004322,118.484026654241));
#56285=CARTESIAN_POINT('Ctrl Pts',(-6.86036292271164,3.94433895788806,118.476117998017));
#56286=CARTESIAN_POINT('Ctrl Pts',(-6.75841884047851,4.11189685870951,118.468209341793));
#56287=CARTESIAN_POINT('Ctrl Pts',(-6.65657301338832,4.2792932648651,118.460308308043));
#56288=CARTESIAN_POINT('Ctrl Pts',(-6.54840244666605,4.44307086265501,118.452407274293));
#56289=CARTESIAN_POINT('Ctrl Pts',(-6.43419461001667,4.60272318529286,118.444506240544));
#56290=CARTESIAN_POINT('Ctrl Pts',(-6.32007571442572,4.76225117630012,118.436611359842));
#56291=CARTESIAN_POINT('Ctrl Pts',(-6.19992911548144,4.91766001388852,118.42871647914));
#56292=CARTESIAN_POINT('Ctrl Pts',(-6.07408673908301,5.06847031027073,118.420821598438));
#56293=CARTESIAN_POINT('Ctrl Pts',(-5.94831908319837,5.21919106111867,118.412931405422));
#56294=CARTESIAN_POINT('Ctrl Pts',(-5.81686260878021,5.36531844774603,118.405041212406));
#56295=CARTESIAN_POINT('Ctrl Pts',(-5.68009101375787,5.50640418743731,118.397151019391));
#56296=CARTESIAN_POINT('Ctrl Pts',(-5.5433753302584,5.64743225200561,118.389264051845));
#56297=CARTESIAN_POINT('Ctrl Pts',(-5.40134909585611,5.78342253022632,118.381377084299));
#56298=CARTESIAN_POINT('Ctrl Pts',(-5.25442472713145,5.91396159836278,118.373490116754));
#56299=CARTESIAN_POINT('Ctrl Pts',(-5.10751311778582,6.04448933007176,118.365603834137));
#56300=CARTESIAN_POINT('Ctrl Pts',(-4.95570447470364,6.16956656137185,118.357717551521));
#56301=CARTESIAN_POINT('Ctrl Pts',(-4.79944672457402,6.28881802391958,118.349831268905));
#56302=CARTESIAN_POINT('Ctrl Pts',(-4.64318924908982,6.40806927686574,118.34194500015));
#56303=CARTESIAN_POINT('Ctrl Pts',(-4.48248295573017,6.52149457197276,118.334058731395));
#56304=CARTESIAN_POINT('Ctrl Pts',(-4.31780745996508,6.62876004533803,118.32617246264));
#56305=CARTESIAN_POINT('Ctrl Pts',(-4.1531046531704,6.73604330842061,118.318284885966));
#56306=CARTESIAN_POINT('Ctrl Pts',(-3.98443162102727,6.83716452613187,118.310397309293));
#56307=CARTESIAN_POINT('Ctrl Pts',(-3.81229566226637,6.93183401297702,118.302509732619));
#56308=CARTESIAN_POINT('Ctrl Pts',(-3.6401023041762,7.02653506768913,118.294619525806));
#56309=CARTESIAN_POINT('Ctrl Pts',(-3.46444402041368,7.11477993907158,118.286729318993));
#56310=CARTESIAN_POINT('Ctrl Pts',(-3.2858515401473,7.19632549681514,118.27883911218));
#56311=CARTESIAN_POINT('Ctrl Pts',(-3.10708660003226,7.27794979994891,118.270941286099));
#56312=CARTESIAN_POINT('Ctrl Pts',(-2.92538211741085,7.35286172449167,118.263043460019));
#56313=CARTESIAN_POINT('Ctrl Pts',(-2.7412885612694,7.42086639307389,118.255145633938));
#56314=CARTESIAN_POINT('Ctrl Pts',(-2.55709306904711,7.48890871712619,118.247243434682));
#56315=CARTESIAN_POINT('Ctrl Pts',(-2.37050619243673,7.55003605246322,118.239341235426));
#56316=CARTESIAN_POINT('Ctrl Pts',(-2.18209257317945,7.60410369485287,118.23143903617));
#56317=CARTESIAN_POINT('Ctrl Pts',(-1.9934515243977,7.65823660098645,118.22352729836));
#56318=CARTESIAN_POINT('Ctrl Pts',(-1.80297966214709,7.70529271029314,118.21561556055));
#56319=CARTESIAN_POINT('Ctrl Pts',(-1.61125187231184,7.74517839716889,118.207703822741));
#56320=CARTESIAN_POINT('Ctrl Pts',(-1.53194107755394,7.76167765128483,118.204431025333));
#56321=CARTESIAN_POINT('Ctrl Pts',(-1.45241543903234,7.77695053402871,118.201158227925));
#56322=CARTESIAN_POINT('Ctrl Pts',(-1.37271584731438,7.79099301774376,118.197885430517));
#56323=CARTESIAN_POINT('Ctrl Pts',(-1.17023137710682,7.82666929680805,118.189570574255));
#56324=CARTESIAN_POINT('Ctrl Pts',(-0.966181923830737,7.85447815505976,
118.181255717993));
#56325=CARTESIAN_POINT('Ctrl Pts',(-0.761191861567461,7.87429412391253,
118.172940861731));
#56326=CARTESIAN_POINT('Ctrl Pts',(-0.556454237440179,7.89408569008849,
118.164636244926));
#56327=CARTESIAN_POINT('Ctrl Pts',(-0.350778605037622,7.90590397008626,
118.156331628121));
#56328=CARTESIAN_POINT('Ctrl Pts',(-0.144798034947215,7.90967474230612,
118.148027011316));
#56329=CARTESIAN_POINT('Ctrl Pts',(0.0609424639345085,7.91344111967532,
118.139732073576));
#56330=CARTESIAN_POINT('Ctrl Pts',(0.266986899509766,7.90917869147408,118.131437135836));
#56331=CARTESIAN_POINT('Ctrl Pts',(0.472697746957,7.89686506406319,118.123142198096));
#56332=CARTESIAN_POINT('Ctrl Pts',(0.678100272093222,7.88456989249023,118.114859692925));
#56333=CARTESIAN_POINT('Ctrl Pts',(0.883169915056289,7.86424762120578,118.106577187755));
#56334=CARTESIAN_POINT('Ctrl Pts',(1.08726973854097,7.83592786564891,118.098294682584));
#56335=CARTESIAN_POINT('Ctrl Pts',(1.29118206726784,7.8076341258211,118.090019786074));
#56336=CARTESIAN_POINT('Ctrl Pts',(1.49412606370222,7.77135759262824,118.081744889564));
#56337=CARTESIAN_POINT('Ctrl Pts',(1.69546867099022,7.72717975626882,118.073469993054));
#56338=CARTESIAN_POINT('Ctrl Pts',(1.89658096874354,7.68305245355984,118.065204561941));
#56339=CARTESIAN_POINT('Ctrl Pts',(2.09609524681368,7.63104194528221,118.056939130827));
#56340=CARTESIAN_POINT('Ctrl Pts',(2.29338713114806,7.5712810320767,118.048673699713));
#56341=CARTESIAN_POINT('Ctrl Pts',(2.37048440328183,7.54792779885116,118.045443753413));
#56342=CARTESIAN_POINT('Ctrl Pts',(2.44724239369957,7.52339157676419,118.042213807113));
#56343=CARTESIAN_POINT('Ctrl Pts',(2.52362426201262,7.49768241419849,118.038983860813));
#56344=CARTESIAN_POINT('Ctrl Pts',(2.71911236414118,7.43188361262053,118.030717290668));
#56345=CARTESIAN_POINT('Ctrl Pts',(2.91191542388773,7.35847235377821,118.022450720523));
#56346=CARTESIAN_POINT('Ctrl Pts',(3.10144646655632,7.27770230327439,118.014184150378));
#56347=CARTESIAN_POINT('Ctrl Pts',(3.2911473312336,7.19685988187013,118.00591017329));
#56348=CARTESIAN_POINT('Ctrl Pts',(3.47757005578809,7.10864562070118,117.997636196203));
#56349=CARTESIAN_POINT('Ctrl Pts',(3.66015070824269,7.01335995033411,117.989362219115));
#56350=CARTESIAN_POINT('Ctrl Pts',(3.84290680617902,6.91798271801832,117.981080291394));
#56351=CARTESIAN_POINT('Ctrl Pts',(4.02181320126577,6.81552064636116,117.972798363673));
#56352=CARTESIAN_POINT('Ctrl Pts',(4.19633275112753,6.70631884432991,117.964516435952));
#56353=CARTESIAN_POINT('Ctrl Pts',(4.37114158767991,6.59693602746139,117.956220779961));
#56354=CARTESIAN_POINT('Ctrl Pts',(4.54154879166722,6.48079130082324,117.94792512397));
#56355=CARTESIAN_POINT('Ctrl Pts',(4.70704661993294,6.35827280932314,117.939629467979));
#56356=CARTESIAN_POINT('Ctrl Pts',(4.87269402620684,6.23564358481755,117.93132631432));
#56357=CARTESIAN_POINT('Ctrl Pts',(5.03342296815703,6.10662927642654,117.923023160661));
#56358=CARTESIAN_POINT('Ctrl Pts',(5.18875974805491,5.97165749829686,117.914720007003));
#56359=CARTESIAN_POINT('Ctrl Pts',(5.34433336011951,5.83647993723102,117.906404194051));
#56360=CARTESIAN_POINT('Ctrl Pts',(5.49449816012126,5.69532694839535,117.898088381099));
#56361=CARTESIAN_POINT('Ctrl Pts',(5.63881685028556,5.54866340021952,117.889772568147));
#56362=CARTESIAN_POINT('Ctrl Pts',(5.69487423146808,5.49169521116297,117.886542475801));
#56363=CARTESIAN_POINT('Ctrl Pts',(5.75005000122328,5.43389596882698,117.883312383455));
#56364=CARTESIAN_POINT('Ctrl Pts',(5.80432019090631,5.37529423580117,117.880082291109));
#56365=CARTESIAN_POINT('Ctrl Pts',(5.93723577686808,5.23177007034328,117.872171325266));
#56366=CARTESIAN_POINT('Ctrl Pts',(6.06499253895526,5.08313191158827,117.864260359422));
#56367=CARTESIAN_POINT('Ctrl Pts',(6.18717483688316,4.9297858511136,117.856349393579));
#56368=CARTESIAN_POINT('Ctrl Pts',(6.30923349761745,4.77659496268013,117.848446432902));
#56369=CARTESIAN_POINT('Ctrl Pts',(6.42572871750585,4.61870592930406,117.840543472226));
#56370=CARTESIAN_POINT('Ctrl Pts',(6.53628214802461,4.45656108242834,117.832640511549));
#56371=CARTESIAN_POINT('Ctrl Pts',(6.64674416788173,4.29455030437041,117.824744085403));
#56372=CARTESIAN_POINT('Ctrl Pts',(6.75127399285098,4.12829100613005,117.816847659258));
#56373=CARTESIAN_POINT('Ctrl Pts',(6.8495338025682,3.95825816331826,117.808951233112));
#56374=CARTESIAN_POINT('Ctrl Pts',(6.94773054572438,3.78833445349471,117.801059875168));
#56375=CARTESIAN_POINT('Ctrl Pts',(7.03966512005126,3.61464232196076,117.793168517223));
#56376=CARTESIAN_POINT('Ctrl Pts',(7.12504311495439,3.43768550190984,117.785277159278));
#56377=CARTESIAN_POINT('Ctrl Pts',(7.21038210406012,3.26080952636549,117.77738940658));
#56378=CARTESIAN_POINT('Ctrl Pts',(7.28917033346571,3.08067214410774,117.769501653882));
#56379=CARTESIAN_POINT('Ctrl Pts',(7.36115930315627,2.89780170362913,117.761613901183));
#56380=CARTESIAN_POINT('Ctrl Pts',(7.4331286981632,2.71498098786575,117.753728293262));
#56381=CARTESIAN_POINT('Ctrl Pts',(7.49830239240097,2.52942901533257,117.74584268534));
#56382=CARTESIAN_POINT('Ctrl Pts',(7.55647989391253,2.34169438930355,117.737957077419));
#56383=CARTESIAN_POINT('Ctrl Pts',(7.61466425695561,2.15393762160428,117.730070539458));
#56384=CARTESIAN_POINT('Ctrl Pts',(7.66585067006356,1.96399801311556,117.722184001497));
#56385=CARTESIAN_POINT('Ctrl Pts',(7.70988823705659,1.77244023089536,117.714297463537));
#56386=CARTESIAN_POINT('Ctrl Pts',(7.75393135195071,1.58085831601523,117.706409932021));
#56387=CARTESIAN_POINT('Ctrl Pts',(7.79082374821383,1.38765815696165,117.698522400506));
#56388=CARTESIAN_POINT('Ctrl Pts',(7.82046548532773,1.19341551556772,117.690634868991));
#56389=CARTESIAN_POINT('Ctrl Pts',(7.85011592503815,0.999115845959503,117.682745021754));
#56390=CARTESIAN_POINT('Ctrl Pts',(7.87251141148446,0.80377342468765,117.674855174517));
#56391=CARTESIAN_POINT('Ctrl Pts',(7.88760376240749,0.607970301293734,117.66696532728));
#56392=CARTESIAN_POINT('Ctrl Pts',(7.90270307404301,0.412076871939257,117.659071841183));
#56393=CARTESIAN_POINT('Ctrl Pts',(7.91049251161675,0.215722660212971,117.651178355086));
#56394=CARTESIAN_POINT('Ctrl Pts',(7.91097598880074,0.0194911420416452,
117.643284868989));
#56395=CARTESIAN_POINT('Ctrl Pts',(7.9114600248837,-0.176967219493072,117.635382258033));
#56396=CARTESIAN_POINT('Ctrl Pts',(7.90462123006718,-0.373302259600198,
117.627479647077));
#56397=CARTESIAN_POINT('Ctrl Pts',(7.8905155855907,-0.568933030813101,117.619577036121));
#56398=CARTESIAN_POINT('Ctrl Pts',(7.87640058548218,-0.764693555013525,
117.611669183722));
#56399=CARTESIAN_POINT('Ctrl Pts',(7.85500916458256,-0.959748537756036,
117.603761331324));
#56400=CARTESIAN_POINT('Ctrl Pts',(7.82644873420673,-1.15352555707879,117.595853478925));
#56401=CARTESIAN_POINT('Ctrl Pts',(7.79784922506148,-1.3475677183254,117.587934806342));
#56402=CARTESIAN_POINT('Ctrl Pts',(7.76206117628894,-1.54032808603793,117.580016133759));
#56403=CARTESIAN_POINT('Ctrl Pts',(7.7192425890873,-1.73124661756229,117.572097461175));
#56404=CARTESIAN_POINT('Ctrl Pts',(7.70154576191687,-1.81015282341411,117.568824691351));
#56405=CARTESIAN_POINT('Ctrl Pts',(7.68264859531561,-1.88874461788705,117.565551921526));
#56406=CARTESIAN_POINT('Ctrl Pts',(7.66256466949527,-1.96698339743956,117.562279151701));
#56407=CARTESIAN_POINT('Ctrl Pts',(7.61443390925768,-2.15448119909491,117.554436018783));
#56408=CARTESIAN_POINT('Ctrl Pts',(7.55934159075306,-2.34050541276033,117.546592885864));
#56409=CARTESIAN_POINT('Ctrl Pts',(7.49738959448499,-2.52449406188809,117.538749752945));
#56410=CARTESIAN_POINT('Ctrl Pts',(7.43551035424263,-2.70826663593039,117.530915830951));
#56411=CARTESIAN_POINT('Ctrl Pts',(7.36678758798236,-2.89000807604153,117.523081908957));
#56412=CARTESIAN_POINT('Ctrl Pts',(7.29137408996509,-3.06916680553301,117.515247986962));
#56413=CARTESIAN_POINT('Ctrl Pts',(7.216034490447,-3.24814997545531,117.507421741513));
#56414=CARTESIAN_POINT('Ctrl Pts',(7.1340173508897,-3.42455515323873,117.499595496063));
#56415=CARTESIAN_POINT('Ctrl Pts',(7.04552521067031,-3.59784595359628,117.491769250614));
#56416=CARTESIAN_POINT('Ctrl Pts',(6.95710258478053,-3.77100062667987,117.483949153012));
#56417=CARTESIAN_POINT('Ctrl Pts',(6.86221524779078,-3.9410454834532,117.47612905541));
#56418=CARTESIAN_POINT('Ctrl Pts',(6.76111385728658,-4.10746398752411,117.468308957809));
#56419=CARTESIAN_POINT('Ctrl Pts',(6.66007224322784,-4.27378409624572,117.460493483859));
#56420=CARTESIAN_POINT('Ctrl Pts',(6.55282407636424,-4.43648182369307,117.452678009909));
#56421=CARTESIAN_POINT('Ctrl Pts',(6.43966606259968,-4.59506496169552,117.444862535959));
#56422=CARTESIAN_POINT('Ctrl Pts',(6.3265529743179,-4.75358513973786,117.437050164873));
#56423=CARTESIAN_POINT('Ctrl Pts',(6.20753491778364,-4.90799369723403,117.429237793788));
#56424=CARTESIAN_POINT('Ctrl Pts',(6.08295215386101,-5.05782701304005,117.421425422702));
#56425=CARTESIAN_POINT('Ctrl Pts',(5.95837410584057,-5.20765465712041,117.413613347342));
#56426=CARTESIAN_POINT('Ctrl Pts',(5.82823198787705,-5.35290712848169,117.405801271983));
#56427=CARTESIAN_POINT('Ctrl Pts',(5.69290691429884,-5.49315318056291,117.397989196623));
#56428=CARTESIAN_POINT('Ctrl Pts',(5.55757788288406,-5.633403334404,117.390176892785));
#56429=CARTESIAN_POINT('Ctrl Pts',(5.41706583763429,-5.76864652356256,117.382364588946));
#56430=CARTESIAN_POINT('Ctrl Pts',(5.27178936098721,-5.89848776665528,117.374552285108));
#56431=CARTESIAN_POINT('Ctrl Pts',(5.12648307359517,-6.02835565318178,117.366738378184));
#56432=CARTESIAN_POINT('Ctrl Pts',(4.97641066951175,-6.15281915105685,117.35892447126));
#56433=CARTESIAN_POINT('Ctrl Pts',(4.82202457226624,-6.27152294299085,117.351110564336));
#56434=CARTESIAN_POINT('Ctrl Pts',(4.66757962833394,-6.39027198074031,117.343293679019));
#56435=CARTESIAN_POINT('Ctrl Pts',(4.50881799462534,-6.5032567252031,117.335476793702));
#56436=CARTESIAN_POINT('Ctrl Pts',(4.34622199373894,-6.61016455023171,117.327659908384));
#56437=CARTESIAN_POINT('Ctrl Pts',(4.18344961058971,-6.71718834763349,117.3198345434));
#56438=CARTESIAN_POINT('Ctrl Pts',(4.01683484662423,-6.8181218659688,117.312009178416));
#56439=CARTESIAN_POINT('Ctrl Pts',(3.84688651504871,-6.91269738527128,117.304183813432));
#56440=CARTESIAN_POINT('Ctrl Pts',(3.67683489640687,-7.00733038338419,117.296353692538));
#56441=CARTESIAN_POINT('Ctrl Pts',(3.50344598497656,-7.09559752255831,117.288523571644));
#56442=CARTESIAN_POINT('Ctrl Pts',(3.32724966263928,-7.17727877976513,117.280693450749));
#56443=CARTESIAN_POINT('Ctrl Pts',(3.15081249160492,-7.25907168983798,117.272852626599));
#56444=CARTESIAN_POINT('Ctrl Pts',(2.97156056807867,-7.33426060170491,117.265011802448));
#56445=CARTESIAN_POINT('Ctrl Pts',(2.79004113115738,-7.40267461708605,117.257170978297));
#56446=CARTESIAN_POINT('Ctrl Pts',(2.69207595825905,-7.43959733433968,117.252939322963));
#56447=CARTESIAN_POINT('Ctrl Pts',(2.59345055539616,-7.47454759113312,117.248707667628));
#56448=CARTESIAN_POINT('Ctrl Pts',(2.49425224523058,-7.50750469444823,117.244476012294));
#56449=CARTESIAN_POINT('Ctrl Pts',(2.3087987846975,-7.56911873654966,117.236564837957));
#56450=CARTESIAN_POINT('Ctrl Pts',(2.12081166575402,-7.62393979439585,117.228653663621));
#56451=CARTESIAN_POINT('Ctrl Pts',(1.93083040962673,-7.67175435798493,117.220742489285));
#56452=CARTESIAN_POINT('Ctrl Pts',(1.74105511784712,-7.71951708437911,117.212839891688));
#56453=CARTESIAN_POINT('Ctrl Pts',(1.54929032645702,-7.76028836311641,117.204937294092));
#56454=CARTESIAN_POINT('Ctrl Pts',(1.35609348820962,-7.79390347972282,117.197034696496));
#56455=CARTESIAN_POINT('Ctrl Pts',(1.16307023768138,-7.82748839308432,117.189139199399));
#56456=CARTESIAN_POINT('Ctrl Pts',(0.968617841097546,-7.8539298943556,117.181243702301));
#56457=CARTESIAN_POINT('Ctrl Pts',(0.773307077361525,-7.87311356225112,
117.173348205204));
#56458=CARTESIAN_POINT('Ctrl Pts',(0.578135556833815,-7.89228355350428,
117.165458337055));
#56459=CARTESIAN_POINT('Ctrl Pts',(0.382107230160541,-7.90420598686831,
117.157568468907));
#56460=CARTESIAN_POINT('Ctrl Pts',(0.185801475095989,-7.90881778851,117.149678600758));
#56461=CARTESIAN_POINT('Ctrl Pts',(-0.0104007477622928,-7.91342715787455,
117.141792893749));
#56462=CARTESIAN_POINT('Ctrl Pts',(-0.206879763543778,-7.91073357034298,
117.133907186739));
#56463=CARTESIAN_POINT('Ctrl Pts',(-0.403052401971563,-7.90072590090714,
117.126021479729));
#56464=CARTESIAN_POINT('Ctrl Pts',(-0.599157968129581,-7.89072165313658,
117.118138468876));
#56465=CARTESIAN_POINT('Ctrl Pts',(-0.79495702174133,-7.8734083250332,117.110255458024));
#56466=CARTESIAN_POINT('Ctrl Pts',(-0.989867441810694,-7.84882688353127,
117.102372447171));
#56467=CARTESIAN_POINT('Ctrl Pts',(-1.18478077062658,-7.82424507518808,
117.094489318677));
#56468=CARTESIAN_POINT('Ctrl Pts',(-1.37880509625493,-7.79239497147145,
117.086606190182));
#56469=CARTESIAN_POINT('Ctrl Pts',(-1.57136388485958,-7.75336936701451,
117.078723061687));
#56470=CARTESIAN_POINT('Ctrl Pts',(-1.76393457956659,-7.71434134956544,
117.070839445771));
#56471=CARTESIAN_POINT('Ctrl Pts',(-1.95503921840713,-7.66813701526065,
117.062955829854));
#56472=CARTESIAN_POINT('Ctrl Pts',(-2.14411188438199,-7.61490021124715,
117.055072213938));
#56473=CARTESIAN_POINT('Ctrl Pts',(-2.33322802301851,-7.56165116672519,
117.047186785375));
#56474=CARTESIAN_POINT('Ctrl Pts',(-2.52031092577487,-7.50136652396782,
117.039301356813));
#56475=CARTESIAN_POINT('Ctrl Pts',(-2.70481001492635,-7.43423996001973,
117.031415928251));
#56476=CARTESIAN_POINT('Ctrl Pts',(-2.88938253886896,-7.36708667818796,
117.023527361111));
#56477=CARTESIAN_POINT('Ctrl Pts',(-3.07136887611023,-7.29308616669873,
117.01563879397));
#56478=CARTESIAN_POINT('Ctrl Pts',(-3.25023837094958,-7.21248026215719,
117.00775022683));
#56479=CARTESIAN_POINT('Ctrl Pts',(-3.42929822181413,-7.13178857541108,
116.999853264539));
#56480=CARTESIAN_POINT('Ctrl Pts',(-3.60523429033463,-7.04447759645699,
116.991956302249));
#56481=CARTESIAN_POINT('Ctrl Pts',(-3.77753949333058,-6.95083566028775,
116.984059339958));
#56482=CARTESIAN_POINT('Ctrl Pts',(-3.94994977957764,-6.85713661499515,
116.976157561571));
#56483=CARTESIAN_POINT('Ctrl Pts',(-4.11872448979214,-6.757099090351,116.968255783184));
#56484=CARTESIAN_POINT('Ctrl Pts',(-4.28338527494833,-6.65105492281907,
116.960354004797));
#56485=CARTESIAN_POINT('Ctrl Pts',(-4.44825902335697,-6.54487360356156,
116.952442006682));
#56486=CARTESIAN_POINT('Ctrl Pts',(-4.60900793715952,-6.43267032105508,
116.944530008567));
#56487=CARTESIAN_POINT('Ctrl Pts',(-4.76518561554445,-6.31481805354741,
116.936618010452));
#56488=CARTESIAN_POINT('Ctrl Pts',(-4.83062245689491,-6.26543916527449,
116.933302964597));
#56489=CARTESIAN_POINT('Ctrl Pts',(-4.89525723688726,-6.21506904459781,
116.929987918742));
#56490=CARTESIAN_POINT('Ctrl Pts',(-4.95905904380867,-6.16373704825404,
116.926672872886));
#56491=CARTESIAN_POINT('Ctrl Pts',(-5.10925161418515,-6.04289902115986,
116.918869092995));
#56492=CARTESIAN_POINT('Ctrl Pts',(-5.2552544282984,-5.91638324043838,116.911065313103));
#56493=CARTESIAN_POINT('Ctrl Pts',(-5.396602472448,-5.78451404651836,116.903261533211));
#56494=CARTESIAN_POINT('Ctrl Pts',(-5.53779613515862,-5.65278888116298,
116.895466276668));
#56495=CARTESIAN_POINT('Ctrl Pts',(-5.67434489294149,-5.51572218409021,
116.887671020126));
#56496=CARTESIAN_POINT('Ctrl Pts',(-5.80581449285359,-5.37368021699944,
116.879875763584));
#56497=CARTESIAN_POINT('Ctrl Pts',(-5.93716663718702,-5.2317651508915,116.872087471361));
#56498=CARTESIAN_POINT('Ctrl Pts',(-6.0634484198576,-5.08488392492899,116.864299179139));
#56499=CARTESIAN_POINT('Ctrl Pts',(-6.18426024755322,-4.93344161722149,
116.856510886916));
#56500=CARTESIAN_POINT('Ctrl Pts',(-6.30498814006934,-4.78210452551413,
116.848728005685));
#56501=CARTESIAN_POINT('Ctrl Pts',(-6.4202534256128,-4.62621293980114,116.840945124453));
#56502=CARTESIAN_POINT('Ctrl Pts',(-6.52969474849135,-4.46620728264201,
116.833162243222));
#56503=CARTESIAN_POINT('Ctrl Pts',(-6.64150407003033,-4.30273955857937,
116.825210962598));
#56504=CARTESIAN_POINT('Ctrl Pts',(-6.74723427532696,-4.13497797762956,
116.817259681973));
#56505=CARTESIAN_POINT('Ctrl Pts',(-6.84654425013144,-3.96342690496395,
116.809308401349));
#56506=CARTESIAN_POINT('Ctrl Pts',(-6.94368381291583,-3.79562506807155,
116.801530895364));
#56507=CARTESIAN_POINT('Ctrl Pts',(-7.03468067239163,-3.62419798061624,
116.793753389378));
#56508=CARTESIAN_POINT('Ctrl Pts',(-7.1192601520836,-3.44964576253193,116.785975883393));
#56509=CARTESIAN_POINT('Ctrl Pts',(-7.20383518237405,-3.27510272696933,
116.778198786553));
#56510=CARTESIAN_POINT('Ctrl Pts',(-7.28199334988041,-3.09743520791403,
116.770421689712));
#56511=CARTESIAN_POINT('Ctrl Pts',(-7.35350673591185,-2.91716637936528,
116.762644592872));
#56512=CARTESIAN_POINT('Ctrl Pts',(-7.42502921607158,-2.73687462660684,
116.754866507043));
#56513=CARTESIAN_POINT('Ctrl Pts',(-7.48990510123846,-2.55398123613032,
116.747088421214));
#56514=CARTESIAN_POINT('Ctrl Pts',(-7.54795522932732,-2.36902782931529,
116.739310335385));
#56515=CARTESIAN_POINT('Ctrl Pts',(-7.60827034050064,-2.17685796404203,
116.731228766456));
#56516=CARTESIAN_POINT('Ctrl Pts',(-7.6612161953595,-1.98246449310634,116.723147197527));
#56517=CARTESIAN_POINT('Ctrl Pts',(-7.70664948242962,-1.78646991437507,
116.715065628598));
#56518=CARTESIAN_POINT('Ctrl Pts',(-7.75043061863374,-1.59760254641514,
116.707277940477));
#56519=CARTESIAN_POINT('Ctrl Pts',(-7.78723591500723,-1.40724882405409,
116.699490252356));
#56520=CARTESIAN_POINT('Ctrl Pts',(-7.8169897571167,-1.21597374031375,116.691702564234));
#56521=CARTESIAN_POINT('Ctrl Pts',(-7.84676024076048,-1.02459167506634,
116.683910520404));
#56522=CARTESIAN_POINT('Ctrl Pts',(-7.86947137020366,-0.832287573381514,
116.676118476574));
#56523=CARTESIAN_POINT('Ctrl Pts',(-7.88509953641388,-0.63962981547581,
116.668326432744));
#56524=CARTESIAN_POINT('Ctrl Pts',(-7.90074499513318,-0.446758882461544,
116.660525767045));
#56525=CARTESIAN_POINT('Ctrl Pts',(-7.90929183229359,-0.253533865349083,
116.652725101347));
#56526=CARTESIAN_POINT('Ctrl Pts',(-7.91076848804177,-0.0605221331858206,
116.644924435648));
#56527=CARTESIAN_POINT('Ctrl Pts',(-7.91093210062368,-0.0391365476305301,
116.644060126511));
#56528=CARTESIAN_POINT('Ctrl Pts',(-7.91100896837752,-0.0177535743505116,
116.643195817374));
#56529=CARTESIAN_POINT('Ctrl Pts',(-7.9109991690038,0.00362602002780673,
116.642331508237));
#56530=CARTESIAN_POINT('',(-7.911,5.49282841433296E-12,112.642331508237));
#56531=CARTESIAN_POINT('Ctrl Pts',(-7.91099906790742,0.00384025622421617,
116.648271708555));
#56532=CARTESIAN_POINT('Ctrl Pts',(-7.91090181332933,0.204186491404295,
116.641038596631));
#56533=CARTESIAN_POINT('Ctrl Pts',(-7.90319391388634,0.404448063733921,
116.633586206934));
#56534=CARTESIAN_POINT('Ctrl Pts',(-7.88397113197543,0.655407277402388,
116.623744455381));
#56535=CARTESIAN_POINT('Ctrl Pts',(-7.87954944499618,0.706583214937105,
116.621711092525));
#56536=CARTESIAN_POINT('Ctrl Pts',(-7.87398382771249,0.764424729315218,
116.619379512643));
#56537=CARTESIAN_POINT('Ctrl Pts',(-7.87332927737647,0.771137196198854,
116.619108425336));
#56538=CARTESIAN_POINT('Ctrl Pts',(-7.87224356805935,0.782125741787089,
116.618663800835));
#56539=CARTESIAN_POINT('Ctrl Pts',(-7.87181750573578,0.786402331549728,
116.618490549528));
#56540=CARTESIAN_POINT('Ctrl Pts',(-7.87105729432813,0.793970411920566,
116.618183580638));
#56541=CARTESIAN_POINT('Ctrl Pts',(-7.87072456471077,0.797262047257542,
116.618049943328));
#56542=CARTESIAN_POINT('Ctrl Pts',(-7.87006300203117,0.803765992781635,
116.617785640008));
#56543=CARTESIAN_POINT('Ctrl Pts',(-7.86973426680427,0.806978312546824,
116.617654979584));
#56544=CARTESIAN_POINT('Ctrl Pts',(-7.86907631285033,0.81336903876038,116.617394797561));
#56545=CARTESIAN_POINT('Ctrl Pts',(-7.86874713499281,0.816547448811426,
116.617265278323));
#56546=CARTESIAN_POINT('Ctrl Pts',(-7.86795797392982,0.824122480200145,
116.616956314078));
#56547=CARTESIAN_POINT('Ctrl Pts',(-7.86749623185531,0.828518909638366,
116.616776767759));
#56548=CARTESIAN_POINT('Ctrl Pts',(-7.865816677121,0.844382604564224,116.616128080102));
#56549=CARTESIAN_POINT('Ctrl Pts',(-7.86457748367141,0.855847522405284,
116.615657705902));
#56550=CARTESIAN_POINT('Ctrl Pts',(-7.84549494040132,1.02885611074588,116.608536564253));
#56551=CARTESIAN_POINT('Ctrl Pts',(-7.82270358772423,1.18980585930489,116.601608509287));
#56552=CARTESIAN_POINT('Ctrl Pts',(-7.78345939719205,1.41641585629904,116.591539026345));
#56553=CARTESIAN_POINT('Ctrl Pts',(-7.77109529531072,1.48275137302747,116.588552735429));
#56554=CARTESIAN_POINT('Ctrl Pts',(-7.75347795334157,1.57098921857877,116.58453611901));
#56555=CARTESIAN_POINT('Ctrl Pts',(-7.74897739584507,1.5930401142245,116.58352864544));
#56556=CARTESIAN_POINT('Ctrl Pts',(-7.62546753531652,2.18527873177784,116.556375634767));
#56557=CARTESIAN_POINT('Ctrl Pts',(-7.44394297185286,2.74061542260714,116.528726923268));
#56558=CARTESIAN_POINT('Ctrl Pts',(-7.09460680014913,3.50988620283875,116.490693269253));
#56559=CARTESIAN_POINT('Ctrl Pts',(-6.97431221853708,3.74322482906473,116.47916753938));
#56560=CARTESIAN_POINT('Ctrl Pts',(-6.76427975646116,4.10521845657186,116.46141565878));
#56561=CARTESIAN_POINT('Ctrl Pts',(-6.68193912303167,4.23792313924182,116.454935371928));
#56562=CARTESIAN_POINT('Ctrl Pts',(-6.57960044723064,4.39245163669582,116.447419374038));
#56563=CARTESIAN_POINT('Ctrl Pts',(-6.56334475899924,4.41670454354117,116.44624061879));
#56564=CARTESIAN_POINT('Ctrl Pts',(-6.54148324135061,4.44893391924601,116.44467525233));
#56565=CARTESIAN_POINT('Ctrl Pts',(-6.53599650422043,4.45699065653201,116.444284029478));
#56566=CARTESIAN_POINT('Ctrl Pts',(-6.52693013911629,4.47025098282459,116.443640270824));
#56567=CARTESIAN_POINT('Ctrl Pts',(-6.52335915320187,4.47546045105217,116.443387399354));
#56568=CARTESIAN_POINT('Ctrl Pts',(-6.51640399976914,4.4855808410209,116.442896217192));
#56569=CARTESIAN_POINT('Ctrl Pts',(-6.51302051051227,4.49049222239547,116.442657880337));
#56570=CARTESIAN_POINT('Ctrl Pts',(-6.50516250980977,4.50187111885236,116.442105763316));
#56571=CARTESIAN_POINT('Ctrl Pts',(-6.50068389815598,4.50833580232435,116.441792143475));
#56572=CARTESIAN_POINT('Ctrl Pts',(-6.48617988896869,4.52920516763934,116.440779881201));
#56573=CARTESIAN_POINT('Ctrl Pts',(-6.4761161627448,4.54358321751534,116.440082738899));
#56574=CARTESIAN_POINT('Ctrl Pts',(-6.38202976527669,4.67705683074392,116.433613296936));
#56575=CARTESIAN_POINT('Ctrl Pts',(-6.29477634304091,4.79384585985468,116.427969963229));
#56576=CARTESIAN_POINT('Ctrl Pts',(-6.19911203479009,4.91477385661273,116.422126893477));
#56577=CARTESIAN_POINT('Ctrl Pts',(-6.19387068605095,4.92137765331141,116.421807805507));
#56578=CARTESIAN_POINT('Ctrl Pts',(-6.17561253032216,4.94430650536352,116.420699887674));
#56579=CARTESIAN_POINT('Ctrl Pts',(-6.16254161237168,4.96058845572453,116.419913108852));
#56580=CARTESIAN_POINT('Ctrl Pts',(-6.13845694019903,4.99034771544492,116.41847488029));
#56581=CARTESIAN_POINT('Ctrl Pts',(-6.1274628936193,5.00384076678697,116.41782270261));
#56582=CARTESIAN_POINT('Ctrl Pts',(-6.08131523549221,5.06009787773319,116.415103060957));
#56583=CARTESIAN_POINT('Ctrl Pts',(-6.04575746103112,5.10252901804449,116.413050631394));
#56584=CARTESIAN_POINT('Ctrl Pts',(-5.53750371260452,5.69625661621901,116.384293694912));
#56585=CARTESIAN_POINT('Ctrl Pts',(-4.9916025985403,6.18021649218671,116.360800591652));
#56586=CARTESIAN_POINT('Ctrl Pts',(-4.234206288446,6.68500581428937,116.328510164025));
#56587=CARTESIAN_POINT('Ctrl Pts',(-4.07752112375769,6.78171224647276,116.321820514977));
#56588=CARTESIAN_POINT('Ctrl Pts',(-3.84798855843084,6.91254857526785,116.311805379098));
#56589=CARTESIAN_POINT('Ctrl Pts',(-3.77776622745434,6.95117438599509,116.308713400882));
#56590=CARTESIAN_POINT('Ctrl Pts',(-3.67194976963609,7.00730172534992,116.303994709643));
#56591=CARTESIAN_POINT('Ctrl Pts',(-3.63678969351032,7.02561408005244,116.302417151656));
#56592=CARTESIAN_POINT('Ctrl Pts',(-3.59499930613283,7.04698192126174,116.300528977499));
#56593=CARTESIAN_POINT('Ctrl Pts',(-3.5884999875473,7.05029375617576,116.30023495115));
#56594=CARTESIAN_POINT('Ctrl Pts',(-3.5791268698679,7.05505366422214,116.299810363572));
#56595=CARTESIAN_POINT('Ctrl Pts',(-3.57625673635926,7.05650898895833,116.299680276545));
#56596=CARTESIAN_POINT('Ctrl Pts',(-3.57060552760912,7.05937014732746,116.29942399092));
#56597=CARTESIAN_POINT('Ctrl Pts',(-3.56782450787089,7.06077608990344,116.299297799523));
#56598=CARTESIAN_POINT('Ctrl Pts',(-3.56228884039312,7.06357053717609,116.299046471669));
#56599=CARTESIAN_POINT('Ctrl Pts',(-3.5595342195601,7.0649590696443,116.298921337677));
#56600=CARTESIAN_POINT('Ctrl Pts',(-3.5529599104722,7.06826818628319,116.298622520478));
#56601=CARTESIAN_POINT('Ctrl Pts',(-3.54913948482629,7.07018728152267,116.298448739739));
#56602=CARTESIAN_POINT('Ctrl Pts',(-3.53758441794462,7.07597995441549,116.297922731515));
#56603=CARTESIAN_POINT('Ctrl Pts',(-3.52984500250232,7.0798439309398,116.29756987778));
#56604=CARTESIAN_POINT('Ctrl Pts',(-3.45193740902376,7.11858053278858,116.294012617268));
#56605=CARTESIAN_POINT('Ctrl Pts',(-3.38126336080635,7.15242042655522,116.290742337232));
#56606=CARTESIAN_POINT('Ctrl Pts',(-3.2981757548262,7.19069746791441,116.286857986446));
#56607=CARTESIAN_POINT('Ctrl Pts',(-3.28623719012119,7.1961613733691,116.286298909992));
#56608=CARTESIAN_POINT('Ctrl Pts',(-3.18444086313071,7.24244420062179,116.28152413666));
#56609=CARTESIAN_POINT('Ctrl Pts',(-3.0938429616586,7.28160669287414,116.277223617874));
#56610=CARTESIAN_POINT('Ctrl Pts',(-2.96924740462947,7.3327202136533,116.271263926551));
#56611=CARTESIAN_POINT('Ctrl Pts',(-2.93586300467866,7.34615030107099,116.26966268054));
#56612=CARTESIAN_POINT('Ctrl Pts',(-2.65645843244351,7.45634215135389,116.256231545564));
#56613=CARTESIAN_POINT('Ctrl Pts',(-2.40583014848456,7.54094027553931,116.24399697626));
#56614=CARTESIAN_POINT('Ctrl Pts',(-2.12185186155035,7.62119489548043,116.230249011718));
#56615=CARTESIAN_POINT('Ctrl Pts',(-2.09220617728504,7.62938662438005,116.228815094235));
#56616=CARTESIAN_POINT('Ctrl Pts',(-2.02906059098436,7.64643935641497,116.225764394876));
#56617=CARTESIAN_POINT('Ctrl Pts',(-1.99554868917345,7.65525356469257,116.224147483659));
#56618=CARTESIAN_POINT('Ctrl Pts',(-1.92388335229802,7.67360021887583,116.220695358925));
#56619=CARTESIAN_POINT('Ctrl Pts',(-1.88571451422883,7.68306893409005,116.218860164627));
#56620=CARTESIAN_POINT('Ctrl Pts',(-1.80370339383224,7.70276584689238,116.214925842413));
#56621=CARTESIAN_POINT('Ctrl Pts',(-1.75984111724073,7.7129052167111,116.212827035881));
#56622=CARTESIAN_POINT('Ctrl Pts',(-1.66500130565015,7.73397760859545,116.20830280711));
#56623=CARTESIAN_POINT('Ctrl Pts',(-1.61399727606799,7.74478223271647,116.205878309065));
#56624=CARTESIAN_POINT('Ctrl Pts',(-1.50270659440359,7.76721076318736,116.200609930504));
#56625=CARTESIAN_POINT('Ctrl Pts',(-1.44238367434907,7.77863867162948,116.197768216039));
#56626=CARTESIAN_POINT('Ctrl Pts',(-1.174567705809,7.82615267629989,116.185222828359));
#56627=CARTESIAN_POINT('Ctrl Pts',(-0.965808590787287,7.8546480169439,116.175635044654));
#56628=CARTESIAN_POINT('Ctrl Pts',(-0.393591458958936,7.90959352423486,
116.150040502727));
#56629=CARTESIAN_POINT('Ctrl Pts',(-0.0290336427505016,7.91933007611112,
116.134503568535));
#56630=CARTESIAN_POINT('Ctrl Pts',(0.352782493072675,7.90315029781344,116.119064140596));
#56631=CARTESIAN_POINT('Ctrl Pts',(0.370627792324953,7.90233352639464,116.118344371987));
#56632=CARTESIAN_POINT('Ctrl Pts',(0.396508118067032,7.90106113606163,116.117303158974));
#56633=CARTESIAN_POINT('Ctrl Pts',(0.404545393383706,7.90065369375698,116.11698017385));
#56634=CARTESIAN_POINT('Ctrl Pts',(0.418583479330228,7.89992056834951,116.11641668238));
#56635=CARTESIAN_POINT('Ctrl Pts',(0.424584559312617,7.8996003106233,116.116176002723));
#56636=CARTESIAN_POINT('Ctrl Pts',(0.436186985433,7.89896786840578,116.11571106964));
#56637=CARTESIAN_POINT('Ctrl Pts',(0.441788374317177,7.89865656329278,116.11548678827));
#56638=CARTESIAN_POINT('Ctrl Pts',(0.455081633405319,7.89790358681932,116.114954942356));
#56639=CARTESIAN_POINT('Ctrl Pts',(0.462773205864404,7.8974566361674,116.114647546675));
#56640=CARTESIAN_POINT('Ctrl Pts',(0.489861386752654,7.89584285626502,116.113566130658));
#56641=CARTESIAN_POINT('Ctrl Pts',(0.509254411105159,7.89461579437881,116.112794034822));
#56642=CARTESIAN_POINT('Ctrl Pts',(0.752594531968337,7.87831846331943,116.103132047586));
#56643=CARTESIAN_POINT('Ctrl Pts',(0.975814751531368,7.85379497354143,116.094551078133));
#56644=CARTESIAN_POINT('Ctrl Pts',(1.60689149870922,7.757137655432,116.070874600331));
#56645=CARTESIAN_POINT('Ctrl Pts',(2.01054410206709,7.66244223681423,116.056462604569));
#56646=CARTESIAN_POINT('Ctrl Pts',(2.77568705046096,7.41828359616922,116.028787511476));
#56647=CARTESIAN_POINT('Ctrl Pts',(3.13718223019088,7.27278709330631,116.015531733195));
#56648=CARTESIAN_POINT('Ctrl Pts',(3.60268807190867,7.0442400289475,115.996702295834));
#56649=CARTESIAN_POINT('Ctrl Pts',(3.71746907004695,6.98434681082448,115.991905971416));
#56650=CARTESIAN_POINT('Ctrl Pts',(3.8943716936779,6.88644188416451,115.984197494795));
#56651=CARTESIAN_POINT('Ctrl Pts',(3.95752897593229,6.85034137118276,115.981380532285));
#56652=CARTESIAN_POINT('Ctrl Pts',(4.04294151447298,6.79994437031201,115.977470411399));
#56653=CARTESIAN_POINT('Ctrl Pts',(4.06563651089896,6.78639958027024,115.97642175276));
#56654=CARTESIAN_POINT('Ctrl Pts',(4.09886672812555,6.76634066202132,115.97487247072));
#56655=CARTESIAN_POINT('Ctrl Pts',(4.10945537794118,6.75991500712004,115.974376725403));
#56656=CARTESIAN_POINT('Ctrl Pts',(4.12607604377352,6.74977537844769,115.973595355229));
#56657=CARTESIAN_POINT('Ctrl Pts',(4.13211826766775,6.74607810509266,115.973310628537));
#56658=CARTESIAN_POINT('Ctrl Pts',(4.14229902657093,6.73982962771544,115.972829761851));
#56659=CARTESIAN_POINT('Ctrl Pts',(4.14644019853362,6.73728271011331,115.972633849068));
#56660=CARTESIAN_POINT('Ctrl Pts',(4.15455974076809,6.73227868000615,115.972249114284));
#56661=CARTESIAN_POINT('Ctrl Pts',(4.15853828601928,6.72982185413918,115.972060307348));
#56662=CARTESIAN_POINT('Ctrl Pts',(4.16612658234032,6.72512664123397,115.971699647776));
#56663=CARTESIAN_POINT('Ctrl Pts',(4.169736714723,6.72288887090255,115.971527827203));
#56664=CARTESIAN_POINT('Ctrl Pts',(4.1780509273921,6.71772596441377,115.971131577839));
#56665=CARTESIAN_POINT('Ctrl Pts',(4.18275373753407,6.71479879488276,115.970907044369));
#56666=CARTESIAN_POINT('Ctrl Pts',(4.19705172758589,6.70587844967117,115.970223181513));
#56667=CARTESIAN_POINT('Ctrl Pts',(4.20663710283854,6.69986964566608,115.969763056974));
#56668=CARTESIAN_POINT('Ctrl Pts',(4.27471133874205,6.65699213027726,115.966483634586));
#56669=CARTESIAN_POINT('Ctrl Pts',(4.33272640076335,6.61937933579364,115.963627444815));
#56670=CARTESIAN_POINT('Ctrl Pts',(4.7628140245435,6.33246482382478,115.942030524016));
#56671=CARTESIAN_POINT('Ctrl Pts',(5.11359491994557,6.05273702622087,115.922071124785));
#56672=CARTESIAN_POINT('Ctrl Pts',(5.90902990068829,5.29967688001256,115.87347903305));
#56673=CARTESIAN_POINT('Ctrl Pts',(6.32286901234377,4.7984071611308,115.845304962315));
#56674=CARTESIAN_POINT('Ctrl Pts',(6.69494585501499,4.21468938097619,115.817176650297));
#56675=CARTESIAN_POINT('Ctrl Pts',(6.71857960990425,4.17691209643038,115.8153738654));
#56676=CARTESIAN_POINT('Ctrl Pts',(6.7498832973406,4.12592168017611,115.812963551817));
#56677=CARTESIAN_POINT('Ctrl Pts',(6.75783581144726,4.11288334218295,115.812349233119));
#56678=CARTESIAN_POINT('Ctrl Pts',(6.77094147546803,4.09125565862892,115.811333496288));
#56679=CARTESIAN_POINT('Ctrl Pts',(6.77611614609079,4.08267942701656,115.810931567106));
#56680=CARTESIAN_POINT('Ctrl Pts',(6.78617431426053,4.06593773917696,115.810148606209));
#56681=CARTESIAN_POINT('Ctrl Pts',(6.79105939864988,4.05777325228817,115.809767536982));
#56682=CARTESIAN_POINT('Ctrl Pts',(6.80234599346721,4.03883239240284,115.808885249042));
#56683=CARTESIAN_POINT('Ctrl Pts',(6.80873665126472,4.02804956817804,115.80838428727));
#56684=CARTESIAN_POINT('Ctrl Pts',(6.82929834264459,3.99316750654709,115.806767927087));
#56685=CARTESIAN_POINT('Ctrl Pts',(6.84336731071729,3.96900824543168,115.805654950098));
#56686=CARTESIAN_POINT('Ctrl Pts',(6.98006732455026,3.73137894057308,115.794771039067));
#56687=CARTESIAN_POINT('Ctrl Pts',(7.09280210049344,3.5123632550971,115.785244587339));
#56688=CARTESIAN_POINT('Ctrl Pts',(7.43284713766094,2.76834046273727,115.754292665549));
#56689=CARTESIAN_POINT('Ctrl Pts',(7.61345241698799,2.22401991848581,115.734016104148));
#56690=CARTESIAN_POINT('Ctrl Pts',(7.77557796106222,1.47095307467421,115.70593025629));
#56691=CARTESIAN_POINT('Ctrl Pts',(7.81003303182561,1.2754196656315,115.698617994516));
#56692=CARTESIAN_POINT('Ctrl Pts',(7.85306928074295,0.962777758997314,115.686667827457));
#56693=CARTESIAN_POINT('Ctrl Pts',(7.86646167605596,0.846414387519442,115.682163362771));
#56694=CARTESIAN_POINT('Ctrl Pts',(7.88065136374469,0.6932547232068,115.676118192187));
#56695=CARTESIAN_POINT('Ctrl Pts',(7.88378276295673,0.656686619546123,115.674666168826));
#56696=CARTESIAN_POINT('Ctrl Pts',(7.88788077509335,0.6045664661074,115.672582797481));
#56697=CARTESIAN_POINT('Ctrl Pts',(7.8890561053163,0.58903098085984,115.671960058646));
#56698=CARTESIAN_POINT('Ctrl Pts',(7.89078802671747,0.565202965195084,115.6710021159));
#56699=CARTESIAN_POINT('Ctrl Pts',(7.89137745896507,0.556912806318153,115.670668312633));
#56700=CARTESIAN_POINT('Ctrl Pts',(7.89232636199662,0.543262784569546,115.670117820148));
#56701=CARTESIAN_POINT('Ctrl Pts',(7.89269344026632,0.53790344406409,115.669901461163));
#56702=CARTESIAN_POINT('Ctrl Pts',(7.89339296164801,0.527535543119284,115.669482469001));
#56703=CARTESIAN_POINT('Ctrl Pts',(7.89372609724392,0.522527030661014,115.669279866311));
#56704=CARTESIAN_POINT('Ctrl Pts',(7.89432487212466,0.513393513420458,115.668910037227));
#56705=CARTESIAN_POINT('Ctrl Pts',(7.89459204585982,0.509268608511942,115.668742878958));
#56706=CARTESIAN_POINT('Ctrl Pts',(7.89517761394497,0.500116801778324,115.668371706981));
#56707=CARTESIAN_POINT('Ctrl Pts',(7.89549444028891,0.49508980432794,115.668167623222));
#56708=CARTESIAN_POINT('Ctrl Pts',(7.89634493891155,0.4813867107484,115.667610751676));
#56709=CARTESIAN_POINT('Ctrl Pts',(7.89686911170679,0.47271004982859,115.667257534852));
#56710=CARTESIAN_POINT('Ctrl Pts',(7.89930735816456,0.43121348771975,115.665565268938));
#56711=CARTESIAN_POINT('Ctrl Pts',(7.90103111392026,0.398383100949825,115.664217477952));
#56712=CARTESIAN_POINT('Ctrl Pts',(7.92358590531018,-0.0892208495931408,
115.644056057509));
#56713=CARTESIAN_POINT('Ctrl Pts',(7.90532444936921,-0.544893638295657,
115.623297776831));
#56714=CARTESIAN_POINT('Ctrl Pts',(7.80992642604498,-1.29628346053187,115.588424057613));
#56715=CARTESIAN_POINT('Ctrl Pts',(7.7546939890279,-1.59374755679164,115.574439893761));
#56716=CARTESIAN_POINT('Ctrl Pts',(7.63589573263551,-2.07732949870228,115.551891281789));
#56717=CARTESIAN_POINT('Ctrl Pts',(7.58218442227572,-2.26554332923599,115.543159966489));
#56718=CARTESIAN_POINT('Ctrl Pts',(7.44378190449087,-2.69016803723906,115.523663193885));
#56719=CARTESIAN_POINT('Ctrl Pts',(7.35470417322022,-2.92493330692503,115.513033787937));
#56720=CARTESIAN_POINT('Ctrl Pts',(7.23594940239037,-3.19799103149877,115.500872744973));
#56721=CARTESIAN_POINT('Ctrl Pts',(7.21690761680385,-3.24073370431275,115.498974941931));
#56722=CARTESIAN_POINT('Ctrl Pts',(7.19266433846465,-3.29387852959899,115.49662229893));
#56723=CARTESIAN_POINT('Ctrl Pts',(7.18781785887241,-3.30444102425456,115.496155060772));
#56724=CARTESIAN_POINT('Ctrl Pts',(7.18011193114909,-3.32113827875267,115.495416992489));
#56725=CARTESIAN_POINT('Ctrl Pts',(7.17726786370809,-3.327280093907,115.495145622847));
#56726=CARTESIAN_POINT('Ctrl Pts',(7.17192348302463,-3.33878264378533,115.494637612243));
#56727=CARTESIAN_POINT('Ctrl Pts',(7.16942503378652,-3.34414423641057,115.49440090596));
#56728=CARTESIAN_POINT('Ctrl Pts',(7.16383136121043,-3.3561129991475,115.493872699833));
#56729=CARTESIAN_POINT('Ctrl Pts',(7.16073300413596,-3.36271870348419,115.493581310656));
#56730=CARTESIAN_POINT('Ctrl Pts',(7.152899230657,-3.37936040412829,115.492847551501));
#56731=CARTESIAN_POINT('Ctrl Pts',(7.14815182079555,-3.38939075544526,115.492405605259));
#56732=CARTESIAN_POINT('Ctrl Pts',(7.12280578086598,-3.44265188587129,115.490060487041));
#56733=CARTESIAN_POINT('Ctrl Pts',(7.10183583181089,-3.48570539800617,115.488170487759));
#56734=CARTESIAN_POINT('Ctrl Pts',(7.07436548015585,-3.540827831956,115.485757453502));
#56735=CARTESIAN_POINT('Ctrl Pts',(7.06822309401343,-3.5530734551986,115.485221822784));
#56736=CARTESIAN_POINT('Ctrl Pts',(6.64679847104864,-4.38781911778258,115.448738321643));
#56737=CARTESIAN_POINT('Ctrl Pts',(6.09114533849994,-5.13133949425804,115.419251059324));
#56738=CARTESIAN_POINT('Ctrl Pts',(5.25418110055923,-5.91856052692249,115.379186349169));
#56739=CARTESIAN_POINT('Ctrl Pts',(5.08165324824459,-6.06733609464714,115.37104384702));
#56740=CARTESIAN_POINT('Ctrl Pts',(4.81154683374247,-6.2806453311819,115.358079316186));
#56741=CARTESIAN_POINT('Ctrl Pts',(4.71855499950254,-6.35080507554742,115.353579302401));
#56742=CARTESIAN_POINT('Ctrl Pts',(4.61376281470051,-6.42629555079542,115.348428964343));
#56743=CARTESIAN_POINT('Ctrl Pts',(4.60345558394729,-6.4336831208573,115.347921549043));
#56744=CARTESIAN_POINT('Ctrl Pts',(4.58774034795296,-6.444889706652,115.347146564977));
#56745=CARTESIAN_POINT('Ctrl Pts',(4.58234519740399,-6.44872679855975,115.34688026838));
#56746=CARTESIAN_POINT('Ctrl Pts',(4.57237374290582,-6.45579977762838,115.34638763896));
#56747=CARTESIAN_POINT('Ctrl Pts',(4.56779880022876,-6.45903758573642,115.346161442868));
#56748=CARTESIAN_POINT('Ctrl Pts',(4.56036080449279,-6.46428979763383,115.345793398809));
#56749=CARTESIAN_POINT('Ctrl Pts',(4.55749984192238,-6.46630717224482,115.345651763647));
#56750=CARTESIAN_POINT('Ctrl Pts',(4.55195416979389,-6.47021212996013,115.345377081885));
#56751=CARTESIAN_POINT('Ctrl Pts',(4.5492696318142,-6.47209993646396,115.345244052576));
#56752=CARTESIAN_POINT('Ctrl Pts',(4.54313503038467,-6.47640817561383,115.344939919457));
#56753=CARTESIAN_POINT('Ctrl Pts',(4.53968420846513,-6.47882752114685,115.344768738353));
#56754=CARTESIAN_POINT('Ctrl Pts',(4.53056840666725,-6.485207683078,115.344316278718));
#56755=CARTESIAN_POINT('Ctrl Pts',(4.52490017805842,-6.48916382580535,115.344034671215));
#56756=CARTESIAN_POINT('Ctrl Pts',(4.48850914283008,-6.51449210107582,115.342225032297));
#56757=CARTESIAN_POINT('Ctrl Pts',(4.45764065546592,-6.53565309340281,115.340682398058));
#56758=CARTESIAN_POINT('Ctrl Pts',(3.93458242925358,-6.8887910125632,115.31443248094));
#56759=CARTESIAN_POINT('Ctrl Pts',(3.406739498924,-7.16452613142196,115.286445106328));
#56760=CARTESIAN_POINT('Ctrl Pts',(2.51326301751179,-7.5100039648883,115.242192396197));
#56761=CARTESIAN_POINT('Ctrl Pts',(2.16476895094236,-7.61777272368432,115.225595298003));
#56762=CARTESIAN_POINT('Ctrl Pts',(1.56378171512177,-7.75902792204781,115.198661016452));
#56763=CARTESIAN_POINT('Ctrl Pts',(1.31485052534034,-7.80506961066854,115.187969104255));
#56764=CARTESIAN_POINT('Ctrl Pts',(1.02494801678207,-7.84442257563391,115.176059686907));
#56765=CARTESIAN_POINT('Ctrl Pts',(0.985733056024901,-7.84944675665488,
115.174459895589));
#56766=CARTESIAN_POINT('Ctrl Pts',(0.935655542244121,-7.85548143742645,
115.172431016765));
#56767=CARTESIAN_POINT('Ctrl Pts',(0.924826681624134,-7.85676367964011,
115.171993124981));
#56768=CARTESIAN_POINT('Ctrl Pts',(0.907465239926092,-7.85878305179962,
115.171292406771));
#56769=CARTESIAN_POINT('Ctrl Pts',(0.90093434994248,-7.85953443368617,115.171029118682));
#56770=CARTESIAN_POINT('Ctrl Pts',(0.888554272140645,-7.86094313363883,
115.170530596381));
#56771=CARTESIAN_POINT('Ctrl Pts',(0.882705274659372,-7.86160206593607,
115.170295310027));
#56772=CARTESIAN_POINT('Ctrl Pts',(0.869453242053805,-7.86308002855273,
115.169762769259));
#56773=CARTESIAN_POINT('Ctrl Pts',(0.862049769791817,-7.86389513347848,
115.169465642142));
#56774=CARTESIAN_POINT('Ctrl Pts',(0.843026764398102,-7.8659623349778,115.168703169819));
#56775=CARTESIAN_POINT('Ctrl Pts',(0.831405568861974,-7.86719914343043,
115.168238319652));
#56776=CARTESIAN_POINT('Ctrl Pts',(0.76403082555413,-7.87421867803947,115.165548761716));
#56777=CARTESIAN_POINT('Ctrl Pts',(0.708219147866111,-7.87943454176536,
115.163342417494));
#56778=CARTESIAN_POINT('Ctrl Pts',(-0.296873217622958,-7.96259959581657,
115.123983272364));
#56779=CARTESIAN_POINT('Ctrl Pts',(-1.25227004437144,-7.86909068245732,
115.093841062277));
#56780=CARTESIAN_POINT('Ctrl Pts',(-2.31832385121852,-7.56529557336172,
115.054215274145));
#56781=CARTESIAN_POINT('Ctrl Pts',(-2.46724638868333,-7.51804588946125,
115.048504191553));
#56782=CARTESIAN_POINT('Ctrl Pts',(-2.71444502946125,-7.43147938887357,
115.038583546642));
#56783=CARTESIAN_POINT('Ctrl Pts',(-2.81350958885966,-7.3945425675753,115.034486100323));
#56784=CARTESIAN_POINT('Ctrl Pts',(-2.9286072683571,-7.34898001146861,115.02954978517));
#56785=CARTESIAN_POINT('Ctrl Pts',(-2.94539130330259,-7.34226925422444,
115.028825527766));
#56786=CARTESIAN_POINT('Ctrl Pts',(-2.96740674226264,-7.33337918971146,
115.027869528586));
#56787=CARTESIAN_POINT('Ctrl Pts',(-2.97265909361747,-7.3312516685059,115.027640999898));
#56788=CARTESIAN_POINT('Ctrl Pts',(-2.98127204410904,-7.32775212291198,
115.027265511959));
#56789=CARTESIAN_POINT('Ctrl Pts',(-2.9846339619335,-7.32638343857433,115.027118761856));
#56790=CARTESIAN_POINT('Ctrl Pts',(-2.991147843542,-7.32372631745953,115.02683406977));
#56791=CARTESIAN_POINT('Ctrl Pts',(-2.99429992048068,-7.32243815823089,
115.026696144918));
#56792=CARTESIAN_POINT('Ctrl Pts',(-3.00157621866272,-7.3194590696334,115.026377385005));
#56793=CARTESIAN_POINT('Ctrl Pts',(-3.00569984116402,-7.31776669026507,
115.026196461101));
#56794=CARTESIAN_POINT('Ctrl Pts',(-3.01889358013371,-7.31233880321456,
115.025616706514));
#56795=CARTESIAN_POINT('Ctrl Pts',(-3.02795814986253,-7.30858992297624,
115.025217063334));
#56796=CARTESIAN_POINT('Ctrl Pts',(-3.10781721396611,-7.27538813421967,
115.021684610535));
#56797=CARTESIAN_POINT('Ctrl Pts',(-3.17818491582602,-7.24492513839153,
115.018491645827));
#56798=CARTESIAN_POINT('Ctrl Pts',(-3.26343107511898,-7.20654018551908,
115.014535265325));
#56799=CARTESIAN_POINT('Ctrl Pts',(-3.27874351568692,-7.1995864311048,115.013821088294));
#56800=CARTESIAN_POINT('Ctrl Pts',(-3.30008663153042,-7.18981178813383,
115.012820857425));
#56801=CARTESIAN_POINT('Ctrl Pts',(-3.30613617506278,-7.1870319963067,115.012536812));
#56802=CARTESIAN_POINT('Ctrl Pts',(-3.32798594055171,-7.17695850795335,
115.011508971098));
#56803=CARTESIAN_POINT('Ctrl Pts',(-3.34376551305338,-7.16962035479225,
115.010763039261));
#56804=CARTESIAN_POINT('Ctrl Pts',(-3.37600400594731,-7.15449854511342,
115.009231796671));
#56805=CARTESIAN_POINT('Ctrl Pts',(-3.39246052387339,-7.14671001692831,
115.008446263732));
#56806=CARTESIAN_POINT('Ctrl Pts',(-3.44367529872468,-7.12225437390386,
115.005989771782));
#56807=CARTESIAN_POINT('Ctrl Pts',(-3.47833841040738,-7.10539012027898,
115.004310157035));
#56808=CARTESIAN_POINT('Ctrl Pts',(-4.21224268021214,-6.74167460247681,
114.96840730019));
#56809=CARTESIAN_POINT('Ctrl Pts',(-4.85649522620086,-6.29347811850427,
114.930802124614));
#56810=CARTESIAN_POINT('Ctrl Pts',(-5.63933860977059,-5.5559615477231,114.883476861699));
#56811=CARTESIAN_POINT('Ctrl Pts',(-5.84248052901552,-5.34193730675529,
114.870936859068));
#56812=CARTESIAN_POINT('Ctrl Pts',(-6.06150482349919,-5.08369877083443,
114.857126993756));
#56813=CARTESIAN_POINT('Ctrl Pts',(-6.08951825665932,-5.05010904826316,
114.855354502633));
#56814=CARTESIAN_POINT('Ctrl Pts',(-6.12460169334882,-5.00732557836908,
114.853126466242));
#56815=CARTESIAN_POINT('Ctrl Pts',(-6.13193171092298,-4.99834661103127,
114.852660499792));
#56816=CARTESIAN_POINT('Ctrl Pts',(-6.14359003952098,-4.98400140006619,
114.851918639451));
#56817=CARTESIAN_POINT('Ctrl Pts',(-6.1479311019895,-4.97864556833096,114.851642236749));
#56818=CARTESIAN_POINT('Ctrl Pts',(-6.15610882925944,-4.96852920537994,
114.851121231903));
#56819=CARTESIAN_POINT('Ctrl Pts',(-6.15994698563641,-4.96376988958623,
114.85087657046));
#56820=CARTESIAN_POINT('Ctrl Pts',(-6.16858057874928,-4.95303879468147,
114.850325927352));
#56821=CARTESIAN_POINT('Ctrl Pts',(-6.17337287159187,-4.94706448784086,
114.850020070592));
#56822=CARTESIAN_POINT('Ctrl Pts',(-6.18556994534602,-4.93181369626165,
114.849241084323));
#56823=CARTESIAN_POINT('Ctrl Pts',(-6.19296255037568,-4.92252747423548,
114.848768436781));
#56824=CARTESIAN_POINT('Ctrl Pts',(-6.234214633144,-4.87046864908639,114.84612809672));
#56825=CARTESIAN_POINT('Ctrl Pts',(-6.2676522601347,-4.82736286683613,114.843977031312));
#56826=CARTESIAN_POINT('Ctrl Pts',(-6.86012938247671,-4.04704239753016,
114.80565061011));
#56827=CARTESIAN_POINT('Ctrl Pts',(-7.28593320415537,-3.21789268654761,
114.775773351169));
#56828=CARTESIAN_POINT('Ctrl Pts',(-7.59000785595909,-2.23312559008803,
114.738715804427));
#56829=CARTESIAN_POINT('Ctrl Pts',(-7.61913541542674,-2.13162934573914,
114.734866028635));
#56830=CARTESIAN_POINT('Ctrl Pts',(-7.68596551022528,-1.87985459738685,
114.725178933269));
#56831=CARTESIAN_POINT('Ctrl Pts',(-7.72130034791914,-1.72899834857297,
114.719255656064));
#56832=CARTESIAN_POINT('Ctrl Pts',(-7.75681897312978,-1.55441992752245,
114.712169327939));
#56833=CARTESIAN_POINT('Ctrl Pts',(-7.76135515938823,-1.53160959859086,
114.711238915955));
#56834=CARTESIAN_POINT('Ctrl Pts',(-7.7670102646236,-1.50250239357352,114.710045544368));
#56835=CARTESIAN_POINT('Ctrl Pts',(-7.76822226070017,-1.49622351317799,
114.709787753039));
#56836=CARTESIAN_POINT('Ctrl Pts',(-7.77015172419558,-1.48616217311393,
114.709374075768));
#56837=CARTESIAN_POINT('Ctrl Pts',(-7.77087404800033,-1.48238063662222,
114.709218462483));
#56838=CARTESIAN_POINT('Ctrl Pts',(-7.77217188291264,-1.47555914656806,
114.70893750969));
#56839=CARTESIAN_POINT('Ctrl Pts',(-7.77274837022012,-1.47251938720994,
114.708812225698));
#56840=CARTESIAN_POINT('Ctrl Pts',(-7.77411234721491,-1.46530415531789,
114.708514642878));
#56841=CARTESIAN_POINT('Ctrl Pts',(-7.77489825510597,-1.46112839180911,
114.708342255209));
#56842=CARTESIAN_POINT('Ctrl Pts',(-7.77687603994566,-1.45057305192077,
114.707906089931));
#56843=CARTESIAN_POINT('Ctrl Pts',(-7.778063429352,-1.4441926492463,114.707642061916));
#56844=CARTESIAN_POINT('Ctrl Pts',(-7.78439794848421,-1.40991987635502,
114.706221812726));
#56845=CARTESIAN_POINT('Ctrl Pts',(-7.78940284152846,-1.38200174138548,
114.705057769813));
#56846=CARTESIAN_POINT('Ctrl Pts',(-7.87156588342275,-0.909052962050528,
114.685225000803));
#56847=CARTESIAN_POINT('Ctrl Pts',(-7.91061575441299,-0.458278575113945,
114.66466740998));
#56848=CARTESIAN_POINT('Ctrl Pts',(-7.91150122343188,0.590095865630536,
114.616562902213));
#56849=CARTESIAN_POINT('Ctrl Pts',(-7.84447459963245,1.18509353893569,114.589167834301));
#56850=CARTESIAN_POINT('Ctrl Pts',(-7.70010911675395,1.81512687398723,114.561755470135));
#56851=CARTESIAN_POINT('Ctrl Pts',(-7.68861338522194,1.86322041220235,114.559671826483));
#56852=CARTESIAN_POINT('Ctrl Pts',(-7.64589242441081,2.03481626361016,114.552269593527));
#56853=CARTESIAN_POINT('Ctrl Pts',(-7.61213546433998,2.15767092858362,114.547030092214));
#56854=CARTESIAN_POINT('Ctrl Pts',(-7.57042389038027,2.29628054693532,114.54118470337));
#56855=CARTESIAN_POINT('Ctrl Pts',(-7.56536783001319,2.31288387772137,114.540485592137));
#56856=CARTESIAN_POINT('Ctrl Pts',(-7.55789748460164,2.33712875749698,114.539466276754));
#56857=CARTESIAN_POINT('Ctrl Pts',(-7.5555261800531,2.34478343560438,114.539144682096));
#56858=CARTESIAN_POINT('Ctrl Pts',(-7.55130656431015,2.35833168189141,114.538575881687));
#56859=CARTESIAN_POINT('Ctrl Pts',(-7.54946297603595,2.36422670733805,114.538328523085));
#56860=CARTESIAN_POINT('Ctrl Pts',(-7.5456236437485,2.37645300705303,114.53781577755));
#56861=CARTESIAN_POINT('Ctrl Pts',(-7.54362683028941,2.38278394182943,114.537550425565));
#56862=CARTESIAN_POINT('Ctrl Pts',(-7.53846692518996,2.39907202213077,114.536868128858));
#56863=CARTESIAN_POINT('Ctrl Pts',(-7.53529206906851,2.40902544288219,114.536451566715));
#56864=CARTESIAN_POINT('Ctrl Pts',(-7.52205182381373,2.45025237509161,114.534727731417));
#56865=CARTESIAN_POINT('Ctrl Pts',(-7.51181132248268,2.4814695303517,114.533426162941));
#56866=CARTESIAN_POINT('Ctrl Pts',(-7.30846560723666,3.08855354275673,114.508184421553));
#56867=CARTESIAN_POINT('Ctrl Pts',(-7.04987682696602,3.6403513549266,114.486697291546));
#56868=CARTESIAN_POINT('Ctrl Pts',(-6.40509552785112,4.68428372647476,114.444421976861));
#56869=CARTESIAN_POINT('Ctrl Pts',(-6.01877404344938,5.17126004935686,114.423725553408));
#56870=CARTESIAN_POINT('Ctrl Pts',(-5.57435211485233,5.61342819134297,114.399027162713));
#56871=CARTESIAN_POINT('Ctrl Pts',(-5.56901318660006,5.61872491643253,114.398730325039));
#56872=CARTESIAN_POINT('Ctrl Pts',(-5.54079458777866,5.64664072163285,114.397160665173));
#56873=CARTESIAN_POINT('Ctrl Pts',(-5.51778492817767,5.6691274051102,114.395878185609));
#56874=CARTESIAN_POINT('Ctrl Pts',(-5.48982104367894,5.69612418727276,114.394315581653));
#56875=CARTESIAN_POINT('Ctrl Pts',(-5.4849971500352,5.70076943158283,114.394045883204));
#56876=CARTESIAN_POINT('Ctrl Pts',(-5.4770922277948,5.70836227909637,114.393603684081));
#56877=CARTESIAN_POINT('Ctrl Pts',(-5.47401469704151,5.71131353347008,114.393431467554));
#56878=CARTESIAN_POINT('Ctrl Pts',(-5.46850207577078,5.71659141361181,114.393122873989));
#56879=CARTESIAN_POINT('Ctrl Pts',(-5.46606788056069,5.71891897721289,114.392986570383));
#56880=CARTESIAN_POINT('Ctrl Pts',(-5.46091332779494,5.7238414338761,114.392697855796));
#56881=CARTESIAN_POINT('Ctrl Pts',(-5.45819260626598,5.72643594277061,114.39254541471));
#56882=CARTESIAN_POINT('Ctrl Pts',(-5.45093435159827,5.73334761912903,114.392138602921));
#56883=CARTESIAN_POINT('Ctrl Pts',(-5.44639357780424,5.73766130248945,114.391883959673));
#56884=CARTESIAN_POINT('Ctrl Pts',(-5.42448668206845,5.75842316618419,114.390654767073));
#56885=CARTESIAN_POINT('Ctrl Pts',(-5.40705132218461,5.77479775406727,114.389674457737));
#56886=CARTESIAN_POINT('Ctrl Pts',(-5.26623745052928,5.90584768139919,114.381743177298));
#56887=CARTESIAN_POINT('Ctrl Pts',(-5.13930613276481,6.01662857498759,114.374508597872));
#56888=CARTESIAN_POINT('Ctrl Pts',(-4.86460079320475,6.24134256698503,114.3588669934));
#56889=CARTESIAN_POINT('Ctrl Pts',(-4.71613239345001,6.35427320065368,114.350422629969));
#56890=CARTESIAN_POINT('Ctrl Pts',(-4.43257918872856,6.55453875103664,114.334515246114));
#56891=CARTESIAN_POINT('Ctrl Pts',(-4.29854723023253,6.64320910692246,114.327081486576));
#56892=CARTESIAN_POINT('Ctrl Pts',(-3.87428048504851,6.90566887179359,114.303992480968));
#56893=CARTESIAN_POINT('Ctrl Pts',(-3.5755236402543,7.06498142123424,114.288369901359));
#56894=CARTESIAN_POINT('Ctrl Pts',(-2.9134483279361,7.36524643234313,114.255847807305));
#56895=CARTESIAN_POINT('Ctrl Pts',(-2.54804195562352,7.49950503779965,114.239161662206));
#56896=CARTESIAN_POINT('Ctrl Pts',(-2.15008285076706,7.61325778860508,114.222400886701));
#56897=CARTESIAN_POINT('Ctrl Pts',(-2.12592787847292,7.62003812930556,114.221388781452));
#56898=CARTESIAN_POINT('Ctrl Pts',(-2.09258626203811,7.62922629812788,114.21999888458));
#56899=CARTESIAN_POINT('Ctrl Pts',(-2.08342705887356,7.63173262525021,114.219617809274));
#56900=CARTESIAN_POINT('Ctrl Pts',(-2.06882576587508,7.63569988281892,114.219011486479));
#56901=CARTESIAN_POINT('Ctrl Pts',(-2.0633866037437,7.63717149694125,114.218785883176));
#56902=CARTESIAN_POINT('Ctrl Pts',(-2.05279813065841,7.64002416601828,114.218347202487));
#56903=CARTESIAN_POINT('Ctrl Pts',(-2.04764898697989,7.64140582935227,114.218134104919));
#56904=CARTESIAN_POINT('Ctrl Pts',(-2.03532496956186,7.64469936637174,114.217624627555));
#56905=CARTESIAN_POINT('Ctrl Pts',(-2.0281487872562,7.64660634733251,114.217328410688));
#56906=CARTESIAN_POINT('Ctrl Pts',(-2.00661116098096,7.65229725096662,114.216440724345));
#56907=CARTESIAN_POINT('Ctrl Pts',(-1.99224169792055,7.65605084810427,114.215850263146));
#56908=CARTESIAN_POINT('Ctrl Pts',(-1.86690511802338,7.68841456343842,114.210715446017));
#56909=CARTESIAN_POINT('Ctrl Pts',(-1.75533649285171,7.71465154167654,114.206250352622));
#56910=CARTESIAN_POINT('Ctrl Pts',(-1.33983526939512,7.80288177173758,114.189981967903));
#56911=CARTESIAN_POINT('Ctrl Pts',(-1.03289807400134,7.84941168923707,114.178686900753));
#56912=CARTESIAN_POINT('Ctrl Pts',(0.0588799863000562,7.94975086287487,
114.140011739207));
#56913=CARTESIAN_POINT('Ctrl Pts',(0.847967369154513,7.90459197026372,114.115144751372));
#56914=CARTESIAN_POINT('Ctrl Pts',(1.68431394085534,7.7299219381343,114.082019335349));
#56915=CARTESIAN_POINT('Ctrl Pts',(1.7511335334382,7.71505913495567,114.079321329593));
#56916=CARTESIAN_POINT('Ctrl Pts',(1.82678330603892,7.69719883478677,114.076199620795));
#56917=CARTESIAN_POINT('Ctrl Pts',(1.83581283990184,7.69505025096701,114.075825923681));
#56918=CARTESIAN_POINT('Ctrl Pts',(1.84899686870546,7.69188857600627,114.075278666567));
#56919=CARTESIAN_POINT('Ctrl Pts',(1.85315438556888,7.69088799224674,114.075105856044));
#56920=CARTESIAN_POINT('Ctrl Pts',(1.86051047390233,7.68911130168749,114.074799673773));
#56921=CARTESIAN_POINT('Ctrl Pts',(1.86370937934513,7.68833656797847,114.074666384998));
#56922=CARTESIAN_POINT('Ctrl Pts',(1.87035243493749,7.68672331585019,114.074389294576));
#56923=CARTESIAN_POINT('Ctrl Pts',(1.87379649371323,7.68588448165218,114.074245473806));
#56924=CARTESIAN_POINT('Ctrl Pts',(1.88274041433374,7.68369973334673,114.073871557327));
#56925=CARTESIAN_POINT('Ctrl Pts',(1.88823938672965,7.68235023141181,114.073641244299));
#56926=CARTESIAN_POINT('Ctrl Pts',(1.91171013888337,7.67656355530988,114.072656447187));
#56927=CARTESIAN_POINT('Ctrl Pts',(1.92966763024812,7.67206924495204,114.071898537022));
#56928=CARTESIAN_POINT('Ctrl Pts',(2.05449275917079,7.6403626693165,114.066600103834));
#56929=CARTESIAN_POINT('Ctrl Pts',(2.16079255226994,7.6109825667969,114.061934455314));
#56930=CARTESIAN_POINT('Ctrl Pts',(2.50380509418856,7.50841274039745,114.046458814773));
#56931=CARTESIAN_POINT('Ctrl Pts',(2.73769287654617,7.4263264640513,114.035251988419));
#56932=CARTESIAN_POINT('Ctrl Pts',(3.15479090092532,7.25755546955799,114.014527643675));
#56933=CARTESIAN_POINT('Ctrl Pts',(3.33927393124967,7.17454281985285,114.005084804466));
#56934=CARTESIAN_POINT('Ctrl Pts',(3.89376392774937,6.8990123644565,113.976192124441));
#56935=CARTESIAN_POINT('Ctrl Pts',(4.25192966638275,6.68422848173635,113.956845897423));
#56936=CARTESIAN_POINT('Ctrl Pts',(4.8626118366503,6.24898031886751,113.9236344417));
#56937=CARTESIAN_POINT('Ctrl Pts',(5.1212611733734,6.03883013881877,113.909473258998));
#56938=CARTESIAN_POINT('Ctrl Pts',(5.3822513094109,5.79791218556196,113.895093966686));
#56939=CARTESIAN_POINT('Ctrl Pts',(5.39851734326731,5.78276969750192,113.894197294112));
#56940=CARTESIAN_POINT('Ctrl Pts',(5.42066801867198,5.76197412397302,113.892975501419));
#56941=CARTESIAN_POINT('Ctrl Pts',(5.4266079614961,5.75638025209686,113.892647792545));
#56942=CARTESIAN_POINT('Ctrl Pts',(5.43670604587886,5.74684097801868,113.892090551353));
#56943=CARTESIAN_POINT('Ctrl Pts',(5.44086856724014,5.74290023334393,113.891860814908));
#56944=CARTESIAN_POINT('Ctrl Pts',(5.44919961476439,5.73499587141712,113.891400935756));
#56945=CARTESIAN_POINT('Ctrl Pts',(5.4533681084395,5.73103222471857,113.891170794579));
#56946=CARTESIAN_POINT('Ctrl Pts',(5.46289314610155,5.72195546213095,113.890644832419));
#56947=CARTESIAN_POINT('Ctrl Pts',(5.46824684495901,5.71683936098624,113.890349143244));
#56948=CARTESIAN_POINT('Ctrl Pts',(5.48425334796483,5.70150017175247,113.889464894832));
#56949=CARTESIAN_POINT('Ctrl Pts',(5.49488475173091,5.69125474402982,113.888877322696));
#56950=CARTESIAN_POINT('Ctrl Pts',(5.51903674805535,5.66784883122372,113.887541872946));
#56951=CARTESIAN_POINT('Ctrl Pts',(5.53253908791069,5.65466959663575,113.886794829965));
#56952=CARTESIAN_POINT('Ctrl Pts',(5.65164444441297,5.53757939112244,113.88020081793));
#56953=CARTESIAN_POINT('Ctrl Pts',(5.75435917667658,5.43076640795265,113.874485146649));
#56954=CARTESIAN_POINT('Ctrl Pts',(6.02854405522238,5.12912303299153,113.859088550451));
#56955=CARTESIAN_POINT('Ctrl Pts',(6.19352483388177,4.92864156006523,113.84966904665));
#56956=CARTESIAN_POINT('Ctrl Pts',(6.82867221923104,4.07444695933599,113.811984482845));
#56957=CARTESIAN_POINT('Ctrl Pts',(7.20749988035636,3.35908245583782,113.786347561572));
#56958=CARTESIAN_POINT('Ctrl Pts',(7.4870047275012,2.55554329361777,113.752919138255));
#56959=CARTESIAN_POINT('Ctrl Pts',(7.50175231976099,2.5119222201467,113.751089566115));
#56960=CARTESIAN_POINT('Ctrl Pts',(7.51890708148125,2.45968234143464,113.748882736262));
#56961=CARTESIAN_POINT('Ctrl Pts',(7.52168183986271,2.45118404441712,113.74852323687));
#56962=CARTESIAN_POINT('Ctrl Pts',(7.52616685384855,2.43736839383444,113.747938014027));
#56963=CARTESIAN_POINT('Ctrl Pts',(7.52788589874087,2.43205388396971,113.74771270577));
#56964=CARTESIAN_POINT('Ctrl Pts',(7.53093099026241,2.422605676911,113.747311819562));
#56965=CARTESIAN_POINT('Ctrl Pts',(7.53225926684657,2.41847269630847,113.747136345548));
#56966=CARTESIAN_POINT('Ctrl Pts',(7.53504121021527,2.4097920563301,113.746767558863));
#56967=CARTESIAN_POINT('Ctrl Pts',(7.53649416312275,2.40524417127762,113.746574213396));
#56968=CARTESIAN_POINT('Ctrl Pts',(7.54029525891965,2.39330910927881,113.746066468241));
#56969=CARTESIAN_POINT('Ctrl Pts',(7.54263665943547,2.38591980321354,113.74575176189));
#56970=CARTESIAN_POINT('Ctrl Pts',(7.55292174158578,2.35329431502966,113.744360758988));
#56971=CARTESIAN_POINT('Ctrl Pts',(7.56074959699998,2.32802200922963,113.743279299989));
#56972=CARTESIAN_POINT('Ctrl Pts',(7.75756735472088,1.68112999105057,113.715503962785));
#56973=CARTESIAN_POINT('Ctrl Pts',(7.86938896930225,1.03863170025377,113.685944336042));
#56974=CARTESIAN_POINT('Ctrl Pts',(7.92641764586476,-0.117614165030195,
113.635016451404));
#56975=CARTESIAN_POINT('Ctrl Pts',(7.90252346158347,-0.62620806724524,113.613344034359));
#56976=CARTESIAN_POINT('Ctrl Pts',(7.82518086677541,-1.16258964015839,113.591379570098));
#56977=CARTESIAN_POINT('Ctrl Pts',(7.82012697233585,-1.19611221478048,113.590010111831));
#56978=CARTESIAN_POINT('Ctrl Pts',(7.81288533224873,-1.24213719873356,113.588134155333));
#56979=CARTESIAN_POINT('Ctrl Pts',(7.81088277490538,-1.25466820845354,113.587623830588));
#56980=CARTESIAN_POINT('Ctrl Pts',(7.80727400160041,-1.27690660402853,113.586718924017));
#56981=CARTESIAN_POINT('Ctrl Pts',(7.80567981208698,-1.28661590354036,113.586324095544));
#56982=CARTESIAN_POINT('Ctrl Pts',(7.80251173316728,-1.30568824637023,113.58554900914));
#56983=CARTESIAN_POINT('Ctrl Pts',(7.8009390932224,-1.31505148467227,113.585168725657));
#56984=CARTESIAN_POINT('Ctrl Pts',(7.79723441097925,-1.33686804520771,113.584283193993));
#56985=CARTESIAN_POINT('Ctrl Pts',(7.79508938154828,-1.34931914867162,113.583778213904));
#56986=CARTESIAN_POINT('Ctrl Pts',(7.78813676358106,-1.38910659673721,113.582165850738));
#56987=CARTESIAN_POINT('Ctrl Pts',(7.78321511944348,-1.41642288989412,113.581060835815));
#56988=CARTESIAN_POINT('Ctrl Pts',(7.66678450436959,-2.04370467583689,113.55572993481));
#56989=CARTESIAN_POINT('Ctrl Pts',(7.4863738679513,-2.62879948481135,113.533259426344));
#56990=CARTESIAN_POINT('Ctrl Pts',(7.06392079686754,-3.58845200226038,113.495310003127));
#56991=CARTESIAN_POINT('Ctrl Pts',(6.85434488320203,-3.97415172240473,113.479643838835));
#56992=CARTESIAN_POINT('Ctrl Pts',(6.53959894218909,-4.4537534603533,113.457727623592));
#56993=CARTESIAN_POINT('Ctrl Pts',(6.46237452036348,-4.56508347149693,113.452449317373));
#56994=CARTESIAN_POINT('Ctrl Pts',(6.3742674321451,-4.68538387186075,113.446476530752));
#56995=CARTESIAN_POINT('Ctrl Pts',(6.36617359083058,-4.69637531840089,113.445928285819));
#56996=CARTESIAN_POINT('Ctrl Pts',(6.35484678790306,-4.71167404498058,113.445161586739));
#56997=CARTESIAN_POINT('Ctrl Pts',(6.35163778310411,-4.71599909625832,113.444944432054));
#56998=CARTESIAN_POINT('Ctrl Pts',(6.3460182225041,-4.72355692050891,113.444564252095));
#56999=CARTESIAN_POINT('Ctrl Pts',(6.34360960439008,-4.72679113655732,113.444401333316));
#57000=CARTESIAN_POINT('Ctrl Pts',(6.33855057286811,-4.73357341219581,113.444059203664));
#57001=CARTESIAN_POINT('Ctrl Pts',(6.33589965165436,-4.73712108959628,113.443879964625));
#57002=CARTESIAN_POINT('Ctrl Pts',(6.32957316061572,-4.74557290164447,113.443452287811));
#57003=CARTESIAN_POINT('Ctrl Pts',(6.32589487201399,-4.75047498975805,113.44320369758));
#57004=CARTESIAN_POINT('Ctrl Pts',(6.31350720015219,-4.76694425043252,113.442366704036));
#57005=CARTESIAN_POINT('Ctrl Pts',(6.30477179427587,-4.77849173598575,113.441776820024));
#57006=CARTESIAN_POINT('Ctrl Pts',(6.08666405560422,-5.06517295359002,113.427055254306));
#57007=CARTESIAN_POINT('Ctrl Pts',(5.85955233316282,-5.32625656427809,113.411753347226));
#57008=CARTESIAN_POINT('Ctrl Pts',(5.39869151786496,-5.79080179627688,113.381995723101));
#57009=CARTESIAN_POINT('Ctrl Pts',(5.16858957679347,-5.99707730297325,113.367662346137));
#57010=CARTESIAN_POINT('Ctrl Pts',(4.58845575924935,-6.45889000144918,113.333622188026));
#57011=CARTESIAN_POINT('Ctrl Pts',(4.22831924378883,-6.70019168064386,113.314157838926));
#57012=CARTESIAN_POINT('Ctrl Pts',(3.69616826818806,-6.9966677571959,113.288276197032));
#57013=CARTESIAN_POINT('Ctrl Pts',(3.53928302775982,-7.07732298161823,113.280961283663));
#57014=CARTESIAN_POINT('Ctrl Pts',(3.36468926893079,-7.15982313962474,113.273157454912));
#57015=CARTESIAN_POINT('Ctrl Pts',(3.34953012987038,-7.16692745748346,113.272482597376));
#57016=CARTESIAN_POINT('Ctrl Pts',(3.32704583357555,-7.17737778512299,113.271485630024));
#57017=CARTESIAN_POINT('Ctrl Pts',(3.31973798389758,-7.18076079310896,113.271162218404));
#57018=CARTESIAN_POINT('Ctrl Pts',(3.30724600029924,-7.18652053620013,113.270610441837));
#57019=CARTESIAN_POINT('Ctrl Pts',(3.30206444543268,-7.18890283159546,113.270381881455));
#57020=CARTESIAN_POINT('Ctrl Pts',(3.29167140158531,-7.19366757777455,113.269924062897));
#57021=CARTESIAN_POINT('Ctrl Pts',(3.28645989090551,-7.19604997350592,113.269694806739));
#57022=CARTESIAN_POINT('Ctrl Pts',(3.27445417039002,-7.20152251931124,113.269167390882));
#57023=CARTESIAN_POINT('Ctrl Pts',(3.26765816165978,-7.20460872282955,113.268869369869));
#57024=CARTESIAN_POINT('Ctrl Pts',(3.24816418322325,-7.21342807170229,113.268016028233));
#57025=CARTESIAN_POINT('Ctrl Pts',(3.23545539294149,-7.21913731062699,113.267461546307));
#57026=CARTESIAN_POINT('Ctrl Pts',(3.20609059306456,-7.23223590117682,113.266184588281));
#57027=CARTESIAN_POINT('Ctrl Pts',(3.18942397469236,-7.23960135205334,113.265462949212));
#57028=CARTESIAN_POINT('Ctrl Pts',(3.13593070440558,-7.26302096518825,113.263156703382));
#57029=CARTESIAN_POINT('Ctrl Pts',(3.09900689494922,-7.27885233053718,113.261579857334));
#57030=CARTESIAN_POINT('Ctrl Pts',(2.95584546753655,-7.33894705868507,113.255522971119));
#57031=CARTESIAN_POINT('Ctrl Pts',(2.84876536721906,-7.38117223719992,113.251113276011));
#57032=CARTESIAN_POINT('Ctrl Pts',(2.49948272882219,-7.5101720318603,113.237087251311));
#57033=CARTESIAN_POINT('Ctrl Pts',(2.2539543452568,-7.58747646056536,113.227781532307));
#57034=CARTESIAN_POINT('Ctrl Pts',(1.17205725711898,-7.87094498829714,113.188429609568));
#57035=CARTESIAN_POINT('Ctrl Pts',(0.30916061301062,-7.95169086946019,113.161798096139));
#57036=CARTESIAN_POINT('Ctrl Pts',(-0.595606776303615,-7.88868179284596,
113.126216452307));
#57037=CARTESIAN_POINT('Ctrl Pts',(-0.641583470141476,-7.88507567170836,
113.124385924291));
#57038=CARTESIAN_POINT('Ctrl Pts',(-0.695584827526059,-7.88036472512556,
113.122206944979));
#57039=CARTESIAN_POINT('Ctrl Pts',(-0.703643425308883,-7.87964925503474,
113.12188101817));
#57040=CARTESIAN_POINT('Ctrl Pts',(-0.715810113849971,-7.87855024128623,
113.121387777422));
#57041=CARTESIAN_POINT('Ctrl Pts',(-0.719919046565194,-7.87817584151481,
113.121220999717));
#57042=CARTESIAN_POINT('Ctrl Pts',(-0.727272001827565,-7.87750005077193,
113.120922188529));
#57043=CARTESIAN_POINT('Ctrl Pts',(-0.730516131327986,-7.87719987027768,
113.120790226636));
#57044=CARTESIAN_POINT('Ctrl Pts',(-0.737411737973479,-7.87655752084076,
113.120509466215));
#57045=CARTESIAN_POINT('Ctrl Pts',(-0.74106316604755,-7.87621481641108,
113.120360636165));
#57046=CARTESIAN_POINT('Ctrl Pts',(-0.750838307265465,-7.8752905136588,
113.119961783876));
#57047=CARTESIAN_POINT('Ctrl Pts',(-0.756961571848057,-7.87470431295756,
113.119711493232));
#57048=CARTESIAN_POINT('Ctrl Pts',(-0.785993051777178,-7.87189085735959,
113.118522733498));
#57049=CARTESIAN_POINT('Ctrl Pts',(-0.80889194799356,-7.86957079788246,
113.117578922005));
#57050=CARTESIAN_POINT('Ctrl Pts',(-0.988510200437143,-7.85058007281931,
113.110129193246));
#57051=CARTESIAN_POINT('Ctrl Pts',(-1.14470153439236,-7.82933027936056,
113.103373570541));
#57052=CARTESIAN_POINT('Ctrl Pts',(-1.542930816378,-7.76298055049504,113.08562738993));
#57053=CARTESIAN_POINT('Ctrl Pts',(-1.78368706416445,-7.71122248394325,
113.074402377143));
#57054=CARTESIAN_POINT('Ctrl Pts',(-2.31499858640699,-7.57078482436854,
113.049067791044));
#57055=CARTESIAN_POINT('Ctrl Pts',(-2.60367181645543,-7.47642290844188,
113.034921593991));
#57056=CARTESIAN_POINT('Ctrl Pts',(-3.05455905556037,-7.29974537617735,
113.012742248698));
#57057=CARTESIAN_POINT('Ctrl Pts',(-3.22060071417901,-7.22802522629254,
113.004552534517));
#57058=CARTESIAN_POINT('Ctrl Pts',(-3.70784019814695,-6.99744005022162,
112.980579426672));
#57059=CARTESIAN_POINT('Ctrl Pts',(-4.02087626336123,-6.82237828610346,
112.965279104118));
#57060=CARTESIAN_POINT('Ctrl Pts',(-4.34117711907326,-6.61352270456729,
112.949800663924));
#57061=CARTESIAN_POINT('Ctrl Pts',(-4.3612963721988,-6.60027236639864,112.94882905397));
#57062=CARTESIAN_POINT('Ctrl Pts',(-4.38835059883131,-6.58227700831028,
112.947523357466));
#57063=CARTESIAN_POINT('Ctrl Pts',(-4.39533888667246,-6.57761261129523,
112.947186161516));
#57064=CARTESIAN_POINT('Ctrl Pts',(-4.40711457031713,-6.56972567673556,
112.946618088214));
#57065=CARTESIAN_POINT('Ctrl Pts',(-4.41190588733069,-6.56650902268415,
112.946386983429));
#57066=CARTESIAN_POINT('Ctrl Pts',(-4.4214747627516,-6.56006975058397,112.94592550455));
#57067=CARTESIAN_POINT('Ctrl Pts',(-4.42625232816286,-6.55684714918671,
112.945695130024));
#57068=CARTESIAN_POINT('Ctrl Pts',(-4.43698240846079,-6.54959233830433,
112.945177798636));
#57069=CARTESIAN_POINT('Ctrl Pts',(-4.44293296007714,-6.54555722636256,
112.944890954718));
#57070=CARTESIAN_POINT('Ctrl Pts',(-4.45531895069065,-6.53713352486124,
112.944293996935));
#57071=CARTESIAN_POINT('Ctrl Pts',(-4.46175342713752,-6.53274353010524,
112.943983938132));
#57072=CARTESIAN_POINT('Ctrl Pts',(-4.47844544623616,-6.52131904492611,
112.943179745593));
#57073=CARTESIAN_POINT('Ctrl Pts',(-4.48869291986336,-6.51426984194363,
112.942686185144));
#57074=CARTESIAN_POINT('Ctrl Pts',(-4.51871576048691,-6.49351275071951,
112.941240565419));
#57075=CARTESIAN_POINT('Ctrl Pts',(-4.53844534209447,-6.47973871834073,
112.940291089055));
#57076=CARTESIAN_POINT('Ctrl Pts',(-4.60590931666847,-6.43218005786104,
112.937045983586));
#57077=CARTESIAN_POINT('Ctrl Pts',(-4.65333226732243,-6.39795591778388,
112.934767598431));
#57078=CARTESIAN_POINT('Ctrl Pts',(-4.82168783247279,-6.27359510542896,
112.926685149101));
#57079=CARTESIAN_POINT('Ctrl Pts',(-4.94041929840592,-6.18052822270472,
112.920997108455));
#57080=CARTESIAN_POINT('Ctrl Pts',(-5.20538048682271,-5.96032294486073,
112.908272664376));
#57081=CARTESIAN_POINT('Ctrl Pts',(-5.34974655763972,-5.83109353661543,
112.901317619394));
#57082=CARTESIAN_POINT('Ctrl Pts',(-6.05050445451427,-5.15585597485429,
112.867037859177));
#57083=CARTESIAN_POINT('Ctrl Pts',(-6.52867205715385,-4.53514374839793,
112.842325521851));
#57084=CARTESIAN_POINT('Ctrl Pts',(-6.94081453738616,-3.79650555720081,
112.809519852572));
#57085=CARTESIAN_POINT('Ctrl Pts',(-6.97254440708817,-3.73791183799385,
112.806893877122));
#57086=CARTESIAN_POINT('Ctrl Pts',(-7.00782656225619,-3.67074559937355,
112.803849158977));
#57087=CARTESIAN_POINT('Ctrl Pts',(-7.01210928499735,-3.66255781606667,
112.803477418164));
#57088=CARTESIAN_POINT('Ctrl Pts',(-7.01837268125978,-3.65053209268946,
112.802930550645));
#57089=CARTESIAN_POINT('Ctrl Pts',(-7.02036458387028,-3.6466999824783,112.802756155788));
#57090=CARTESIAN_POINT('Ctrl Pts',(-7.02391148859713,-3.63986261416544,
112.802444765479));
#57091=CARTESIAN_POINT('Ctrl Pts',(-7.02546770404296,-3.63685798307104,
112.80230784829));
#57092=CARTESIAN_POINT('Ctrl Pts',(-7.02871769563886,-3.63057325816955,
112.802021297804));
#57093=CARTESIAN_POINT('Ctrl Pts',(-7.03041110411858,-3.62729297616298,
112.801871641044));
#57094=CARTESIAN_POINT('Ctrl Pts',(-7.0348175238976,-3.61874267378419,112.80148130938));
#57095=CARTESIAN_POINT('Ctrl Pts',(-7.03752690523141,-3.61347079570145,
112.801240404346));
#57096=CARTESIAN_POINT('Ctrl Pts',(-7.04917846290029,-3.59073653946237,
112.800200528583));
#57097=CARTESIAN_POINT('Ctrl Pts',(-7.058061521376,-3.57324410659505,112.799397861659));
#57098=CARTESIAN_POINT('Ctrl Pts',(-7.12023786558303,-3.44967058241966,
112.793710528407));
#57099=CARTESIAN_POINT('Ctrl Pts',(-7.17120023135378,-3.34243910032111,
112.788687452431));
#57100=CARTESIAN_POINT('Ctrl Pts',(-7.28510033603492,-3.08817172352702,
112.776645170133));
#57101=CARTESIAN_POINT('Ctrl Pts',(-7.34603010978106,-2.94029401555891,
112.769541268623));
#57102=CARTESIAN_POINT('Ctrl Pts',(-7.73854961810325,-1.89911352877953,
112.719321585755));
#57103=CARTESIAN_POINT('Ctrl Pts',(-7.91092258247302,-0.953821026728434,
112.673985643915));
#57104=CARTESIAN_POINT('Ctrl Pts',(-7.91099997392412,-0.000642317922101565,
112.635042636927));
#57105=CARTESIAN_POINT('',(-7.911,4.87276885507981E-12,110.642331508237));
#57106=CARTESIAN_POINT('Ctrl Pts',(-7.911,5.49282841433296E-12,112.642331508237));
#57107=CARTESIAN_POINT('Ctrl Pts',(-7.91099999999847,2.20167589667229,112.553744072504));
#57108=CARTESIAN_POINT('Ctrl Pts',(-6.94214576672064,4.38610418339171,112.465156636771));
#57109=CARTESIAN_POINT('Ctrl Pts',(-3.67820201487766,7.34180684107894,112.287981765306));
#57110=CARTESIAN_POINT('Ctrl Pts',(-1.40868175871167,8.08992666571438,112.199394329573));
#57111=CARTESIAN_POINT('Ctrl Pts',(2.97309270521825,7.65454228025044,112.022219458108));
#57112=CARTESIAN_POINT('Ctrl Pts',(5.05102072676072,6.4744488083386,111.933632022375));
#57113=CARTESIAN_POINT('Ctrl Pts',(7.66951518848087,2.93425195367147,111.75645715091));
#57114=CARTESIAN_POINT('Ctrl Pts',(8.18956872247117,0.60188196009315,111.667869715177));
#57115=CARTESIAN_POINT('Ctrl Pts',(7.32306689761068,-3.71537198232993,111.490694843711));
#57116=CARTESIAN_POINT('Ctrl Pts',(5.9432995884978,-5.66643518936954,111.402107407979));
#57117=CARTESIAN_POINT('Ctrl Pts',(2.16154501637252,-7.92205913233161,111.224932536513));
#57118=CARTESIAN_POINT('Ctrl Pts',(-0.210816529306575,-8.20894963712987,
111.13634510078));
#57119=CARTESIAN_POINT('Ctrl Pts',(-4.42123908576965,-6.91982244717495,
110.959170229315));
#57120=CARTESIAN_POINT('Ctrl Pts',(-6.22631625634599,-5.35390358803044,
110.870582793582));
#57121=CARTESIAN_POINT('Ctrl Pts',(-7.65317280859649,-2.31334857513966,
110.735440741312));
#57122=CARTESIAN_POINT('Ctrl Pts',(-7.91100000000071,-1.15702837835991,
110.688886124774));
#57123=CARTESIAN_POINT('Ctrl Pts',(-7.911,4.87276885507981E-12,110.642331508237));
#57124=CARTESIAN_POINT('',(-7.91812613509609,-0.0016953829844947,108.642276941385));
#57125=CARTESIAN_POINT('Ctrl Pts',(-7.911,4.87276885507981E-12,110.642331508237));
#57126=CARTESIAN_POINT('Ctrl Pts',(-7.91099999999864,2.20167589667137,110.553744072504));
#57127=CARTESIAN_POINT('Ctrl Pts',(-6.94214576672126,4.38610418339058,110.465156636771));
#57128=CARTESIAN_POINT('Ctrl Pts',(-3.67820201487929,7.34180684107803,110.287981765306));
#57129=CARTESIAN_POINT('Ctrl Pts',(-1.40868175871384,8.08992666571392,110.199394329573));
#57130=CARTESIAN_POINT('Ctrl Pts',(2.97309270521562,7.65454228025138,110.022219458108));
#57131=CARTESIAN_POINT('Ctrl Pts',(5.05102072675818,6.47444880834048,109.933632022375));
#57132=CARTESIAN_POINT('Ctrl Pts',(7.66951518847946,2.93425195367492,109.75645715091));
#57133=CARTESIAN_POINT('Ctrl Pts',(8.18956872247078,0.601881960097223,109.667869715177));
#57134=CARTESIAN_POINT('Ctrl Pts',(7.32306689761272,-3.71537198232573,109.490694843712));
#57135=CARTESIAN_POINT('Ctrl Pts',(5.9432995885012,-5.66643518936585,109.402107407979));
#57136=CARTESIAN_POINT('Ctrl Pts',(2.1615450163779,-7.92205913233006,109.224932536513));
#57137=CARTESIAN_POINT('Ctrl Pts',(-0.210816529300619,-8.20894963712995,
109.136345100781));
#57138=CARTESIAN_POINT('Ctrl Pts',(-4.42123908576411,-6.9198224471784,108.959170229315));
#57139=CARTESIAN_POINT('Ctrl Pts',(-6.22631625634144,-5.35390358803561,
108.870582793583));
#57140=CARTESIAN_POINT('Ctrl Pts',(-7.65292805026068,-2.31387014206744,
108.73546392314));
#57141=CARTESIAN_POINT('Ctrl Pts',(-7.91074317242851,-1.15817992851268,
108.688932488431));
#57142=CARTESIAN_POINT('Ctrl Pts',(-7.91099980821568,-0.00172842309520182,
108.642401053722));
#57143=CARTESIAN_POINT('',(-7.90355940251074,-0.00222154607187651,106.642331508237));
#57144=CARTESIAN_POINT('Ctrl Pts',(-7.92321969856481,-0.00167176746646912,
108.642188231721));
#57145=CARTESIAN_POINT('Ctrl Pts',(-7.90990747858981,2.44136070272242,108.543454857439));
#57146=CARTESIAN_POINT('Ctrl Pts',(-5.38153242390624,7.53592095794861,108.338787103357));
#57147=CARTESIAN_POINT('Ctrl Pts',(3.28116688241203,8.75427127644514,108.028184969472));
#57148=CARTESIAN_POINT('Ctrl Pts',(9.14177665892542,1.98895403673894,107.710381830063));
#57149=CARTESIAN_POINT('Ctrl Pts',(6.61600493471317,-6.61592908789789,107.392578690655));
#57150=CARTESIAN_POINT('Ctrl Pts',(-0.534690503584316,-8.70980249966465,
107.12774274115));
#57151=CARTESIAN_POINT('Ctrl Pts',(-5.36923601473013,-6.22858863134672,
106.915873981543));
#57152=CARTESIAN_POINT('Ctrl Pts',(-7.52371069543634,-3.22405648818859,
106.771725967208));
#57153=CARTESIAN_POINT('Ctrl Pts',(-7.90357192039929,-0.955852324005775,
106.680545142771));
#57154=CARTESIAN_POINT('Ctrl Pts',(-7.89827895664709,-0.00379813367885562,
106.642331508237));
#57155=CARTESIAN_POINT('',(-7.9109999128679,0.00033058666535775,104.642331508237));
#57156=CARTESIAN_POINT('Ctrl Pts',(-7.911,4.53193038651989E-12,106.642331508237));
#57157=CARTESIAN_POINT('Ctrl Pts',(-7.91099999999874,2.20167589667133,106.553744072504));
#57158=CARTESIAN_POINT('Ctrl Pts',(-6.94214576672117,4.38610418339086,106.465156636771));
#57159=CARTESIAN_POINT('Ctrl Pts',(-3.67820201487855,7.34180684107849,106.287981765306));
#57160=CARTESIAN_POINT('Ctrl Pts',(-1.40868175871265,8.08992666571421,106.199394329573));
#57161=CARTESIAN_POINT('Ctrl Pts',(2.97309270521732,7.6545422802508,106.022219458108));
#57162=CARTESIAN_POINT('Ctrl Pts',(5.05102072675993,6.47444880833922,105.933632022375));
#57163=CARTESIAN_POINT('Ctrl Pts',(7.66951518848051,2.9342519536724,105.75645715091));
#57164=CARTESIAN_POINT('Ctrl Pts',(8.18956872247109,0.601881960094145,105.667869715177));
#57165=CARTESIAN_POINT('Ctrl Pts',(7.32306689761113,-3.71537198232904,105.490694843711));
#57166=CARTESIAN_POINT('Ctrl Pts',(5.94329958849849,-5.66643518936882,105.402107407979));
#57167=CARTESIAN_POINT('Ctrl Pts',(2.16154501637348,-7.92205913233135,105.224932536513));
#57168=CARTESIAN_POINT('Ctrl Pts',(-0.210816529305578,-8.2089496371299,
105.13634510078));
#57169=CARTESIAN_POINT('Ctrl Pts',(-4.42123908576881,-6.91982244717548,
104.959170229315));
#57170=CARTESIAN_POINT('Ctrl Pts',(-6.22631625634534,-5.35390358803119,
104.870582793582));
#57171=CARTESIAN_POINT('Ctrl Pts',(-7.65317280859634,-2.31334857514032,
104.735440741312));
#57172=CARTESIAN_POINT('Ctrl Pts',(-7.9110000000007,-1.15702837836027,104.688886124774));
#57173=CARTESIAN_POINT('Ctrl Pts',(-7.911,4.81115147721312E-12,104.642331508237));
#57174=CARTESIAN_POINT('',(-7.91099995190663,0.000872314928047417,102.642418784884));
#57175=CARTESIAN_POINT('Ctrl Pts',(-7.9109989008751,0.004170174215462,104.642331508237));
#57176=CARTESIAN_POINT('Ctrl Pts',(-7.91087854410085,0.232492124240155,
104.633166418883));
#57177=CARTESIAN_POINT('Ctrl Pts',(-7.9008690756303,0.460503234003182,104.624001329529));
#57178=CARTESIAN_POINT('Ctrl Pts',(-7.88107863799055,0.687401266953312,
104.614836240174));
#57179=CARTESIAN_POINT('Ctrl Pts',(-7.86178446149252,0.908609649227945,
104.605900972807));
#57180=CARTESIAN_POINT('Ctrl Pts',(-7.83319402724638,1.12875997869005,104.59696570544));
#57181=CARTESIAN_POINT('Ctrl Pts',(-7.79545881515053,1.34712392202496,104.588030438073));
#57182=CARTESIAN_POINT('Ctrl Pts',(-7.75626773479519,1.57391259961897,104.578750437725));
#57183=CARTESIAN_POINT('Ctrl Pts',(-7.70721240269764,1.79877409903119,104.569470437378));
#57184=CARTESIAN_POINT('Ctrl Pts',(-7.64851849464034,2.02091212999097,104.56019043703));
#57185=CARTESIAN_POINT('Ctrl Pts',(-7.58982458658305,2.24305016095075,104.550910436682));
#57186=CARTESIAN_POINT('Ctrl Pts',(-7.52149222134172,2.46246455165217,104.541630436334));
#57187=CARTESIAN_POINT('Ctrl Pts',(-7.44380231317566,2.67838162373487,104.532350435986));
#57188=CARTESIAN_POINT('Ctrl Pts',(-7.37757362925124,2.86244547267503,104.524439470143));
#57189=CARTESIAN_POINT('Ctrl Pts',(-7.30443025259769,3.04428369458642,104.5165285043));
#57190=CARTESIAN_POINT('Ctrl Pts',(-7.22454135979477,3.22334036996013,104.508617538457));
#57191=CARTESIAN_POINT('Ctrl Pts',(-7.14473330716828,3.40221585652622,104.50071457778));
#57192=CARTESIAN_POINT('Ctrl Pts',(-7.05819347429968,3.57831509117353,104.492811617103));
#57193=CARTESIAN_POINT('Ctrl Pts',(-6.96514037610916,3.75109857789608,104.484908656427));
#57194=CARTESIAN_POINT('Ctrl Pts',(-6.87216421850044,3.92373919928417,104.477012230281));
#57195=CARTESIAN_POINT('Ctrl Pts',(-6.77268568681204,4.09306923292176,104.469115804136));
#57196=CARTESIAN_POINT('Ctrl Pts',(-6.66697093203234,4.25857013461512,104.461219377991));
#57197=CARTESIAN_POINT('Ctrl Pts',(-6.56132402865668,4.42396481207731,104.453328020046));
#57198=CARTESIAN_POINT('Ctrl Pts',(-6.44944906193141,4.5855349650534,104.445436662101));
#57199=CARTESIAN_POINT('Ctrl Pts',(-6.33165769508611,4.742787348412,104.437545304157));
#57200=CARTESIAN_POINT('Ctrl Pts',(-6.21392014241337,4.8999678894351,104.429657551459));
#57201=CARTESIAN_POINT('Ctrl Pts',(-6.09027178201926,5.05283431658878,104.42176979876));
#57202=CARTESIAN_POINT('Ctrl Pts',(-5.96106726325917,5.20092281070387,104.413882046062));
#57203=CARTESIAN_POINT('Ctrl Pts',(-5.83189787679232,5.34897103774122,104.405996438141));
#57204=CARTESIAN_POINT('Ctrl Pts',(-5.69717556947778,5.49224366193245,104.398110830219));
#57205=CARTESIAN_POINT('Ctrl Pts',(-5.55729507127935,5.63031015937259,104.390225222298));
#57206=CARTESIAN_POINT('Ctrl Pts',(-5.41739807538984,5.76839294055817,104.382338684337));
#57207=CARTESIAN_POINT('Ctrl Pts',(-5.27234191345448,5.90126812124871,104.374452146377));
#57208=CARTESIAN_POINT('Ctrl Pts',(-5.12255840636323,6.02854181153266,104.366565608416));
#57209=CARTESIAN_POINT('Ctrl Pts',(-4.97275602938126,6.15583153589588,104.358678076901));
#57210=CARTESIAN_POINT('Ctrl Pts',(-4.81822538273729,6.27751813995468,104.350790545386));
#57211=CARTESIAN_POINT('Ctrl Pts',(-4.65943159300754,6.39324786240008,104.34290301387));
#57212=CARTESIAN_POINT('Ctrl Pts',(-4.50059118258624,6.50901156224285,104.335013166634));
#57213=CARTESIAN_POINT('Ctrl Pts',(-4.33748541328695,6.61881469235311,104.327123319397));
#57214=CARTESIAN_POINT('Ctrl Pts',(-4.17060881936156,6.72234654535628,104.31923347216));
#57215=CARTESIAN_POINT('Ctrl Pts',(-4.00365526062135,6.82592614807503,104.311339986063));
#57216=CARTESIAN_POINT('Ctrl Pts',(-3.83292770407638,6.92322852849717,104.303446499966));
#57217=CARTESIAN_POINT('Ctrl Pts',(-3.65894593145937,7.01398857075323,104.295553013869));
#57218=CARTESIAN_POINT('Ctrl Pts',(-3.48476303615417,7.10485353149244,104.287650402913));
#57219=CARTESIAN_POINT('Ctrl Pts',(-3.30731871620451,7.18916088826047,104.279747791957));
#57220=CARTESIAN_POINT('Ctrl Pts',(-3.12715447685737,7.26669291203852,104.271845181001));
#57221=CARTESIAN_POINT('Ctrl Pts',(-2.94687074276943,7.34427635927952,104.263937328603));
#57222=CARTESIAN_POINT('Ctrl Pts',(-2.76386381314278,7.41507539097209,104.256029476205));
#57223=CARTESIAN_POINT('Ctrl Pts',(-2.57869129941304,7.47892185962198,104.248121623806));
#57224=CARTESIAN_POINT('Ctrl Pts',(-2.39326541716374,7.54285568834986,104.240202951223));
#57225=CARTESIAN_POINT('Ctrl Pts',(-2.2056683607187,7.59981785305497,104.23228427864));
#57226=CARTESIAN_POINT('Ctrl Pts',(-2.01647003972864,7.64969081590078,104.224365606057));
#57227=CARTESIAN_POINT('Ctrl Pts',(-1.93827479305112,7.67030320089374,104.221092836231));
#57228=CARTESIAN_POINT('Ctrl Pts',(-1.85980611506728,7.68970525345834,104.217820066405));
#57229=CARTESIAN_POINT('Ctrl Pts',(-1.78110452738176,7.70789125912789,104.21454729658));
#57230=CARTESIAN_POINT('Ctrl Pts',(-1.59249761457652,7.75147368848496,104.206704163661));
#57231=CARTESIAN_POINT('Ctrl Pts',(-1.40199427875364,7.78819766795832,104.198861030742));
#57232=CARTESIAN_POINT('Ctrl Pts',(-1.21014031245643,7.81789494839678,104.191017897823));
#57233=CARTESIAN_POINT('Ctrl Pts',(-1.0185116582224,7.84755735254023,104.183183975829));
#57234=CARTESIAN_POINT('Ctrl Pts',(-0.825535875346164,7.87020943587607,
104.175350053835));
#57235=CARTESIAN_POINT('Ctrl Pts',(-0.63177296092783,7.8857329352344,104.167516131841));
#57236=CARTESIAN_POINT('Ctrl Pts',(-0.438199916876828,7.90124122294846,
104.159689886391));
#57237=CARTESIAN_POINT('Ctrl Pts',(-0.243841624972492,7.90963480966726,
104.151863640942));
#57238=CARTESIAN_POINT('Ctrl Pts',(-0.0492674952268234,7.9108465864226,
104.144037395492));
#57239=CARTESIAN_POINT('Ctrl Pts',(0.145153788286887,7.9120574112759,104.13621729789));
#57240=CARTESIAN_POINT('Ctrl Pts',(0.339790222195503,7.90609766032266,104.128397200289));
#57241=CARTESIAN_POINT('Ctrl Pts',(0.534067867171041,7.89295207848466,104.120577102687));
#57242=CARTESIAN_POINT('Ctrl Pts',(0.728230645011801,7.87981426900422,104.112761628737));
#57243=CARTESIAN_POINT('Ctrl Pts',(0.922034706765155,7.85949911554536,104.104946154787));
#57244=CARTESIAN_POINT('Ctrl Pts',(1.11490651313295,7.83204344133597,104.097130680837));
#57245=CARTESIAN_POINT('Ctrl Pts',(1.30770174640816,7.80459866745422,104.089318309752));
#57246=CARTESIAN_POINT('Ctrl Pts',(1.49956511415679,7.770019070504,104.081505938666));
#57247=CARTESIAN_POINT('Ctrl Pts',(1.68992840562266,7.72839329898975,104.07369356758));
#57248=CARTESIAN_POINT('Ctrl Pts',(1.88028449115895,7.68676910315943,104.06588149222));
#57249=CARTESIAN_POINT('Ctrl Pts',(2.06914026820764,7.63809933040576,104.058069416861));
#57250=CARTESIAN_POINT('Ctrl Pts',(2.25593746052766,7.58252379977722,104.050257341501));
#57251=CARTESIAN_POINT('Ctrl Pts',(2.44274011608328,7.52694664373765,104.042445037663));
#57252=CARTESIAN_POINT('Ctrl Pts',(2.62748372953017,7.46446342707425,104.034632733824));
#57253=CARTESIAN_POINT('Ctrl Pts',(2.80962497138708,7.39526392498322,104.026820429986));
#57254=CARTESIAN_POINT('Ctrl Pts',(2.99180358864167,7.32605022314871,104.019006523062));
#57255=CARTESIAN_POINT('Ctrl Pts',(3.17137844169123,7.25011761537827,104.011192616138));
#57256=CARTESIAN_POINT('Ctrl Pts',(3.34782583481584,7.16770417775033,104.003378709214));
#57257=CARTESIAN_POINT('Ctrl Pts',(3.52434048363695,7.08525932694565,103.995561823897));
#57258=CARTESIAN_POINT('Ctrl Pts',(3.69772497954674,6.99632887435923,103.98774493858));
#57259=CARTESIAN_POINT('Ctrl Pts',(3.8674797624686,6.90119709086009,103.979928053262));
#57260=CARTESIAN_POINT('Ctrl Pts',(4.03741869341718,6.80596210950162,103.972102688278));
#57261=CARTESIAN_POINT('Ctrl Pts',(4.20371974027894,6.70451253332006,103.964277323294));
#57262=CARTESIAN_POINT('Ctrl Pts',(4.36591101402899,6.59717682176098,103.95645195831));
#57263=CARTESIAN_POINT('Ctrl Pts',(4.52820086044954,6.48977587631181,103.948621837416));
#57264=CARTESIAN_POINT('Ctrl Pts',(4.68637567093829,6.37648187032801,103.940791716522));
#57265=CARTESIAN_POINT('Ctrl Pts',(4.83999620088008,6.25766392317983,103.932961595627));
#57266=CARTESIAN_POINT('Ctrl Pts',(4.99382671990661,6.13868355977139,103.925120771477));
#57267=CARTESIAN_POINT('Ctrl Pts',(5.1430902552499,6.01416439830458,103.917279947326));
#57268=CARTESIAN_POINT('Ctrl Pts',(5.28738318273056,5.88451358049058,103.909439123175));
#57269=CARTESIAN_POINT('Ctrl Pts',(5.3652573863346,5.81454165352118,103.905207467841));
#57270=CARTESIAN_POINT('Ctrl Pts',(5.44168446242181,5.74307562955914,103.900975812506));
#57271=CARTESIAN_POINT('Ctrl Pts',(5.51660584373181,5.67018350363585,103.896744157171));
#57272=CARTESIAN_POINT('Ctrl Pts',(5.65667304254243,5.53391004317758,103.888832982835));
#57273=CARTESIAN_POINT('Ctrl Pts',(5.79187609005824,5.39226033010117,103.880921808499));
#57274=CARTESIAN_POINT('Ctrl Pts',(5.92177708633773,5.24561503922328,103.873010634162));
#57275=CARTESIAN_POINT('Ctrl Pts',(6.05153725307177,5.09912873088015,103.865108036566));
#57276=CARTESIAN_POINT('Ctrl Pts',(6.17600659136928,4.94765788810591,103.85720543897));
#57277=CARTESIAN_POINT('Ctrl Pts',(6.29478226508762,4.79162156635292,103.849302841374));
#57278=CARTESIAN_POINT('Ctrl Pts',(6.41345121864179,4.63572544352578,103.841407344276));
#57279=CARTESIAN_POINT('Ctrl Pts',(6.52643649113257,4.47527228610266,103.833511847178));
#57280=CARTESIAN_POINT('Ctrl Pts',(6.63337375974589,4.31071613116831,103.825616350081));
#57281=CARTESIAN_POINT('Ctrl Pts',(6.74023478940494,4.14627729351104,103.817726481933));
#57282=CARTESIAN_POINT('Ctrl Pts',(6.84105621866451,3.97774157421741,103.809836613784));
#57283=CARTESIAN_POINT('Ctrl Pts',(6.93551535006845,3.80559428065642,103.801946745636));
#57284=CARTESIAN_POINT('Ctrl Pts',(7.02992466346148,3.63353777806103,103.794061038626));
#57285=CARTESIAN_POINT('Ctrl Pts',(7.11797819979438,3.45787379827077,103.786175331616));
#57286=CARTESIAN_POINT('Ctrl Pts',(7.19939763332376,3.27911492895449,103.778289624606));
#57287=CARTESIAN_POINT('Ctrl Pts',(7.28078922919831,3.1004171780652,103.770406613753));
#57288=CARTESIAN_POINT('Ctrl Pts',(7.3555511001764,2.91862696002967,103.762523602901));
#57289=CARTESIAN_POINT('Ctrl Pts',(7.42345164809672,2.73427991039142,103.754640592048));
#57290=CARTESIAN_POINT('Ctrl Pts',(7.49135320933112,2.5499301096493,103.746757463553));
#57291=CARTESIAN_POINT('Ctrl Pts',(7.55239311580177,2.36302372168847,103.738874335059));
#57292=CARTESIAN_POINT('Ctrl Pts',(7.60638835125973,2.17411527979089,103.730991206564));
#57293=CARTESIAN_POINT('Ctrl Pts',(7.66038692529708,1.98519515749554,103.723107590647));
#57294=CARTESIAN_POINT('Ctrl Pts',(7.70733986497832,1.79427306618492,103.715223974731));
#57295=CARTESIAN_POINT('Ctrl Pts',(7.74711436309768,1.60191761494953,103.707340358814));
#57296=CARTESIAN_POINT('Ctrl Pts',(7.78689800639556,1.40951793625629,103.699454930252));
#57297=CARTESIAN_POINT('Ctrl Pts',(7.81949984938443,1.21568457873006,103.69156950169));
#57298=CARTESIAN_POINT('Ctrl Pts',(7.84483838239496,1.02099547212648,103.683684073128));
#57299=CARTESIAN_POINT('Ctrl Pts',(7.87018700071214,0.826228874874966,103.675795505987));
#57300=CARTESIAN_POINT('Ctrl Pts',(7.88826650406258,0.630606191624877,103.667906938847));
#57301=CARTESIAN_POINT('Ctrl Pts',(7.89904730704057,0.434709835562825,103.660018371706));
#57302=CARTESIAN_POINT('Ctrl Pts',(7.90983958313647,0.238605003193925,103.652121409416));
#57303=CARTESIAN_POINT('Ctrl Pts',(7.91331762524989,0.0422262607709591,
103.644224447125));
#57304=CARTESIAN_POINT('Ctrl Pts',(7.90950397795936,-0.153843500496655,
103.636327484835));
#57305=CARTESIAN_POINT('Ctrl Pts',(7.90568800485134,-0.35003283823409,103.628425706448));
#57306=CARTESIAN_POINT('Ctrl Pts',(7.89457149619237,-0.545912475716475,
103.620523928061));
#57307=CARTESIAN_POINT('Ctrl Pts',(7.87622884207967,-0.740905005511776,
103.612622149674));
#57308=CARTESIAN_POINT('Ctrl Pts',(7.85786246458148,-0.936149727979011,
103.604710151559));
#57309=CARTESIAN_POINT('Ctrl Pts',(7.83225131902566,-1.1305047102084,103.596798153444));
#57310=CARTESIAN_POINT('Ctrl Pts',(7.79952102573957,-1.32340196805295,103.588886155329));
#57311=CARTESIAN_POINT('Ctrl Pts',(7.78580736940212,-1.40422393562269,103.585571109474));
#57312=CARTESIAN_POINT('Ctrl Pts',(7.77084453631388,-1.48479016593419,103.582256063619));
#57313=CARTESIAN_POINT('Ctrl Pts',(7.75464435836518,-1.56505970342194,103.578941017764));
#57314=CARTESIAN_POINT('Ctrl Pts',(7.71598356510864,-1.75661833959485,103.571029851427));
#57315=CARTESIAN_POINT('Ctrl Pts',(7.67016864698014,-1.94700105378001,103.56311868509));
#57316=CARTESIAN_POINT('Ctrl Pts',(7.6172823481017,-2.13563354283883,103.555207518754));
#57317=CARTESIAN_POINT('Ctrl Pts',(7.56445337629691,-2.32406156025142,103.547304927871));
#57318=CARTESIAN_POINT('Ctrl Pts',(7.50456838383806,-2.51074280242541,103.539402336988));
#57319=CARTESIAN_POINT('Ctrl Pts',(7.43776137105443,-2.69511164652793,103.531499746105));
#57320=CARTESIAN_POINT('Ctrl Pts',(7.37101437371167,-2.879314864643,103.523604254439));
#57321=CARTESIAN_POINT('Ctrl Pts',(7.29735786024608,-3.06120950073037,103.515708762773));
#57322=CARTESIAN_POINT('Ctrl Pts',(7.21697609892851,-3.24024335312868,103.507813271107));
#57323=CARTESIAN_POINT('Ctrl Pts',(7.13665163133336,-3.41914959553594,103.499923407112));
#57324=CARTESIAN_POINT('Ctrl Pts',(7.0496116069562,-3.59519880350818,103.492033543117));
#57325=CARTESIAN_POINT('Ctrl Pts',(6.95608912836604,-3.76785682294693,103.484143679123));
#57326=CARTESIAN_POINT('Ctrl Pts',(6.86261595870346,-3.94042380992051,103.476257974991));
#57327=CARTESIAN_POINT('Ctrl Pts',(6.76266730914396,-4.10960286866247,103.468372270859));
#57328=CARTESIAN_POINT('Ctrl Pts',(6.65652325060428,-4.27488236261124,103.460486566728));
#57329=CARTESIAN_POINT('Ctrl Pts',(6.55041546605112,-4.44010537345376,103.45260355748));
#57330=CARTESIAN_POINT('Ctrl Pts',(6.43811667836659,-4.60143118572496,103.444720548233));
#57331=CARTESIAN_POINT('Ctrl Pts',(6.31995164554021,-4.75837495349343,103.436837538985));
#57332=CARTESIAN_POINT('Ctrl Pts',(6.20178482075016,-4.91532110130211,103.428954410192));
#57333=CARTESIAN_POINT('Ctrl Pts',(6.07775177370286,-5.06788479128838,103.4210712814));
#57334=CARTESIAN_POINT('Ctrl Pts',(5.94821946573796,-5.21561177499016,103.413188152607));
#57335=CARTESIAN_POINT('Ctrl Pts',(5.81867912915963,-5.3633479150396,103.405304535206));
#57336=CARTESIAN_POINT('Ctrl Pts',(5.68363907950052,-5.50624649161836,103.397420917804));
#57337=CARTESIAN_POINT('Ctrl Pts',(5.54350530979244,-5.64388783378116,103.389537300403));
#57338=CARTESIAN_POINT('Ctrl Pts',(5.40333929863348,-5.78156084394648,103.381651869169));
#57339=CARTESIAN_POINT('Ctrl Pts',(5.25807747823787,-5.91397396772881,103.373766437934));
#57340=CARTESIAN_POINT('Ctrl Pts',(5.10816146609277,-6.04074560268225,103.3658810067));
#57341=CARTESIAN_POINT('Ctrl Pts',(4.95818576142647,-6.16756771468882,103.357992435699));
#57342=CARTESIAN_POINT('Ctrl Pts',(4.80355243556228,-6.28874363938329,103.350103864698));
#57343=CARTESIAN_POINT('Ctrl Pts',(4.6447350040477,-6.4039329901377,103.342215293697));
#57344=CARTESIAN_POINT('Ctrl Pts',(4.48574852061556,-6.51924495325552,103.334318325771));
#57345=CARTESIAN_POINT('Ctrl Pts',(4.32256931490728,-6.62855741168161,103.326421357845));
#57346=CARTESIAN_POINT('Ctrl Pts',(4.15569954535654,-6.73157353734797,103.31852438992));
#57347=CARTESIAN_POINT('Ctrl Pts',(3.98872798590351,-6.8346525024453,103.310622604874));
#57348=CARTESIAN_POINT('Ctrl Pts',(3.81806167368665,-6.93142730806685,103.302720819829));
#57349=CARTESIAN_POINT('Ctrl Pts',(3.64422624461561,-7.02164767544305,103.294819034784));
#57350=CARTESIAN_POINT('Ctrl Pts',(3.47016595323962,-7.11198474607054,103.286907028499));
#57351=CARTESIAN_POINT('Ctrl Pts',(3.29292866776747,-7.19575029677638,103.278995022214));
#57352=CARTESIAN_POINT('Ctrl Pts',(3.11305985701368,-7.27274221505547,103.271083015929));
#57353=CARTESIAN_POINT('Ctrl Pts',(3.03769675257106,-7.30500100385931,103.267767970072));
#57354=CARTESIAN_POINT('Ctrl Pts',(2.96187186449698,-7.33607126962668,103.264452924214));
#57355=CARTESIAN_POINT('Ctrl Pts',(2.88562602738774,-7.36594077019782,103.261137878356));
#57356=CARTESIAN_POINT('Ctrl Pts',(2.70529867907432,-7.43658446744941,103.253297536487));
#57357=CARTESIAN_POINT('Ctrl Pts',(2.52210438325268,-7.50070846118149,103.245457194618));
#57358=CARTESIAN_POINT('Ctrl Pts',(2.33656004971482,-7.55806907444466,103.237616852749));
#57359=CARTESIAN_POINT('Ctrl Pts',(2.15122316026426,-7.61536555683495,103.229785276615));
#57360=CARTESIAN_POINT('Ctrl Pts',(1.96354179724364,-7.66591361294437,103.221953700481));
#57361=CARTESIAN_POINT('Ctrl Pts',(1.77405393949023,-7.70951708084101,103.214122124348));
#57362=CARTESIAN_POINT('Ctrl Pts',(1.58474109016318,-7.75308027716356,103.206297781352));
#57363=CARTESIAN_POINT('Ctrl Pts',(1.39362540894185,-7.7897115801307,103.198473438356));
#57364=CARTESIAN_POINT('Ctrl Pts',(1.20126136194246,-7.81926416872484,103.190649095361));
#57365=CARTESIAN_POINT('Ctrl Pts',(1.00903759555761,-7.84879520622691,103.182830458232));
#57366=CARTESIAN_POINT('Ctrl Pts',(0.815567622522301,-7.8712577577781,103.175011821103));
#57367=CARTESIAN_POINT('Ctrl Pts',(0.621417658063136,-7.88655571807157,
103.167193183974));
#57368=CARTESIAN_POINT('Ctrl Pts',(0.427371558820727,-7.90184549435137,
103.159378729614));
#57369=CARTESIAN_POINT('Ctrl Pts',(0.232646542418804,-7.90997828705685,
103.151564275255));
#57370=CARTESIAN_POINT('Ctrl Pts',(0.0378157234129442,-7.91090961717189,
103.143749820895));
#57371=CARTESIAN_POINT('Ctrl Pts',(-0.156948707055732,-7.91184062993651,
103.135938029307));
#57372=CARTESIAN_POINT('Ctrl Pts',(-0.351818517124127,-7.90557506772958,
103.12812623772));
#57373=CARTESIAN_POINT('Ctrl Pts',(-0.54621860849317,-7.89212051553547,
103.120314446133));
#57374=CARTESIAN_POINT('Ctrl Pts',(-0.740627798100354,-7.87866533364658,
103.112502288942));
#57375=CARTESIAN_POINT('Ctrl Pts',(-0.934566873670922,-7.85802050473307,
103.10469013175));
#57376=CARTESIAN_POINT('Ctrl Pts',(-1.12746335672154,-7.8302456780902,103.096877974558));
#57377=CARTESIAN_POINT('Ctrl Pts',(-1.32037560923414,-7.80246858083012,
103.089065178716));
#57378=CARTESIAN_POINT('Ctrl Pts',(-1.51224475103333,-7.76756037405695,
103.081252382873));
#57379=CARTESIAN_POINT('Ctrl Pts',(-1.70250611220949,-7.72563226783992,
103.073439587031));
#57380=CARTESIAN_POINT('Ctrl Pts',(-1.89281650554473,-7.68369335635186,
103.065624777757));
#57381=CARTESIAN_POINT('Ctrl Pts',(-2.08151794931597,-7.6347310171212,103.057809968482));
#57382=CARTESIAN_POINT('Ctrl Pts',(-2.2680584546872,-7.57890703506264,103.049995159208));
#57383=CARTESIAN_POINT('Ctrl Pts',(-2.45467985952475,-7.52305884308598,
103.042176960783));
#57384=CARTESIAN_POINT('Ctrl Pts',(-2.63913812246811,-7.46034318111028,
103.034358762358));
#57385=CARTESIAN_POINT('Ctrl Pts',(-2.8208986876382,-7.39097095069931,103.026540563933));
#57386=CARTESIAN_POINT('Ctrl Pts',(-3.00287082112093,-7.32151797138817,
103.018713265168));
#57387=CARTESIAN_POINT('Ctrl Pts',(-3.18213865655702,-7.24539307377926,
103.010885966402));
#57388=CARTESIAN_POINT('Ctrl Pts',(-3.35818881071883,-7.16285480179257,
103.003058667637));
#57389=CARTESIAN_POINT('Ctrl Pts',(-3.53435389113834,-7.08026264848574,
102.995226259179));
#57390=CARTESIAN_POINT('Ctrl Pts',(-3.70729679275847,-6.99124893784943,
102.98739385072));
#57391=CARTESIAN_POINT('Ctrl Pts',(-3.87653077669679,-6.89611703332553,
102.979561442262));
#57392=CARTESIAN_POINT('Ctrl Pts',(-4.04600763524994,-6.80084860111298,
102.971717793194));
#57393=CARTESIAN_POINT('Ctrl Pts',(-4.21176464617896,-6.69944462072016,
102.963874144127));
#57394=CARTESIAN_POINT('Ctrl Pts',(-4.37334499653641,-6.59225109816593,
102.956030495059));
#57395=CARTESIAN_POINT('Ctrl Pts',(-4.46052315823942,-6.5344165024241,102.951798576355));
#57396=CARTESIAN_POINT('Ctrl Pts',(-4.54648608082056,-6.47489727741504,
102.947566657652));
#57397=CARTESIAN_POINT('Ctrl Pts',(-4.63116629696624,-6.41375239074943,
102.943334738948));
#57398=CARTESIAN_POINT('Ctrl Pts',(-4.78851743264026,-6.30013414796009,
102.935471069671));
#57399=CARTESIAN_POINT('Ctrl Pts',(-4.94192080499853,-6.1805515432417,102.927607400395));
#57400=CARTESIAN_POINT('Ctrl Pts',(-5.09088992028185,-6.05530848261033,
102.919743731118));
#57401=CARTESIAN_POINT('Ctrl Pts',(-5.23968758544185,-5.93020956553617,
102.911889112221));
#57402=CARTESIAN_POINT('Ctrl Pts',(-5.38406089155956,-5.79946338873537,
102.904034493323));
#57403=CARTESIAN_POINT('Ctrl Pts',(-5.52355189827762,-5.66341729232747,
102.896179874426));
#57404=CARTESIAN_POINT('Ctrl Pts',(-5.6629091908213,-5.52750160784995,102.88833278486));
#57405=CARTESIAN_POINT('Ctrl Pts',(-5.79739325653309,-5.38629636478731,
102.880485695293));
#57406=CARTESIAN_POINT('Ctrl Pts',(-5.92657870535733,-5.24018948600192,
102.872638605726));
#57407=CARTESIAN_POINT('Ctrl Pts',(-6.05566515247872,-5.09419457671409,
102.864797529803));
#57408=CARTESIAN_POINT('Ctrl Pts',(-6.1794608405758,-4.94330577508444,102.85695645388));
#57409=CARTESIAN_POINT('Ctrl Pts',(-6.29757663468409,-4.78794836336829,
102.849115377957));
#57410=CARTESIAN_POINT('Ctrl Pts',(-6.4156246087182,-4.63268015522787,102.841278804245));
#57411=CARTESIAN_POINT('Ctrl Pts',(-6.52799897499263,-4.47294872652082,
102.833442230534));
#57412=CARTESIAN_POINT('Ctrl Pts',(-6.63435023162384,-4.30921315371526,
102.825605656823));
#57413=CARTESIAN_POINT('Ctrl Pts',(-6.74066952816474,-4.14552678581674,
102.817771438115));
#57414=CARTESIAN_POINT('Ctrl Pts',(-6.84096912777522,-3.977838962193,102.809937219408));
#57415=CARTESIAN_POINT('Ctrl Pts',(-6.9349421079913,-3.80663880067564,102.802103000701));
#57416=CARTESIAN_POINT('Ctrl Pts',(-7.02890201322643,-3.63546245918447,
102.794269872011));
#57417=CARTESIAN_POINT('Ctrl Pts',(-7.1165368833799,-3.46077505951376,102.786436743322));
#57418=CARTESIAN_POINT('Ctrl Pts',(-7.19758505811575,-3.28309158129787,
102.778603614633));
#57419=CARTESIAN_POINT('Ctrl Pts',(-7.27863606234484,-3.10540189992932,
102.770770212479));
#57420=CARTESIAN_POINT('Ctrl Pts',(-7.35309976778337,-2.92471625007048,
102.762936810326));
#57421=CARTESIAN_POINT('Ctrl Pts',(-7.42076202748746,-2.74157106991597,
102.755103408172));
#57422=CARTESIAN_POINT('Ctrl Pts',(-7.48843842601733,-2.55838761941986,
102.747268369137));
#57423=CARTESIAN_POINT('Ctrl Pts',(-7.54931042678635,-2.37274394318788,
102.739433330102));
#57424=CARTESIAN_POINT('Ctrl Pts',(-7.60321320776555,-2.18519333635709,
102.731598291066));
#57425=CARTESIAN_POINT('Ctrl Pts',(-7.65716262412294,-1.9974804652921,102.723756473346));
#57426=CARTESIAN_POINT('Ctrl Pts',(-7.70413067826067,-1.80785770437767,
102.715914655625));
#57427=CARTESIAN_POINT('Ctrl Pts',(-7.74400307466978,-1.61689127015547,
102.708072837904));
#57428=CARTESIAN_POINT('Ctrl Pts',(-7.78389362392783,-1.42583789395975,
102.700227450011));
#57429=CARTESIAN_POINT('Ctrl Pts',(-7.81668201633006,-1.23343996951669,
102.692382062117));
#57430=CARTESIAN_POINT('Ctrl Pts',(-7.84230563603277,-1.04027078736673,
102.684536674224));
#57431=CARTESIAN_POINT('Ctrl Pts',(-7.86796117739653,-0.84686095689197,
102.676681512621));
#57432=CARTESIAN_POINT('Ctrl Pts',(-7.88643407801548,-0.652678297003844,
102.668826351018));
#57433=CARTESIAN_POINT('Ctrl Pts',(-7.89771376744866,-0.45829929898697,
102.660971189416));
#57434=CARTESIAN_POINT('Ctrl Pts',(-7.90659393108899,-0.305270501442419,
102.654787054572));
#57435=CARTESIAN_POINT('Ctrl Pts',(-7.91101682177921,-0.152120092814248,
102.648602919728));
#57436=CARTESIAN_POINT('Ctrl Pts',(-7.91099995190663,0.000872314928047417,
102.642418784884));
#57437=CARTESIAN_POINT('',(-7.91099999491492,-0.00028364795766521,98.635032539653));
#57438=CARTESIAN_POINT('Ctrl Pts',(-7.91099993013027,0.00105141757446709,
102.647258864909));
#57439=CARTESIAN_POINT('Ctrl Pts',(-7.91097619318975,0.179651185499931,
102.640642093266));
#57440=CARTESIAN_POINT('Ctrl Pts',(-7.90490459988792,0.35819593563781,102.63379939406));
#57441=CARTESIAN_POINT('Ctrl Pts',(-7.89220454811321,0.545072556459039,
102.626295665916));
#57442=CARTESIAN_POINT('Ctrl Pts',(-7.89160021739073,0.553753310620412,
102.625946399728));
#57443=CARTESIAN_POINT('Ctrl Pts',(-7.89058727690093,0.567964948982951,
102.625373465286));
#57444=CARTESIAN_POINT('Ctrl Pts',(-7.89018717026809,0.573496447735965,
102.625150184159));
#57445=CARTESIAN_POINT('Ctrl Pts',(-7.88946979434076,0.583271353134799,
102.624755123277));
#57446=CARTESIAN_POINT('Ctrl Pts',(-7.88915491705159,0.587514937562228,
102.624583451073));
#57447=CARTESIAN_POINT('Ctrl Pts',(-7.88852861687332,0.595864258755811,
102.624245362585));
#57448=CARTESIAN_POINT('Ctrl Pts',(-7.88821741205822,0.599970011002315,
102.624078956052));
#57449=CARTESIAN_POINT('Ctrl Pts',(-7.88759128868958,0.608145810706466,
102.623747288526));
#57450=CARTESIAN_POINT('Ctrl Pts',(-7.88727642496625,0.612215861096921,
102.62358203));
#57451=CARTESIAN_POINT('Ctrl Pts',(-7.8865235349574,0.62185102311047,102.623190458366));
#57452=CARTESIAN_POINT('Ctrl Pts',(-7.88608276864437,0.627415913274009,
102.622964025717));
#57453=CARTESIAN_POINT('Ctrl Pts',(-7.88451967146883,0.646888897059917,
102.622170722648));
#57454=CARTESIAN_POINT('Ctrl Pts',(-7.88336643893215,0.660794431650021,
102.621602521431));
#57455=CARTESIAN_POINT('Ctrl Pts',(-7.8684776900109,0.83473293188157,102.614474309575));
#57456=CARTESIAN_POINT('Ctrl Pts',(-7.84990870092257,0.994308438496762,
102.607714747561));
#57457=CARTESIAN_POINT('Ctrl Pts',(-7.8237344739426,1.17194663699994,102.600015381335));
#57458=CARTESIAN_POINT('Ctrl Pts',(-7.82090501308979,1.19068249731943,102.599201120564));
#57459=CARTESIAN_POINT('Ctrl Pts',(-7.8137411971457,1.23699174550653,102.59718333632));
#57460=CARTESIAN_POINT('Ctrl Pts',(-7.80932818433038,1.26455263536201,102.595977904239));
#57461=CARTESIAN_POINT('Ctrl Pts',(-7.72050994056059,1.80105257813195,102.572430226951));
#57462=CARTESIAN_POINT('Ctrl Pts',(-7.58666811392793,2.30055422518567,102.549156478115));
#57463=CARTESIAN_POINT('Ctrl Pts',(-7.25202901720152,3.19082707971832,102.507563032799));
#57464=CARTESIAN_POINT('Ctrl Pts',(-7.0655526334846,3.58487391081999,102.489092294102));
#57465=CARTESIAN_POINT('Ctrl Pts',(-6.82481117722698,4.00099283638436,102.469552829782));
#57466=CARTESIAN_POINT('Ctrl Pts',(-6.80168635647896,4.04017995262355,102.467711734066));
#57467=CARTESIAN_POINT('Ctrl Pts',(-6.77028616356006,4.0923566908158,102.465258438393));
#57468=CARTESIAN_POINT('Ctrl Pts',(-6.76230924216551,4.10552453858889,102.464639134205));
#57469=CARTESIAN_POINT('Ctrl Pts',(-6.74906508852445,4.12724391086071,102.463617333667));
#57470=CARTESIAN_POINT('Ctrl Pts',(-6.74381993105232,4.13580882138465,102.46321431375));
#57471=CARTESIAN_POINT('Ctrl Pts',(-6.73358078677488,4.15245723277549,102.46243076269));
#57472=CARTESIAN_POINT('Ctrl Pts',(-6.72858851708777,4.16054177365766,102.462050191014));
#57473=CARTESIAN_POINT('Ctrl Pts',(-6.71701562020045,4.1792077513163,102.46117133034));
#57474=CARTESIAN_POINT('Ctrl Pts',(-6.7104245272021,4.18978268369556,102.460673292121));
#57475=CARTESIAN_POINT('Ctrl Pts',(-6.692657991791,4.21813833899796,102.459337486896));
#57476=CARTESIAN_POINT('Ctrl Pts',(-6.68143666386314,4.23589024344511,102.458500827832));
#57477=CARTESIAN_POINT('Ctrl Pts',(-6.60053914302513,4.3627471445224,102.452519097253));
#57478=CARTESIAN_POINT('Ctrl Pts',(-6.5282636383704,4.47017391349305,102.447438707664));
#57479=CARTESIAN_POINT('Ctrl Pts',(-6.08991358756491,5.088394238714,102.41807289235));
#57480=CARTESIAN_POINT('Ctrl Pts',(-5.66667411316083,5.55586456609055,102.395571857204));
#57481=CARTESIAN_POINT('Ctrl Pts',(-5.09935993276306,6.04943927067375,102.368313011645));
#57482=CARTESIAN_POINT('Ctrl Pts',(-5.00425814755397,6.12834292841191,102.363818351838));
#57483=CARTESIAN_POINT('Ctrl Pts',(-4.78876014827182,6.2987742180952,102.353725830385));
#57484=CARTESIAN_POINT('Ctrl Pts',(-4.66751010816992,6.38914138732312,102.348108337351));
#57485=CARTESIAN_POINT('Ctrl Pts',(-4.45298562732648,6.53965849992211,102.338161081202));
#57486=CARTESIAN_POINT('Ctrl Pts',(-4.36089638846656,6.60142376053902,102.33388830735));
#57487=CARTESIAN_POINT('Ctrl Pts',(-4.23797158991794,6.68017597935315,102.328145428691));
#57488=CARTESIAN_POINT('Ctrl Pts',(-4.20827550925301,6.69892315965258,102.326755098169));
#57489=CARTESIAN_POINT('Ctrl Pts',(-4.16564985920987,6.72543750977358,102.32475392299));
#57490=CARTESIAN_POINT('Ctrl Pts',(-4.15282112479293,6.73336655385158,102.324150936989));
#57491=CARTESIAN_POINT('Ctrl Pts',(-4.13015268970366,6.74728778731678,102.323084088224));
#57492=CARTESIAN_POINT('Ctrl Pts',(-4.12032240085698,6.75329527239323,102.322620991194));
#57493=CARTESIAN_POINT('Ctrl Pts',(-4.10572529558253,6.76217211794273,102.32193261631));
#57494=CARTESIAN_POINT('Ctrl Pts',(-4.10096848982942,6.76505797467126,102.321708180755));
#57495=CARTESIAN_POINT('Ctrl Pts',(-4.09265419191567,6.77009009745385,102.321315692805));
#57496=CARTESIAN_POINT('Ctrl Pts',(-4.08909804193423,6.77223858599228,102.321147755104));
#57497=CARTESIAN_POINT('Ctrl Pts',(-4.08202162619004,6.77650627732625,102.320813442693));
#57498=CARTESIAN_POINT('Ctrl Pts',(-4.07850139817033,6.77862554124064,102.320647071217));
#57499=CARTESIAN_POINT('Ctrl Pts',(-4.07010628986744,6.78367069620361,102.320250147693));
#57500=CARTESIAN_POINT('Ctrl Pts',(-4.06522990835805,6.78659407341233,102.320019464226));
#57501=CARTESIAN_POINT('Ctrl Pts',(-4.05052996952463,6.79538511770749,102.31932367235));
#57502=CARTESIAN_POINT('Ctrl Pts',(-4.040696859153,6.80123671270748,102.318857714628));
#57503=CARTESIAN_POINT('Ctrl Pts',(-3.92850446450238,6.86767220470696,102.313534939814));
#57504=CARTESIAN_POINT('Ctrl Pts',(-3.82481786982913,6.92595355047103,102.308545762944));
#57505=CARTESIAN_POINT('Ctrl Pts',(-3.69979027117438,6.99256677234025,102.302463787982));
#57506=CARTESIAN_POINT('Ctrl Pts',(-3.67967499574954,7.00317285422648,102.301483453866));
#57507=CARTESIAN_POINT('Ctrl Pts',(-3.40709862087158,7.14539426618797,102.288177417609));
#57508=CARTESIAN_POINT('Ctrl Pts',(-3.14776965808816,7.26336761434618,102.275272202322));
#57509=CARTESIAN_POINT('Ctrl Pts',(-2.85431605766383,7.37819269488221,102.260813395882));
#57510=CARTESIAN_POINT('Ctrl Pts',(-2.82590506180737,7.38912093370939,102.259414933542));
#57511=CARTESIAN_POINT('Ctrl Pts',(-2.76582490602053,7.4118334675935,102.256461367515));
#57512=CARTESIAN_POINT('Ctrl Pts',(-2.73414186751939,7.42357939289169,102.254905991946));
#57513=CARTESIAN_POINT('Ctrl Pts',(-2.66677082559187,7.44806620935744,102.25160432986));
#57514=CARTESIAN_POINT('Ctrl Pts',(-2.6310645324822,7.46075440662486,102.249857838216));
#57515=CARTESIAN_POINT('Ctrl Pts',(-2.5547493702244,7.48725693817743,102.246133708878));
#57516=CARTESIAN_POINT('Ctrl Pts',(-2.5141164657259,7.50099854696139,102.244156038204));
#57517=CARTESIAN_POINT('Ctrl Pts',(-2.42674948512295,7.52975545933348,102.239916883274));
#57518=CARTESIAN_POINT('Ctrl Pts',(-2.37998325470231,7.54466765775602,102.237655732956));
#57519=CARTESIAN_POINT('Ctrl Pts',(-2.27861747871593,7.57595355408697,102.232774824085));
#57520=CARTESIAN_POINT('Ctrl Pts',(-2.22397346184015,7.5921743896793,102.230156165179));
#57521=CARTESIAN_POINT('Ctrl Pts',(-1.96450378655201,7.66615512754583,102.217789977196));
#57522=CARTESIAN_POINT('Ctrl Pts',(-1.75757164823691,7.71622688304804,102.208130903311));
#57523=CARTESIAN_POINT('Ctrl Pts',(-1.37393010219411,7.79282101426147,102.190729656883));
#57524=CARTESIAN_POINT('Ctrl Pts',(-1.19785723343373,7.82182116270348,102.182934513702));
#57525=CARTESIAN_POINT('Ctrl Pts',(-0.886246271514019,7.86237497129892,
102.169511000969));
#57526=CARTESIAN_POINT('Ctrl Pts',(-0.751112268389215,7.87643354791872,
102.163811234974));
#57527=CARTESIAN_POINT('Ctrl Pts',(-0.546083352752086,7.89243859485094,
102.155348575693));
#57528=CARTESIAN_POINT('Ctrl Pts',(-0.476418213367624,7.8969500454934,102.152505228884));
#57529=CARTESIAN_POINT('Ctrl Pts',(-0.393549480976554,7.90121593385416,
102.14916043382));
#57530=CARTESIAN_POINT('Ctrl Pts',(-0.380396001030403,7.90186011721237,
102.148630644501));
#57531=CARTESIAN_POINT('Ctrl Pts',(-0.360140564698243,7.90280142087243,
102.147816519767));
#57532=CARTESIAN_POINT('Ctrl Pts',(-0.353039744358613,7.90312181756908,
102.147531441379));
#57533=CARTESIAN_POINT('Ctrl Pts',(-0.340094389964134,7.90368844431816,
102.147012310148));
#57534=CARTESIAN_POINT('Ctrl Pts',(-0.334250000218825,7.90393776269027,
102.146778158805));
#57535=CARTESIAN_POINT('Ctrl Pts',(-0.321512568785072,7.90446698141622,
102.146268318279));
#57536=CARTESIAN_POINT('Ctrl Pts',(-0.314619423483892,7.90474434822975,
102.145992710243));
#57537=CARTESIAN_POINT('Ctrl Pts',(-0.29584696728772,7.90547512140316,102.145242956579));
#57538=CARTESIAN_POINT('Ctrl Pts',(-0.283966961026479,7.90591076915511,
102.144769378979));
#57539=CARTESIAN_POINT('Ctrl Pts',(-0.227272508236372,7.90786183699207,
102.142513604787));
#57540=CARTESIAN_POINT('Ctrl Pts',(-0.182446272295308,7.90902301612059,
102.140742753471));
#57541=CARTESIAN_POINT('Ctrl Pts',(-0.121808602386883,7.91007796993064,
102.138363987727));
#57542=CARTESIAN_POINT('Ctrl Pts',(-0.106004262811609,7.91030555199766,
102.137745530848));
#57543=CARTESIAN_POINT('Ctrl Pts',(0.780549246606244,7.92041447550463,102.103137906176));
#57544=CARTESIAN_POINT('Ctrl Pts',(1.64684287660674,7.78652997427673,102.074813652592));
#57545=CARTESIAN_POINT('Ctrl Pts',(2.70480258652009,7.43821515039594,102.036384232167));
#57546=CARTESIAN_POINT('Ctrl Pts',(2.9320407002333,7.35160715009197,102.027822986929));
#57547=CARTESIAN_POINT('Ctrl Pts',(3.24886335761303,7.2138271732473,102.015009688091));
#57548=CARTESIAN_POINT('Ctrl Pts',(3.34200202500479,7.17115309131828,102.011130737214));
#57549=CARTESIAN_POINT('Ctrl Pts',(3.47339244222461,7.1078372748321,102.00546346647));
#57550=CARTESIAN_POINT('Ctrl Pts',(3.51234587938199,7.08866927409591,102.00375842055));
#57551=CARTESIAN_POINT('Ctrl Pts',(3.57340584622635,7.05799635822397,102.001043547455));
#57552=CARTESIAN_POINT('Ctrl Pts',(3.59561958174149,7.04670573611469,102.000047002708));
#57553=CARTESIAN_POINT('Ctrl Pts',(3.6233820451247,7.03242939855693,101.998789958992));
#57554=CARTESIAN_POINT('Ctrl Pts',(3.628981265905,7.02954163952994,101.998535842494));
#57555=CARTESIAN_POINT('Ctrl Pts',(3.63733304208231,7.02522163130205,101.998155910825));
#57556=CARTESIAN_POINT('Ctrl Pts',(3.64008822588083,7.02379444002228,101.998030429279));
#57557=CARTESIAN_POINT('Ctrl Pts',(3.64544570798496,7.02101525350872,101.997786145462));
#57558=CARTESIAN_POINT('Ctrl Pts',(3.64804809448055,7.01966343211415,101.997667354707));
#57559=CARTESIAN_POINT('Ctrl Pts',(3.65349119151277,7.01683214649027,101.997418622664));
#57560=CARTESIAN_POINT('Ctrl Pts',(3.65633175710737,7.01535240315055,101.997288662939));
#57561=CARTESIAN_POINT('Ctrl Pts',(3.66419317609988,7.01125106168745,101.996928564923));
#57562=CARTESIAN_POINT('Ctrl Pts',(3.66921210523156,7.00862580027559,101.996698186207));
#57563=CARTESIAN_POINT('Ctrl Pts',(3.68893526399893,6.99828217535659,101.995790968387));
#57564=CARTESIAN_POINT('Ctrl Pts',(3.70361790033703,6.9905229581518,101.995111476691));
#57565=CARTESIAN_POINT('Ctrl Pts',(3.95239237194866,6.85805130878709,101.983529949603));
#57566=CARTESIAN_POINT('Ctrl Pts',(4.18007288285763,6.72169922156217,101.97190165355));
#57567=CARTESIAN_POINT('Ctrl Pts',(4.40388284763992,6.57189119476423,101.959749236539));
#57568=CARTESIAN_POINT('Ctrl Pts',(4.40730859039656,6.56959427974921,101.959563047092));
#57569=CARTESIAN_POINT('Ctrl Pts',(4.41411424894203,6.56502345706303,101.959192805852));
#57570=CARTESIAN_POINT('Ctrl Pts',(4.41749420790928,6.56274961561038,101.959008756072));
#57571=CARTESIAN_POINT('Ctrl Pts',(4.79175050178151,6.31055144771266,101.938610192457));
#57572=CARTESIAN_POINT('Ctrl Pts',(5.14076639969692,6.02963193599232,101.917568020216));
#57573=CARTESIAN_POINT('Ctrl Pts',(5.51183238703923,5.67520638298301,101.894082991572));
#57574=CARTESIAN_POINT('Ctrl Pts',(5.55891651236179,5.6290950538082,101.891078956005));
#57575=CARTESIAN_POINT('Ctrl Pts',(5.66148119870899,5.52610744111659,101.884486686933));
#57576=CARTESIAN_POINT('Ctrl Pts',(5.71669252692006,5.46897245571656,101.880905688421));
#57577=CARTESIAN_POINT('Ctrl Pts',(5.85214545315515,5.32450721670695,101.872046766253));
#57578=CARTESIAN_POINT('Ctrl Pts',(5.93130275489698,5.23618492350482,101.866803188947));
#57579=CARTESIAN_POINT('Ctrl Pts',(6.13589716174251,4.9973067057493,101.853089797723));
#57580=CARTESIAN_POINT('Ctrl Pts',(6.25778080825266,4.84380996680798,101.844752450794));
#57581=CARTESIAN_POINT('Ctrl Pts',(6.4263270822239,4.6145521406595,101.832980815322));
#57582=CARTESIAN_POINT('Ctrl Pts',(6.47760668544398,4.54228836010891,101.829363063229));
#57583=CARTESIAN_POINT('Ctrl Pts',(6.53555274278236,4.45765256665546,101.825230429409));
#57584=CARTESIAN_POINT('Ctrl Pts',(6.54341227073,4.4461075016959,101.82466891598));
#57585=CARTESIAN_POINT('Ctrl Pts',(6.55530086618688,4.42854423073005,101.82381804049));
#57586=CARTESIAN_POINT('Ctrl Pts',(6.55935229071512,4.42254123512997,101.823527808502));
#57587=CARTESIAN_POINT('Ctrl Pts',(6.56664086477851,4.41170970787824,101.82300518936));
#57588=CARTESIAN_POINT('Ctrl Pts',(6.56988094365253,4.40688315933032,101.82277268853));
#57589=CARTESIAN_POINT('Ctrl Pts',(6.57636132243499,4.39720670173508,101.822307319365));
#57590=CARTESIAN_POINT('Ctrl Pts',(6.57960158453984,4.39235677170207,101.822074452563));
#57591=CARTESIAN_POINT('Ctrl Pts',(6.5886536739918,4.37877537443949,101.821423411064));
#57592=CARTESIAN_POINT('Ctrl Pts',(6.59445351452491,4.37003591077846,101.82100570022));
#57593=CARTESIAN_POINT('Ctrl Pts',(6.61784793439725,4.33463150713187,101.819318451357));
#57594=CARTESIAN_POINT('Ctrl Pts',(6.63529841675315,4.30787146249326,101.818054470776));
#57595=CARTESIAN_POINT('Ctrl Pts',(6.9018825556959,3.89360576545395,101.798658665059));
#57596=CARTESIAN_POINT('Ctrl Pts',(7.11687693210921,3.48515009148752,101.781917112215));
#57597=CARTESIAN_POINT('Ctrl Pts',(7.39140709839853,2.83072231598911,101.757159938033));
#57598=CARTESIAN_POINT('Ctrl Pts',(7.47681553189919,2.59675166362009,101.748668432677));
#57599=CARTESIAN_POINT('Ctrl Pts',(7.6241720772216,2.12509873357997,101.731752705972));
#57600=CARTESIAN_POINT('Ctrl Pts',(7.68637097421647,1.88778699413457,101.723337552833));
#57601=CARTESIAN_POINT('Ctrl Pts',(7.77858415927764,1.45483523743107,101.70762076493));
#57602=CARTESIAN_POINT('Ctrl Pts',(7.81247274905533,1.26022969233395,101.7004253305));
#57603=CARTESIAN_POINT('Ctrl Pts',(7.84827264998825,0.996614599443258,101.690270189082));
#57604=CARTESIAN_POINT('Ctrl Pts',(7.85661709764574,0.928542706448378,101.687611437046));
#57605=CARTESIAN_POINT('Ctrl Pts',(7.86659422609799,0.837348633381466,101.683990888177));
#57606=CARTESIAN_POINT('Ctrl Pts',(7.86901203324911,0.814313853528825,101.683071372994));
#57607=CARTESIAN_POINT('Ctrl Pts',(7.8723634172595,0.780975198023991,101.6817328954));
#57608=CARTESIAN_POINT('Ctrl Pts',(7.87337800910295,0.77067941273266,101.681318486895));
#57609=CARTESIAN_POINT('Ctrl Pts',(7.87514927217471,0.752336539923534,101.680578257216));
#57610=CARTESIAN_POINT('Ctrl Pts',(7.87591381589302,0.744290193865863,101.68025288648));
#57611=CARTESIAN_POINT('Ctrl Pts',(7.8770482494476,0.732153497230544,101.679761102085));
#57612=CARTESIAN_POINT('Ctrl Pts',(7.87742728719592,0.728064009855788,101.67959522142));
#57613=CARTESIAN_POINT('Ctrl Pts',(7.87808178660637,0.720942185282276,101.679306042363));
#57614=CARTESIAN_POINT('Ctrl Pts',(7.87835868284953,0.717909977158523,101.679182826431));
#57615=CARTESIAN_POINT('Ctrl Pts',(7.87892659818121,0.71165100798842,101.678928295369));
#57616=CARTESIAN_POINT('Ctrl Pts',(7.87921738567086,0.708424227411561,101.678796967058));
#57617=CARTESIAN_POINT('Ctrl Pts',(7.8799146940792,0.700632867281794,101.678479608142));
#57618=CARTESIAN_POINT('Ctrl Pts',(7.88031923073747,0.696068116048889,101.678293465046));
#57619=CARTESIAN_POINT('Ctrl Pts',(7.88155504074823,0.68198419729996,101.677718500795));
#57620=CARTESIAN_POINT('Ctrl Pts',(7.88237303123551,0.67246390287261,101.677328933718));
#57621=CARTESIAN_POINT('Ctrl Pts',(7.89169490534443,0.561615695186437,101.672782676084));
#57622=CARTESIAN_POINT('Ctrl Pts',(7.89826131812768,0.460138225407757,101.668519764074));
#57623=CARTESIAN_POINT('Ctrl Pts',(7.90326108228446,0.349942555656956,101.663802430475));
#57624=CARTESIAN_POINT('Ctrl Pts',(7.90363825123258,0.341317916025791,101.663432634978));
#57625=CARTESIAN_POINT('Ctrl Pts',(7.90471838697994,0.315656414240807,101.662330648095));
#57626=CARTESIAN_POINT('Ctrl Pts',(7.9053803869428,0.298617950679037,101.661596722377));
#57627=CARTESIAN_POINT('Ctrl Pts',(7.90665661102096,0.26278480148346,101.660048701701));
#57628=CARTESIAN_POINT('Ctrl Pts',(7.90725891690065,0.243989812291861,101.659234128818));
#57629=CARTESIAN_POINT('Ctrl Pts',(7.91088304914098,0.116726109894249,101.653701641022));
#57630=CARTESIAN_POINT('Ctrl Pts',(7.91173980970498,0.00821021824212436,
101.648901223505));
#57631=CARTESIAN_POINT('Ctrl Pts',(7.90165874434802,-0.786968130354667,
101.613278636282));
#57632=CARTESIAN_POINT('Ctrl Pts',(7.80358378605594,-1.46961676903034,101.580577598229));
#57633=CARTESIAN_POINT('Ctrl Pts',(7.53619871956156,-2.42551030567191,101.536792535712));
#57634=CARTESIAN_POINT('Ctrl Pts',(7.43683791213763,-2.71493282556897,101.523765462613));
#57635=CARTESIAN_POINT('Ctrl Pts',(7.30409212781048,-3.03910207651414,101.509475340094));
#57636=CARTESIAN_POINT('Ctrl Pts',(7.28687252749589,-3.08016105018375,101.50767074036));
#57637=CARTESIAN_POINT('Ctrl Pts',(7.26470581916521,-3.13178964499847,101.505408091542));
#57638=CARTESIAN_POINT('Ctrl Pts',(7.26008089185093,-3.14249621556035,101.504939225055));
#57639=CARTESIAN_POINT('Ctrl Pts',(7.2526779895193,-3.15953014412524,101.504193824657));
#57640=CARTESIAN_POINT('Ctrl Pts',(7.24991537968331,-3.16586413780434,101.503916773446));
#57641=CARTESIAN_POINT('Ctrl Pts',(7.24469371815047,-3.17779346160022,101.503395209691));
#57642=CARTESIAN_POINT('Ctrl Pts',(7.24223647548086,-3.18338957525258,101.503150636385));
#57643=CARTESIAN_POINT('Ctrl Pts',(7.23669536265386,-3.19596925962113,101.502601064543));
#57644=CARTESIAN_POINT('Ctrl Pts',(7.23360786197535,-3.20295122970732,101.502296188862));
#57645=CARTESIAN_POINT('Ctrl Pts',(7.22572640056235,-3.22070457949131,101.501521339586));
#57646=CARTESIAN_POINT('Ctrl Pts',(7.22091845067828,-3.23146974832196,101.501051839164));
#57647=CARTESIAN_POINT('Ctrl Pts',(7.19413993619844,-3.29106959884842,101.49845440975));
#57648=CARTESIAN_POINT('Ctrl Pts',(7.17169779408785,-3.3396915151882,101.496342482017));
#57649=CARTESIAN_POINT('Ctrl Pts',(6.79524496636827,-4.13399692486191,101.461945981394));
#57650=CARTESIAN_POINT('Ctrl Pts',(6.32722201323277,-4.8199049684268,101.434487131371));
#57651=CARTESIAN_POINT('Ctrl Pts',(5.61066582405834,-5.58147543859712,101.397711741201));
#57652=CARTESIAN_POINT('Ctrl Pts',(5.45309762544546,-5.73551717662546,101.389823643687));
#57653=CARTESIAN_POINT('Ctrl Pts',(5.1838218846574,-5.97762806844629,101.376284307568));
#57654=CARTESIAN_POINT('Ctrl Pts',(5.07580078994123,-6.06962018986386,101.370838044886));
#57655=CARTESIAN_POINT('Ctrl Pts',(4.95402821506918,-6.16779844908681,101.364611780146));
#57656=CARTESIAN_POINT('Ctrl Pts',(4.94266095763329,-6.17691151929386,101.364029756897));
#57657=CARTESIAN_POINT('Ctrl Pts',(4.92544702115388,-6.19063389891782,101.363147042981));
#57658=CARTESIAN_POINT('Ctrl Pts',(4.9196188540688,-6.19526648003415,101.362847950794));
#57659=CARTESIAN_POINT('Ctrl Pts',(4.90887428015409,-6.20378219730299,101.362296117204));
#57660=CARTESIAN_POINT('Ctrl Pts',(4.90395977827138,-6.2076677377753,101.362043543186));
#57661=CARTESIAN_POINT('Ctrl Pts',(4.89607551691126,-6.21388604610928,101.361638063364));
#57662=CARTESIAN_POINT('Ctrl Pts',(4.89310868548351,-6.21622253891251,101.361485418916));
#57663=CARTESIAN_POINT('Ctrl Pts',(4.88742531663828,-6.2206918186541,101.361192884421));
#57664=CARTESIAN_POINT('Ctrl Pts',(4.88470906164277,-6.22282494622495,101.361053019188));
#57665=CARTESIAN_POINT('Ctrl Pts',(4.87851097366141,-6.22768586586458,101.360733745228));
#57666=CARTESIAN_POINT('Ctrl Pts',(4.87502825266005,-6.23041251440632,101.360554256603));
#57667=CARTESIAN_POINT('Ctrl Pts',(4.865986565639,-6.23747909657683,101.360088052759));
#57668=CARTESIAN_POINT('Ctrl Pts',(4.86042409075307,-6.24181451139192,101.359801023918));
#57669=CARTESIAN_POINT('Ctrl Pts',(4.82660988220073,-6.26809683024638,101.358054892878));
#57670=CARTESIAN_POINT('Ctrl Pts',(4.79821573081392,-6.28985902502156,101.356583202458));
#57671=CARTESIAN_POINT('Ctrl Pts',(4.30761808661232,-6.66061373563912,101.331076833713));
#57672=CARTESIAN_POINT('Ctrl Pts',(3.80863955449585,-6.95798414860458,101.304068741185));
#57673=CARTESIAN_POINT('Ctrl Pts',(2.74200745312272,-7.44426932886802,101.250345207927));
#57674=CARTESIAN_POINT('Ctrl Pts',(2.17626920047898,-7.62887885566547,101.223882076375));
#57675=CARTESIAN_POINT('Ctrl Pts',(1.54325771945928,-7.75919343962312,101.197443963005));
#57676=CARTESIAN_POINT('Ctrl Pts',(1.49126538578825,-7.76935357109912,101.195293361842));
#57677=CARTESIAN_POINT('Ctrl Pts',(1.42701668325811,-7.78124008440692,101.192661112911));
#57678=CARTESIAN_POINT('Ctrl Pts',(1.41485382736987,-7.78346083143229,101.192163920056));
#57679=CARTESIAN_POINT('Ctrl Pts',(1.39573138450325,-7.78690598606026,101.191383977268));
#57680=CARTESIAN_POINT('Ctrl Pts',(1.38877530248622,-7.78814959364303,101.19110062341));
#57681=CARTESIAN_POINT('Ctrl Pts',(1.37641846030216,-7.79034166706965,101.190597912631));
#57682=CARTESIAN_POINT('Ctrl Pts',(1.3710183668916,-7.79129384026519,101.190378439187));
#57683=CARTESIAN_POINT('Ctrl Pts',(1.35949214114425,-7.7933138514888,101.189910447001));
#57684=CARTESIAN_POINT('Ctrl Pts',(1.35336572928745,-7.79438008263954,101.189661978934));
#57685=CARTESIAN_POINT('Ctrl Pts',(1.33574913426386,-7.7974246510065,101.188948304212));
#57686=CARTESIAN_POINT('Ctrl Pts',(1.32425580446123,-7.79938481571741,101.188483669175));
#57687=CARTESIAN_POINT('Ctrl Pts',(1.27401758228586,-7.80783859524756,101.186456957174));
#57688=CARTESIAN_POINT('Ctrl Pts',(1.23522865231797,-7.81406901440788,101.184903157739));
#57689=CARTESIAN_POINT('Ctrl Pts',(0.638933879964946,-7.90529700461379,
101.161182224305));
#57690=CARTESIAN_POINT('Ctrl Pts',(0.073921455706333,-7.93073599718231,
101.141089579641));
#57691=CARTESIAN_POINT('Ctrl Pts',(-0.9063774347419,-7.87002272239105,101.107158435465));
#57692=CARTESIAN_POINT('Ctrl Pts',(-1.32101243080726,-7.81112525796685,
101.093047575357));
#57693=CARTESIAN_POINT('Ctrl Pts',(-1.87928904056887,-7.6860850732928,101.07251351499));
#57694=CARTESIAN_POINT('Ctrl Pts',(-2.02852692444375,-7.64805242923836,
101.06686557821));
#57695=CARTESIAN_POINT('Ctrl Pts',(-2.27835446602918,-7.57655819124616,
101.05700636134));
#57696=CARTESIAN_POINT('Ctrl Pts',(-2.37955619778753,-7.54538559025373,
101.052898147011));
#57697=CARTESIAN_POINT('Ctrl Pts',(-2.49744462419737,-7.50646555029554,
101.047946330544));
#57698=CARTESIAN_POINT('Ctrl Pts',(-2.51477139247207,-7.50067860544299,
101.047214284137));
#57699=CARTESIAN_POINT('Ctrl Pts',(-2.53754579985817,-7.49298442710936,
101.046246299686));
#57700=CARTESIAN_POINT('Ctrl Pts',(-2.54301173368562,-7.49113113176432,
101.046013541344));
#57701=CARTESIAN_POINT('Ctrl Pts',(-2.55193750858615,-7.48809383786527,
101.045632726764));
#57702=CARTESIAN_POINT('Ctrl Pts',(-2.55539857351451,-7.48691341627509,
101.045484883781));
#57703=CARTESIAN_POINT('Ctrl Pts',(-2.5620711261004,-7.48463252735323,101.04519951322));
#57704=CARTESIAN_POINT('Ctrl Pts',(-2.56528272704113,-7.48353239152389,
101.045062005561));
#57705=CARTESIAN_POINT('Ctrl Pts',(-2.5726486846059,-7.48100387946494,101.044746268814));
#57706=CARTESIAN_POINT('Ctrl Pts',(-2.57680256007557,-7.47957410988401,
101.044567955501));
#57707=CARTESIAN_POINT('Ctrl Pts',(-2.59007549949146,-7.47499317686568,
101.043997350104));
#57708=CARTESIAN_POINT('Ctrl Pts',(-2.59918995798751,-7.4718288021053,101.043604253362));
#57709=CARTESIAN_POINT('Ctrl Pts',(-2.68135509803504,-7.44313402047717,
101.040049301053));
#57710=CARTESIAN_POINT('Ctrl Pts',(-2.75403108214714,-7.41655049537198,
101.036824583172));
#57711=CARTESIAN_POINT('Ctrl Pts',(-2.84250899455956,-7.38270713730397,
101.03281088229));
#57712=CARTESIAN_POINT('Ctrl Pts',(-2.85869441468221,-7.37645499511943,
101.032073020297));
#57713=CARTESIAN_POINT('Ctrl Pts',(-3.59900682991811,-7.08768286441425,
100.998161774338));
#57714=CARTESIAN_POINT('Ctrl Pts',(-4.27758514548638,-6.70003935796028,
100.96046698622));
#57715=CARTESIAN_POINT('Ctrl Pts',(-5.03260917231484,-6.10657327914682,
100.91749461562));
#57716=CARTESIAN_POINT('Ctrl Pts',(-5.17248568598446,-5.98855487793442,
100.909453772229));
#57717=CARTESIAN_POINT('Ctrl Pts',(-5.45389990521558,-5.73389359797819,
100.893157306934));
#57718=CARTESIAN_POINT('Ctrl Pts',(-5.59468912316628,-5.59660799971827,
100.884936279293));
#57719=CARTESIAN_POINT('Ctrl Pts',(-5.75353757489532,-5.42972095784023,
100.875576982976));
#57720=CARTESIAN_POINT('Ctrl Pts',(-5.77669262697199,-5.40507970684385,
100.874210421121));
#57721=CARTESIAN_POINT('Ctrl Pts',(-5.8066963163013,-5.37273720213874,100.872436546115));
#57722=CARTESIAN_POINT('Ctrl Pts',(-5.81368870592683,-5.36517015430477,
100.872022918943));
#57723=CARTESIAN_POINT('Ctrl Pts',(-5.82502718977465,-5.35285164211235,
100.871351833239));
#57724=CARTESIAN_POINT('Ctrl Pts',(-5.82938228956825,-5.34810850548187,
100.871093980771));
#57725=CARTESIAN_POINT('Ctrl Pts',(-5.83772881947123,-5.33899599672367,
100.870599634621));
#57726=CARTESIAN_POINT('Ctrl Pts',(-5.84172114623067,-5.33462745396524,
100.870363101856));
#57727=CARTESIAN_POINT('Ctrl Pts',(-5.85081322321812,-5.32465614150758,
100.869824249268));
#57728=CARTESIAN_POINT('Ctrl Pts',(-5.8559098381162,-5.31905051363067,100.869522065972));
#57729=CARTESIAN_POINT('Ctrl Pts',(-5.86930864174531,-5.30427093530072,
100.868727300169));
#57730=CARTESIAN_POINT('Ctrl Pts',(-5.87759738968799,-5.29508479759359,
100.868235300866));
#57731=CARTESIAN_POINT('Ctrl Pts',(-5.9070337350238,-5.26230721510433,100.866486784868));
#57732=CARTESIAN_POINT('Ctrl Pts',(-5.92806125341561,-5.23860807648435,
100.865235449168));
#57733=CARTESIAN_POINT('Ctrl Pts',(-6.29239053119782,-4.82298672313823,
100.843511586092));
#57734=CARTESIAN_POINT('Ctrl Pts',(-6.59630891523287,-4.39819983262814,
100.82484794742));
#57735=CARTESIAN_POINT('Ctrl Pts',(-7.1101005549623,-3.505607731158,100.789270467862));
#57736=CARTESIAN_POINT('Ctrl Pts',(-7.32078269633412,-3.04119959820609,
100.772376901192));
#57737=CARTESIAN_POINT('Ctrl Pts',(-7.55590825743394,-2.35364552567562,
100.745933261476));
#57738=CARTESIAN_POINT('Ctrl Pts',(-7.61785960523315,-2.1446673945528,100.737705504192));
#57739=CARTESIAN_POINT('Ctrl Pts',(-7.67353438125915,-1.92376975046819,
100.728561496283));
#57740=CARTESIAN_POINT('Ctrl Pts',(-7.6759473079877,-1.91411934749301,100.728161136767));
#57741=CARTESIAN_POINT('Ctrl Pts',(-7.67941267725341,-1.90014781325215,
100.727580198348));
#57742=CARTESIAN_POINT('Ctrl Pts',(-7.68047969603304,-1.89583027152591,
100.727400493305));
#57743=CARTESIAN_POINT('Ctrl Pts',(-7.6823337947966,-1.88830066520649,100.727086776274));
#57744=CARTESIAN_POINT('Ctrl Pts',(-7.68312250348036,-1.88508899878534,
100.726952862701));
#57745=CARTESIAN_POINT('Ctrl Pts',(-7.68464259216893,-1.87888231023703,
100.726693871579));
#57746=CARTESIAN_POINT('Ctrl Pts',(-7.68537423323436,-1.87588736339735,
100.726568810346));
#57747=CARTESIAN_POINT('Ctrl Pts',(-7.68711466754766,-1.86874484827184,
100.726270345925));
#57748=CARTESIAN_POINT('Ctrl Pts',(-7.68812185275036,-1.86459689937094,
100.726096845743));
#57749=CARTESIAN_POINT('Ctrl Pts',(-7.69115355554793,-1.85206704524543,
100.725572239546));
#57750=CARTESIAN_POINT('Ctrl Pts',(-7.69316771976651,-1.84368267048238,
100.725220511862));
#57751=CARTESIAN_POINT('Ctrl Pts',(-7.71314481190045,-1.75992116134604,
100.721699953486));
#57752=CARTESIAN_POINT('Ctrl Pts',(-7.73001248888562,-1.68428962078129,
100.718466705807));
#57753=CARTESIAN_POINT('Ctrl Pts',(-7.74862849116477,-1.59463968851177,
100.714580421355));
#57754=CARTESIAN_POINT('Ctrl Pts',(-7.75145422817076,-1.58084679034245,
100.713981007621));
#57755=CARTESIAN_POINT('Ctrl Pts',(-7.85852014414527,-1.05105067840116,
100.690901565655));
#57756=CARTESIAN_POINT('Ctrl Pts',(-7.91102681554453,-0.525965126627474,
100.66609000105));
#57757=CARTESIAN_POINT('Ctrl Pts',(-7.91098891369753,0.217733859368774,
100.631422342524));
#57758=CARTESIAN_POINT('Ctrl Pts',(-7.90202210829038,0.434976997559752,
100.621340051967));
#57759=CARTESIAN_POINT('Ctrl Pts',(-7.84520037423542,1.12252005132096,100.589872468359));
#57760=CARTESIAN_POINT('Ctrl Pts',(-7.76416035555382,1.58906817388382,100.569248301842));
#57761=CARTESIAN_POINT('Ctrl Pts',(-7.63333321063003,2.07780002494947,100.548676478644));
#57762=CARTESIAN_POINT('Ctrl Pts',(-7.62452355610278,2.10989796598658,100.547329863717));
#57763=CARTESIAN_POINT('Ctrl Pts',(-7.6126100912286,2.15225542933883,100.545558580184));
#57764=CARTESIAN_POINT('Ctrl Pts',(-7.60968770066091,2.16256535942939,100.54512789623));
#57765=CARTESIAN_POINT('Ctrl Pts',(-7.60512132096831,2.17855126444294,100.544460799971));
#57766=CARTESIAN_POINT('Ctrl Pts',(-7.60349191104736,2.18423136990829,100.544223903722));
#57767=CARTESIAN_POINT('Ctrl Pts',(-7.60021911169365,2.19559227231814,100.543750353279));
#57768=CARTESIAN_POINT('Ctrl Pts',(-7.59857571360581,2.20127306275619,100.543513699564));
#57769=CARTESIAN_POINT('Ctrl Pts',(-7.59489617636393,2.213939025482,100.542986354258));
#57770=CARTESIAN_POINT('Ctrl Pts',(-7.59285676623179,2.22092324634593,100.542695771597));
#57771=CARTESIAN_POINT('Ctrl Pts',(-7.58687704036646,2.24129707569235,100.541848698057));
#57772=CARTESIAN_POINT('Ctrl Pts',(-7.58291091225359,2.25467911388393,100.541293065586));
#57773=CARTESIAN_POINT('Ctrl Pts',(-7.55416342296259,2.35074161494049,100.537309760978));
#57774=CARTESIAN_POINT('Ctrl Pts',(-7.52806535271193,2.43302359283986,100.533926120139));
#57775=CARTESIAN_POINT('Ctrl Pts',(-7.44117717061716,2.692169128023,100.523348487333));
#57776=CARTESIAN_POINT('Ctrl Pts',(-7.37545898387805,2.86731621398184,100.516318913368));
#57777=CARTESIAN_POINT('Ctrl Pts',(-7.0972527190762,3.53571116420255,100.489755922394));
#57778=CARTESIAN_POINT('Ctrl Pts',(-6.8409701164598,4.00916287686097,100.471612824162));
#57779=CARTESIAN_POINT('Ctrl Pts',(-6.29125336167091,4.81636062961772,100.437805691332));
#57780=CARTESIAN_POINT('Ctrl Pts',(-6.01393983171896,5.1584582346803,100.42229326878));
#57781=CARTESIAN_POINT('Ctrl Pts',(-5.68853786615748,5.4977622586455,100.403662002656));
#57782=CARTESIAN_POINT('Ctrl Pts',(-5.66728086402671,5.51967213473167,100.402443582324));
#57783=CARTESIAN_POINT('Ctrl Pts',(-5.63997745995344,5.54749012492507,100.400877519969));
#57784=CARTESIAN_POINT('Ctrl Pts',(-5.63404745637223,5.55351255454037,100.400537324226));
#57785=CARTESIAN_POINT('Ctrl Pts',(-5.62460746586162,5.56306899689698,100.399995680124));
#57786=CARTESIAN_POINT('Ctrl Pts',(-5.62110376148191,5.56660922930184,100.399794627289));
#57787=CARTESIAN_POINT('Ctrl Pts',(-5.61456170068763,5.57320702015331,100.399419193729));
#57788=CARTESIAN_POINT('Ctrl Pts',(-5.61152418266586,5.57626541043042,100.399244865275));
#57789=CARTESIAN_POINT('Ctrl Pts',(-5.60477230968753,5.5830525751418,100.398857338946));
#57790=CARTESIAN_POINT('Ctrl Pts',(-5.60105673230687,5.58678012647022,100.398644065484));
#57791=CARTESIAN_POINT('Ctrl Pts',(-5.59028928004631,5.59756074019381,100.398025975019));
#57792=CARTESIAN_POINT('Ctrl Pts',(-5.58322779988125,5.60460416158775,100.397620570276));
#57793=CARTESIAN_POINT('Ctrl Pts',(-5.53480451098001,5.65272128054489,100.394840321496));
#57794=CARTESIAN_POINT('Ctrl Pts',(-5.49300384585131,5.69334939710183,100.392439166055));
#57795=CARTESIAN_POINT('Ctrl Pts',(-5.36177473005591,5.81810685244853,100.384907386279));
#57796=CARTESIAN_POINT('Ctrl Pts',(-5.27083583596546,5.90061720582818,100.379697276894));
#57797=CARTESIAN_POINT('Ctrl Pts',(-4.97600865338472,6.15586321369664,100.362923665834));
#57798=CARTESIAN_POINT('Ctrl Pts',(-4.76527492016384,6.32040044497628,100.351111917005));
#57799=CARTESIAN_POINT('Ctrl Pts',(-4.3405024610174,6.61871607962593,100.328090856406));
#57800=CARTESIAN_POINT('Ctrl Pts',(-4.12757841522293,6.75355195359641,100.31689862308));
#57801=CARTESIAN_POINT('Ctrl Pts',(-3.4884110280167,7.11677358936094,100.284645966265));
#57802=CARTESIAN_POINT('Ctrl Pts',(-3.04721746686609,7.31655764942556,100.264100636953));
#57803=CARTESIAN_POINT('Ctrl Pts',(-2.56117772095599,7.48500191762332,100.243268466401));
#57804=CARTESIAN_POINT('Ctrl Pts',(-2.53178106810832,7.49499630868627,100.242014864729));
#57805=CARTESIAN_POINT('Ctrl Pts',(-2.49072378741304,7.50868600998582,100.240272667893));
#57806=CARTESIAN_POINT('Ctrl Pts',(-2.47911240445294,7.51252768839941,100.239780920752));
#57807=CARTESIAN_POINT('Ctrl Pts',(-2.45904707462449,7.51911480760394,100.238932789674));
#57808=CARTESIAN_POINT('Ctrl Pts',(-2.45059733485904,7.52187295212698,100.238576134571));
#57809=CARTESIAN_POINT('Ctrl Pts',(-2.4331304482501,7.52754189645614,100.237839904728));
#57810=CARTESIAN_POINT('Ctrl Pts',(-2.42411267685445,7.53045075089275,100.237460371161));
#57811=CARTESIAN_POINT('Ctrl Pts',(-2.40317266166712,7.53716384123068,100.236580371915));
#57812=CARTESIAN_POINT('Ctrl Pts',(-2.39124656175302,7.5409560065983,100.236080164084));
#57813=CARTESIAN_POINT('Ctrl Pts',(-2.35345110416821,7.55287522535579,100.234498040935));
#57814=CARTESIAN_POINT('Ctrl Pts',(-2.32754885274308,7.56089760676024,100.233418368921));
#57815=CARTESIAN_POINT('Ctrl Pts',(-1.84952057948756,7.70626207151502,100.213576909518));
#57816=CARTESIAN_POINT('Ctrl Pts',(-1.38601637328704,7.80296139722256,100.195802078976));
#57817=CARTESIAN_POINT('Ctrl Pts',(-0.271320596930701,7.93299374670284,
100.154764227382));
#57818=CARTESIAN_POINT('Ctrl Pts',(0.380732266471482,7.92848616729232,100.132170235629));
#57819=CARTESIAN_POINT('Ctrl Pts',(1.09092546501898,7.8357033645753,100.104154546035));
#57820=CARTESIAN_POINT('Ctrl Pts',(1.15691834915784,7.82623186274593,100.101516249931));
#57821=CARTESIAN_POINT('Ctrl Pts',(1.23369796513583,7.81421988423362,100.098398743971));
#57822=CARTESIAN_POINT('Ctrl Pts',(1.2446100124443,7.81248929493555,100.097954546016));
#57823=CARTESIAN_POINT('Ctrl Pts',(1.26101037227166,7.80985305768122,100.097285188924));
#57824=CARTESIAN_POINT('Ctrl Pts',(1.26650144289608,7.80896446633357,100.097060784342));
#57825=CARTESIAN_POINT('Ctrl Pts',(1.27627339036216,7.80737254482427,100.096660901859));
#57826=CARTESIAN_POINT('Ctrl Pts',(1.28055463843317,7.8066714826806,100.096485525548));
#57827=CARTESIAN_POINT('Ctrl Pts',(1.28955818251721,7.80518953029417,100.096116320886));
#57828=CARTESIAN_POINT('Ctrl Pts',(1.29428034944928,7.80440787547584,100.095922458047));
#57829=CARTESIAN_POINT('Ctrl Pts',(1.30670112901621,7.80234029517795,100.095411945606));
#57830=CARTESIAN_POINT('Ctrl Pts',(1.31439853977679,7.80104726304728,100.095094971715));
#57831=CARTESIAN_POINT('Ctrl Pts',(1.34867588245901,7.79523708826217,100.093680742644));
#57832=CARTESIAN_POINT('Ctrl Pts',(1.37523429381286,7.79059551681751,100.092577716693));
#57833=CARTESIAN_POINT('Ctrl Pts',(1.56200759307776,7.75696862496428,100.084766542404));
#57834=CARTESIAN_POINT('Ctrl Pts',(1.72129906038946,7.72318250001323,100.07780818696));
#57835=CARTESIAN_POINT('Ctrl Pts',(2.25330803439449,7.59306781266034,100.053800174322));
#57836=CARTESIAN_POINT('Ctrl Pts',(2.6200104509564,7.47446309144602,100.036001483499));
#57837=CARTESIAN_POINT('Ctrl Pts',(3.44424906383342,7.13973567394389,99.9949966121014));
#57838=CARTESIAN_POINT('Ctrl Pts',(3.89268937192721,6.90548663796145,99.9719819802656));
#57839=CARTESIAN_POINT('Ctrl Pts',(4.47866573998773,6.52405147965715,99.9421302858493));
#57840=CARTESIAN_POINT('Ctrl Pts',(4.63759468630427,6.41205249657729,99.934045434477));
#57841=CARTESIAN_POINT('Ctrl Pts',(4.80713027099167,6.28297457861285,99.9254324633464));
#57842=CARTESIAN_POINT('Ctrl Pts',(4.82197510311782,6.27158888233892,99.9246783729532));
#57843=CARTESIAN_POINT('Ctrl Pts',(4.84277771869976,6.25551615968285,99.9236217232832));
#57844=CARTESIAN_POINT('Ctrl Pts',(4.84876930861334,6.25087311093805,99.9233173959582));
#57845=CARTESIAN_POINT('Ctrl Pts',(4.85915829190651,6.24279847558177,99.9227897296545));
#57846=CARTESIAN_POINT('Ctrl Pts',(4.86355874150425,6.23937084012838,99.9225662314126));
#57847=CARTESIAN_POINT('Ctrl Pts',(4.87261443890336,6.23230169853359,99.9221063025599));
#57848=CARTESIAN_POINT('Ctrl Pts',(4.87726923921309,6.22865962307974,99.9218698952015));
#57849=CARTESIAN_POINT('Ctrl Pts',(4.88816527876279,6.22011448450788,99.9213165184604));
#57850=CARTESIAN_POINT('Ctrl Pts',(4.8944032348228,6.21520723454384,99.9209997191926));
#57851=CARTESIAN_POINT('Ctrl Pts',(4.90754525431525,6.20483666910452,99.9203323045868));
#57852=CARTESIAN_POINT('Ctrl Pts',(4.91444760642111,6.19937119696953,99.9199817775487));
#57853=CARTESIAN_POINT('Ctrl Pts',(4.9329402264708,6.18467793886277,99.9190426676083));
#57854=CARTESIAN_POINT('Ctrl Pts',(4.94451374657122,6.17542907808645,99.9184549447598));
#57855=CARTESIAN_POINT('Ctrl Pts',(5.21982013822596,5.95415067181425,99.9044744998658));
#57856=CARTESIAN_POINT('Ctrl Pts',(5.46971662557255,5.72543998247453,99.8918085124557));
#57857=CARTESIAN_POINT('Ctrl Pts',(6.24134696630462,4.92244433237357,99.8518663506104));
#57858=CARTESIAN_POINT('Ctrl Pts',(6.69332862510937,4.28765573010511,99.8274158127032));
#57859=CARTESIAN_POINT('Ctrl Pts',(7.13955321567155,3.41368341028276,99.7916598837286));
#57860=CARTESIAN_POINT('Ctrl Pts',(7.2261101768101,3.22641821892297,99.7838618870723));
#57861=CARTESIAN_POINT('Ctrl Pts',(7.31004807840962,3.0244461688235,99.7751015101087));
#57862=CARTESIAN_POINT('Ctrl Pts',(7.31482215439826,3.01288140869288,99.7745987019441));
#57863=CARTESIAN_POINT('Ctrl Pts',(7.32128166379366,2.99712798934742,99.7739120949657));
#57864=CARTESIAN_POINT('Ctrl Pts',(7.32299099783204,2.99294908587488,99.7737297978207));
#57865=CARTESIAN_POINT('Ctrl Pts',(7.3258862654845,2.98585353600751,99.7734199902282));
#57866=CARTESIAN_POINT('Ctrl Pts',(7.32707403849465,2.98293763724927,99.7732925961569));
#57867=CARTESIAN_POINT('Ctrl Pts',(7.32937048147655,2.97729038467326,99.7730457160712));
#57868=CARTESIAN_POINT('Ctrl Pts',(7.33047936282902,2.97455912708031,99.7729262442863));
#57869=CARTESIAN_POINT('Ctrl Pts',(7.33311572869248,2.96805513364818,99.7726415789999));
#57870=CARTESIAN_POINT('Ctrl Pts',(7.33464182741804,2.96428184053807,99.772476298312));
#57871=CARTESIAN_POINT('Ctrl Pts',(7.3391630799882,2.95307813432367,99.7719851570559));
#57872=CARTESIAN_POINT('Ctrl Pts',(7.34214985165806,2.94564436702189,99.7716587739686));
#57873=CARTESIAN_POINT('Ctrl Pts',(7.36598969705877,2.88604791739027,99.769038192788));
#57874=CARTESIAN_POINT('Ctrl Pts',(7.38629743357124,2.83367018607658,99.7667106857001));
#57875=CARTESIAN_POINT('Ctrl Pts',(7.49688445954315,2.53917597906776,99.7535080186805));
#57876=CARTESIAN_POINT('Ctrl Pts',(7.57581090604522,2.29298081468585,99.7420371661199));
#57877=CARTESIAN_POINT('Ctrl Pts',(7.7446870897463,1.66136070277169,99.7123228657999));
#57878=CARTESIAN_POINT('Ctrl Pts',(7.81804112351122,1.27221624981311,99.6937804089862));
#57879=CARTESIAN_POINT('Ctrl Pts',(7.88914287150531,0.636421606287519,99.6644236750676));
#57880=CARTESIAN_POINT('Ctrl Pts',(7.90503448577778,0.392489546487242,99.6533715694086));
#57881=CARTESIAN_POINT('Ctrl Pts',(7.91552880907088,-0.167596809893812,
99.6287048777381));
#57882=CARTESIAN_POINT('Ctrl Pts',(7.90252856392297,-0.483485702841372,
99.6153170579792));
#57883=CARTESIAN_POINT('Ctrl Pts',(7.86854159552577,-0.818791939995101,
99.6016914699375));
#57884=CARTESIAN_POINT('Ctrl Pts',(7.86632754754467,-0.839796407199824,
99.6008403105791));
#57885=CARTESIAN_POINT('Ctrl Pts',(7.86316473365714,-0.868691268266269,
99.5996726542763));
#57886=CARTESIAN_POINT('Ctrl Pts',(7.86228816642209,-0.87658937753575,99.5993538213362));
#57887=CARTESIAN_POINT('Ctrl Pts',(7.86076852500718,-0.890096099282285,
99.5988091466243));
#57888=CARTESIAN_POINT('Ctrl Pts',(7.86013134593871,-0.895705361421367,
99.5985831140884));
#57889=CARTESIAN_POINT('Ctrl Pts',(7.85882727334779,-0.907076918639451,
99.5981252211192));
#57890=CARTESIAN_POINT('Ctrl Pts',(7.8581600450813,-0.912839172431544,99.5978933716748));
#57891=CARTESIAN_POINT('Ctrl Pts',(7.85666658519136,-0.925613864363987,
99.5973797602184));
#57892=CARTESIAN_POINT('Ctrl Pts',(7.85583730131153,-0.932625944540598,
99.5970980972742));
#57893=CARTESIAN_POINT('Ctrl Pts',(7.85404800477728,-0.947583766617605,
99.5964978208854));
#57894=CARTESIAN_POINT('Ctrl Pts',(7.8530853194676,-0.955529184149296,99.5961792942968));
#57895=CARTESIAN_POINT('Ctrl Pts',(7.85053371720083,-0.976324224779369,
99.5953465017483));
#57896=CARTESIAN_POINT('Ctrl Pts',(7.84892530663879,-0.989171456168629,
99.5948328672741));
#57897=CARTESIAN_POINT('Ctrl Pts',(7.84406618424682,-1.02722570745312,99.5933139955531));
#57898=CARTESIAN_POINT('Ctrl Pts',(7.8407255165817,-1.05242118288927,99.5923116698681));
#57899=CARTESIAN_POINT('Ctrl Pts',(7.80414095386732,-1.31849651984598,99.5817608905861));
#57900=CARTESIAN_POINT('Ctrl Pts',(7.7599282718119,-1.55774650110608,99.5725765794849));
#57901=CARTESIAN_POINT('Ctrl Pts',(7.62382272278114,-2.14209092537623,99.5506371570535));
#57902=CARTESIAN_POINT('Ctrl Pts',(7.51946514300476,-2.48372432936004,99.5382572869988));
#57903=CARTESIAN_POINT('Ctrl Pts',(7.1751619024553,-3.3871986679991,99.5051024354206));
#57904=CARTESIAN_POINT('Ctrl Pts',(6.89274652289731,-3.93012949201877,99.4847860442526));
#57905=CARTESIAN_POINT('Ctrl Pts',(6.5399624588176,-4.45120071478618,99.4600034720082));
#57906=CARTESIAN_POINT('Ctrl Pts',(6.52903593324065,-4.4672123899258,99.4592362668394));
#57907=CARTESIAN_POINT('Ctrl Pts',(6.50591298124005,-4.50083059243569,99.4576131019517));
#57908=CARTESIAN_POINT('Ctrl Pts',(6.49370370174506,-4.51842804064291,99.4567562829169));
#57909=CARTESIAN_POINT('Ctrl Pts',(6.4778103344398,-4.54113796032228,99.4556409312745));
#57910=CARTESIAN_POINT('Ctrl Pts',(6.4741912973672,-4.54629604718704,99.4553869572314));
#57911=CARTESIAN_POINT('Ctrl Pts',(6.46861538554569,-4.55422303909627,99.4549956499527));
#57912=CARTESIAN_POINT('Ctrl Pts',(6.4666629040217,-4.55699499469011,99.4548586278604));
#57913=CARTESIAN_POINT('Ctrl Pts',(6.4627949933157,-4.56247881063084,99.4545871843959));
#57914=CARTESIAN_POINT('Ctrl Pts',(6.46087963747219,-4.56519072253496,99.4544527681612));
#57915=CARTESIAN_POINT('Ctrl Pts',(6.45662406367177,-4.57120805727374,99.4541541216499));
#57916=CARTESIAN_POINT('Ctrl Pts',(6.45428301498237,-4.57451288826081,99.4539898335175));
#57917=CARTESIAN_POINT('Ctrl Pts',(6.44757153365971,-4.58397199972684,99.453518848336));
#57918=CARTESIAN_POINT('Ctrl Pts',(6.44319483941243,-4.59012181064578,99.4532117183186));
#57919=CARTESIAN_POINT('Ctrl Pts',(6.41503966310326,-4.62956379232805,99.4512360680225));
#57920=CARTESIAN_POINT('Ctrl Pts',(6.39101241269682,-4.6626768077657,99.4495505791869));
#57921=CARTESIAN_POINT('Ctrl Pts',(6.31768939550816,-4.76209492282766,99.4444124328677));
#57922=CARTESIAN_POINT('Ctrl Pts',(6.26761176420726,-4.827814132025,99.4409104506965));
#57923=CARTESIAN_POINT('Ctrl Pts',(6.11762108727093,-5.01838635958545,99.4304726699977));
#57924=CARTESIAN_POINT('Ctrl Pts',(6.01494369595003,-5.14100548211801,99.4233919433543));
#57925=CARTESIAN_POINT('Ctrl Pts',(5.85849568780882,-5.31673141549757,99.4127982282299));
#57926=CARTESIAN_POINT('Ctrl Pts',(5.80756328980176,-5.37231914584692,99.4093777565908));
#57927=CARTESIAN_POINT('Ctrl Pts',(5.71588497968593,-5.46954959330668,99.4032823619629));
#57928=CARTESIAN_POINT('Ctrl Pts',(5.67545848518531,-5.51148661822496,99.4006149083414));
#57929=CARTESIAN_POINT('Ctrl Pts',(5.53958396480704,-5.64935778658685,99.3917261557212));
#57930=CARTESIAN_POINT('Ctrl Pts',(5.44213811231875,-5.74328880260512,99.3854748160144));
#57931=CARTESIAN_POINT('Ctrl Pts',(5.319697986479,-5.85539717556687,99.3778078028305));
#57932=CARTESIAN_POINT('Ctrl Pts',(5.29694400311783,-5.87598902149385,99.3763906445448));
#57933=CARTESIAN_POINT('Ctrl Pts',(5.25254054486855,-5.91570564121164,99.3736405720194));
#57934=CARTESIAN_POINT('Ctrl Pts',(5.23090498330669,-5.9348452775191,99.37230761675));
#57935=CARTESIAN_POINT('Ctrl Pts',(5.18861773342125,-5.97184329935418,99.3697164283078));
#57936=CARTESIAN_POINT('Ctrl Pts',(5.16797745524289,-5.98971413359468,99.3684581240923));
#57937=CARTESIAN_POINT('Ctrl Pts',(5.1275820444983,-6.02432517757995,99.3660084056036));
#57938=CARTESIAN_POINT('Ctrl Pts',(5.10783640679561,-6.04107595670407,99.3648169031677));
#57939=CARTESIAN_POINT('Ctrl Pts',(4.80785530833912,-6.29303611408109,99.3468074680148));
#57940=CARTESIAN_POINT('Ctrl Pts',(4.51169882551256,-6.50863936762877,99.3302694052976));
#57941=CARTESIAN_POINT('Ctrl Pts',(3.98985185790774,-6.83575120035174,99.3036202952102));
#57942=CARTESIAN_POINT('Ctrl Pts',(3.77185765655132,-6.95841340132563,99.2931406400967));
#57943=CARTESIAN_POINT('Ctrl Pts',(3.53014048909022,-7.07972081224955,99.2822028599964));
#57944=CARTESIAN_POINT('Ctrl Pts',(3.51183954113399,-7.08881666412164,99.2813788016947));
#57945=CARTESIAN_POINT('Ctrl Pts',(3.4856733465493,-7.10169546549257,99.280206338258));
#57946=CARTESIAN_POINT('Ctrl Pts',(3.47783684264528,-7.10553643717401,99.2798559312727));
#57947=CARTESIAN_POINT('Ctrl Pts',(3.46441424037888,-7.11208784545819,99.2792569942295));
#57948=CARTESIAN_POINT('Ctrl Pts',(3.45883128573846,-7.11480468371943,99.2790082438401));
#57949=CARTESIAN_POINT('Ctrl Pts',(3.44764800449408,-7.12023053976132,99.2785107068077));
#57950=CARTESIAN_POINT('Ctrl Pts',(3.44204766931522,-7.12293952976081,99.2782619212313));
#57951=CARTESIAN_POINT('Ctrl Pts',(3.43076228383155,-7.12838207055006,99.2777613292051));
#57952=CARTESIAN_POINT('Ctrl Pts',(3.42507714766687,-7.13111543341331,99.2775095293181));
#57953=CARTESIAN_POINT('Ctrl Pts',(3.40442249326649,-7.14101560960262,99.2765960869383));
#57954=CARTESIAN_POINT('Ctrl Pts',(3.38943365237568,-7.14814213412406,99.2759358251418));
#57955=CARTESIAN_POINT('Ctrl Pts',(3.21965351888269,-7.22821091951527,99.2684862663342));
#57956=CARTESIAN_POINT('Ctrl Pts',(3.06255245716724,-7.29616191113857,99.261869431837));
#57957=CARTESIAN_POINT('Ctrl Pts',(2.61090898559797,-7.47435074683545,99.2435334435158));
#57958=CARTESIAN_POINT('Ctrl Pts',(2.3118249078126,-7.57220227122811,99.2322081383494));
#57959=CARTESIAN_POINT('Ctrl Pts',(1.3467074025626,-7.82542558847317,99.1971158273906));
#57960=CARTESIAN_POINT('Ctrl Pts',(0.666120213178818,-7.91245681984313,
99.1746722991833));
#57961=CARTESIAN_POINT('Ctrl Pts',(-0.098538931491644,-7.91080566486328,
99.1451680353399));
#57962=CARTESIAN_POINT('Ctrl Pts',(-0.179985399648391,-7.90937169722905,
99.1419682129775));
#57963=CARTESIAN_POINT('Ctrl Pts',(-0.271393606983445,-7.90634976698278,
99.1382990547919));
#57964=CARTESIAN_POINT('Ctrl Pts',(-0.281393852452829,-7.90600016607141,
99.1378965928149));
#57965=CARTESIAN_POINT('Ctrl Pts',(-0.29560068183747,-7.90547651710202,
99.1373233139094));
#57966=CARTESIAN_POINT('Ctrl Pts',(-0.299807865784511,-7.90531808145919,
99.1371533544922));
#57967=CARTESIAN_POINT('Ctrl Pts',(-0.307521790600614,-7.90502142088696,
99.1368413808688));
#57968=CARTESIAN_POINT('Ctrl Pts',(-0.311028574181621,-7.90488422068152,
99.1366994233292));
#57969=CARTESIAN_POINT('Ctrl Pts',(-0.318159174690539,-7.90460048915112,
99.1364104982692));
#57970=CARTESIAN_POINT('Ctrl Pts',(-0.321782981055823,-7.90445379938105,
99.1362635221709));
#57971=CARTESIAN_POINT('Ctrl Pts',(-0.330788520227108,-7.90408305676143,
99.135897918106));
#57972=CARTESIAN_POINT('Ctrl Pts',(-0.336170120865733,-7.90385599962892,
99.1356791242157));
#57973=CARTESIAN_POINT('Ctrl Pts',(-0.356283091097092,-7.90298682681752,
99.1348602529049));
#57974=CARTESIAN_POINT('Ctrl Pts',(-0.371012810324826,-7.90230902427222,
99.1342582268371));
#57975=CARTESIAN_POINT('Ctrl Pts',(-0.740791280567599,-7.88425714921521,
99.119087924579));
#57976=CARTESIAN_POINT('Ctrl Pts',(-1.09424116330351,-7.84301433389644,
99.1032839521145));
#57977=CARTESIAN_POINT('Ctrl Pts',(-1.52769732588647,-7.76256165084227,
99.0832370562986));
#57978=CARTESIAN_POINT('Ctrl Pts',(-1.61145246815014,-7.74560799526967,
99.0793312559627));
#57979=CARTESIAN_POINT('Ctrl Pts',(-1.76458597635585,-7.71201950140238,
99.0721471778858));
#57980=CARTESIAN_POINT('Ctrl Pts',(-1.83404613116639,-7.6957964630024,99.0688721675812));
#57981=CARTESIAN_POINT('Ctrl Pts',(-2.14685899130905,-7.618260614275,99.0540703182836));
#57982=CARTESIAN_POINT('Ctrl Pts',(-2.38743541568688,-7.54632731602424,
99.0425470344009));
#57983=CARTESIAN_POINT('Ctrl Pts',(-2.77057569825167,-7.41160641280549,
99.0242225481883));
#57984=CARTESIAN_POINT('Ctrl Pts',(-2.91541930951471,-7.35583661023385,
99.0173002280066));
#57985=CARTESIAN_POINT('Ctrl Pts',(-3.35057297761001,-7.17341324995474,
98.9965870539977));
#57986=CARTESIAN_POINT('Ctrl Pts',(-3.63501578979728,-7.03355436400988,
98.983177140739));
#57987=CARTESIAN_POINT('Ctrl Pts',(-3.9291347920294,-6.86631550834635,98.9694867559329));
#57988=CARTESIAN_POINT('Ctrl Pts',(-3.94789419339772,-6.85554668290083,
98.9686142699369));
#57989=CARTESIAN_POINT('Ctrl Pts',(-3.97434578211093,-6.8402175812297,98.9673849938465));
#57990=CARTESIAN_POINT('Ctrl Pts',(-3.98207468439408,-6.83572104191864,
98.9670259283266));
#57991=CARTESIAN_POINT('Ctrl Pts',(-3.99519676543901,-6.82805703872501,
98.9664165050521));
#57992=CARTESIAN_POINT('Ctrl Pts',(-4.00059383327869,-6.82489627027542,
98.9661659077507));
#57993=CARTESIAN_POINT('Ctrl Pts',(-4.0113146395125,-6.81860059194601,98.9656682287564));
#57994=CARTESIAN_POINT('Ctrl Pts',(-4.01663846502505,-6.8154658396295,98.965421141666));
#57995=CARTESIAN_POINT('Ctrl Pts',(-4.0293752111622,-6.80794613570203,98.9648301378263));
#57996=CARTESIAN_POINT('Ctrl Pts',(-4.03678466090763,-6.80355530447192,
98.9644864328149));
#57997=CARTESIAN_POINT('Ctrl Pts',(-4.06202747552514,-6.78854068858828,
98.9633158335948));
#57998=CARTESIAN_POINT('Ctrl Pts',(-4.07982625955739,-6.77785877639054,
98.9624910358902));
#57999=CARTESIAN_POINT('Ctrl Pts',(-4.44833205168706,-6.55472309196552,
98.9454261307017));
#58000=CARTESIAN_POINT('Ctrl Pts',(-4.78205177830485,-6.31538444416365,
98.9302408317226));
#58001=CARTESIAN_POINT('Ctrl Pts',(-5.6396114194999,-5.59323335150966,98.8904533757213));
#58002=CARTESIAN_POINT('Ctrl Pts',(-6.11918817126435,-5.0640708433679,98.8674850588575));
#58003=CARTESIAN_POINT('Ctrl Pts',(-6.60913177132474,-4.35054227799108,
98.8351870114317));
#58004=CARTESIAN_POINT('Ctrl Pts',(-6.69291548296431,-4.22051159831969,
98.8292415453167));
#58005=CARTESIAN_POINT('Ctrl Pts',(-6.77883859686389,-4.07816177656102,
98.8225807160462));
#58006=CARTESIAN_POINT('Ctrl Pts',(-6.78482526762402,-4.06819398299678,
98.8221135171696));
#58007=CARTESIAN_POINT('Ctrl Pts',(-6.79308466360197,-4.0543731653533,98.8214645874316));
#58008=CARTESIAN_POINT('Ctrl Pts',(-6.79537615361268,-4.05053131595882,
98.8212840795219));
#58009=CARTESIAN_POINT('Ctrl Pts',(-6.79930657072544,-4.04392896374125,
98.8209736586407));
#58010=CARTESIAN_POINT('Ctrl Pts',(-6.80094708032332,-4.04116939970067,
98.8208438495583));
#58011=CARTESIAN_POINT('Ctrl Pts',(-6.80414612212475,-4.03578070392252,
98.8205902415996));
#58012=CARTESIAN_POINT('Ctrl Pts',(-6.8057048110604,-4.0331516666281,98.8204664531762));
#58013=CARTESIAN_POINT('Ctrl Pts',(-6.80944599912511,-4.02683306845275,
98.8201688002715));
#58014=CARTESIAN_POINT('Ctrl Pts',(-6.81162702197271,-4.0231426384842,98.8199948380175));
#58015=CARTESIAN_POINT('Ctrl Pts',(-6.81828733685086,-4.01185201860703,
98.8194622535595));
#58016=CARTESIAN_POINT('Ctrl Pts',(-6.82275689610632,-4.00424614154016,
98.8191029826965));
#58017=CARTESIAN_POINT('Ctrl Pts',(-6.8710693211684,-3.92171685672283,98.8151993889385));
#58018=CARTESIAN_POINT('Ctrl Pts',(-6.91368736612001,-3.84608666870855,
98.8115753563138));
#58019=CARTESIAN_POINT('Ctrl Pts',(-7.08479923543061,-3.53039348504515,
98.7963088409027));
#58020=CARTESIAN_POINT('Ctrl Pts',(-7.20209468422893,-3.28448942377354,
98.7840941466115));
#58021=CARTESIAN_POINT('Ctrl Pts',(-7.63002497484085,-2.2536250589279,98.7330514647578));
#58022=CARTESIAN_POINT('Ctrl Pts',(-7.82686484827529,-1.42719750252555,
98.6932871739802));
#58023=CARTESIAN_POINT('Ctrl Pts',(-7.89183441038454,-0.551383313984055,
98.6570776901287));
#58024=CARTESIAN_POINT('Ctrl Pts',(-7.89412831978794,-0.517505584026996,
98.6556846913589));
#58025=CARTESIAN_POINT('Ctrl Pts',(-7.89904588043883,-0.43721412235109,
98.6524011691919));
#58026=CARTESIAN_POINT('Ctrl Pts',(-7.90147868979835,-0.39078974393681,
98.650516831017));
#58027=CARTESIAN_POINT('Ctrl Pts',(-7.90402390803983,-0.33237136883006,
98.6481631937581));
#58028=CARTESIAN_POINT('Ctrl Pts',(-7.90451841767839,-0.320395461818897,
98.6476816180501));
#58029=CARTESIAN_POINT('Ctrl Pts',(-7.90525422919175,-0.30153608536691,
98.6469246929327));
#58030=CARTESIAN_POINT('Ctrl Pts',(-7.90551376135401,-0.294653369731292,
98.6466487574776));
#58031=CARTESIAN_POINT('Ctrl Pts',(-7.90595820000235,-0.282443537613245,
98.6461597892126));
#58032=CARTESIAN_POINT('Ctrl Pts',(-7.9061467114931,-0.277116561429293,
98.6459466406075));
#58033=CARTESIAN_POINT('Ctrl Pts',(-7.9065201654134,-0.266252819273748,
98.6455123177222));
#58034=CARTESIAN_POINT('Ctrl Pts',(-7.90670467616242,-0.260716040888589,
98.6452911574367));
#58035=CARTESIAN_POINT('Ctrl Pts',(-7.90709860651436,-0.248509861907359,
98.6448040246742));
#58036=CARTESIAN_POINT('Ctrl Pts',(-7.90730540428417,-0.241840377672786,
98.6445381366036));
#58037=CARTESIAN_POINT('Ctrl Pts',(-7.90779464743842,-0.225389802611338,
98.6438830058172));
#58038=CARTESIAN_POINT('Ctrl Pts',(-7.90806738453865,-0.215608422095326,
98.6434940751755));
#58039=CARTESIAN_POINT('Ctrl Pts',(-7.91010476584352,-0.13732761564452,
98.6403862582804));
#58040=CARTESIAN_POINT('Ctrl Pts',(-7.91099753799733,-0.0688075858804266,
98.637695474162));
#58041=CARTESIAN_POINT('Ctrl Pts',(-7.91099999491492,-0.00028364795766521,
98.635032539653));
#58042=CARTESIAN_POINT('',(-7.91859353182819,-0.00199197810995972,94.6422060731203));
#58043=CARTESIAN_POINT('Ctrl Pts',(-7.91099999474075,-0.000288464720890058,
98.6350327268391));
#58044=CARTESIAN_POINT('Ctrl Pts',(-7.91103062328953,0.839684092487076,
98.6023902214954));
#58045=CARTESIAN_POINT('Ctrl Pts',(-7.77730583138597,1.67422711870364,98.5749578136994));
#58046=CARTESIAN_POINT('Ctrl Pts',(-7.42655689965386,2.74042479551888,98.5358029537483));
#58047=CARTESIAN_POINT('Ctrl Pts',(-7.32400907867107,3.00375520449944,98.5256894808569));
#58048=CARTESIAN_POINT('Ctrl Pts',(-7.17009196186592,3.34394782886831,98.5113637873219));
#58049=CARTESIAN_POINT('Ctrl Pts',(-7.13114478758396,3.42621929651382,98.5077975022605));
#58050=CARTESIAN_POINT('Ctrl Pts',(-7.08685851709105,3.51574115993614,98.5037849221163));
#58051=CARTESIAN_POINT('Ctrl Pts',(-7.08291546091925,3.52367820851707,98.5034280145292));
#58052=CARTESIAN_POINT('Ctrl Pts',(-7.07706555912408,3.53540408767884,98.5028990067856));
#58053=CARTESIAN_POINT('Ctrl Pts',(-7.0751689790302,3.53919806020053,98.5027275757076));
#58054=CARTESIAN_POINT('Ctrl Pts',(-7.07193735667936,3.5456497103934,98.5024355984758));
#58055=CARTESIAN_POINT('Ctrl Pts',(-7.07060386268146,3.54830816905994,98.5023151540936));
#58056=CARTESIAN_POINT('Ctrl Pts',(-7.06788346172296,3.55372394789592,98.5020695147125));
#58057=CARTESIAN_POINT('Ctrl Pts',(-7.06649644473882,3.55648119955044,98.5019443123776));
#58058=CARTESIAN_POINT('Ctrl Pts',(-7.06318139287089,3.56306159715924,98.5016451642826));
#58059=CARTESIAN_POINT('Ctrl Pts',(-7.0612518713527,3.56688398227045,98.5014711204842));
#58060=CARTESIAN_POINT('Ctrl Pts',(-7.05540317668943,3.57844691037621,98.5009437962916));
#58061=CARTESIAN_POINT('Ctrl Pts',(-7.05147438489161,3.58618254889646,98.5005898853308));
#58062=CARTESIAN_POINT('Ctrl Pts',(-7.01156596432635,3.66444154128579,98.4969981625974));
#58063=CARTESIAN_POINT('Ctrl Pts',(-6.9745434661366,3.73442521569144,98.4936930956724));
#58064=CARTESIAN_POINT('Ctrl Pts',(-6.93233398209062,3.81139618049242,98.4899642829674));
#58065=CARTESIAN_POINT('Ctrl Pts',(-6.92817747305319,3.81894647577177,98.4895975027331));
#58066=CARTESIAN_POINT('Ctrl Pts',(-6.92361816357868,3.8271965166025,98.4891956367143));
#58067=CARTESIAN_POINT('Ctrl Pts',(-6.92322757148096,3.82790303498091,98.4891612128658));
#58068=CARTESIAN_POINT('Ctrl Pts',(-6.91927544433564,3.83504921470213,98.4888129392829));
#58069=CARTESIAN_POINT('Ctrl Pts',(-6.91570504349921,3.84148394562412,98.4884986098132));
#58070=CARTESIAN_POINT('Ctrl Pts',(-6.90845613855813,3.85450537654047,98.4878610651518));
#58071=CARTESIAN_POINT('Ctrl Pts',(-6.9047771806402,3.86109181465925,98.4875378259152));
#58072=CARTESIAN_POINT('Ctrl Pts',(-6.89679718717741,3.87533051689597,98.4868374131411));
#58073=CARTESIAN_POINT('Ctrl Pts',(-6.89249282852016,3.88298089926368,98.4864600657942));
#58074=CARTESIAN_POINT('Ctrl Pts',(-6.88509922021377,3.89607095178625,98.4858126864471));
#58075=CARTESIAN_POINT('Ctrl Pts',(-6.88201622828243,3.90151416335293,98.4855429756838));
#58076=CARTESIAN_POINT('Ctrl Pts',(-6.8654389046754,3.93070165934789,98.4840940107957));
#58077=CARTESIAN_POINT('Ctrl Pts',(-6.85182825999647,3.95437938945336,98.482908878132));
#58078=CARTESIAN_POINT('Ctrl Pts',(-6.82567006959681,3.99934490832982,98.4806404255342));
#58079=CARTESIAN_POINT('Ctrl Pts',(-6.8131448212225,4.02064537357291,98.4795581668644));
#58080=CARTESIAN_POINT('Ctrl Pts',(-6.77045281847062,4.09247515225899,98.4758834363703));
#58081=CARTESIAN_POINT('Ctrl Pts',(-6.7398225072289,4.14272574171468,98.4732704293331));
#58082=CARTESIAN_POINT('Ctrl Pts',(-6.30489273367682,4.83865783395751,98.436538955058));
#58083=CARTESIAN_POINT('Ctrl Pts',(-5.80994425430318,5.4230138527528,98.3995968292326));
#58084=CARTESIAN_POINT('Ctrl Pts',(-5.1406475965354,6.01455679953584,98.3600487731515));
#58085=CARTESIAN_POINT('Ctrl Pts',(-5.04014193459184,6.0990263652341,98.3543235445333));
#58086=CARTESIAN_POINT('Ctrl Pts',(-4.82746261223385,6.26892245021479,98.3426536058549));
#58087=CARTESIAN_POINT('Ctrl Pts',(-4.71501325342544,6.35393081206213,98.3367259783309));
#58088=CARTESIAN_POINT('Ctrl Pts',(-4.54076388835753,6.47848351235244,98.3279001669359));
#58089=CARTESIAN_POINT('Ctrl Pts',(-4.48058964161118,6.52024555994305,98.3249148271406));
#58090=CARTESIAN_POINT('Ctrl Pts',(-4.40879917934463,6.56860625310678,98.3214251338252));
#58091=CARTESIAN_POINT('Ctrl Pts',(-4.39773656800285,6.57601789785428,98.3208893781535));
#58092=CARTESIAN_POINT('Ctrl Pts',(-4.38178586962855,6.58664617471966,98.3201197451903));
#58093=CARTESIAN_POINT('Ctrl Pts',(-4.37691287415178,6.58988535033082,98.3198850012067));
#58094=CARTESIAN_POINT('Ctrl Pts',(-4.36732289497881,6.5962446676921,98.3194237771986));
#58095=CARTESIAN_POINT('Ctrl Pts',(-4.3626061509536,6.59936516317258,98.3191972836696));
#58096=CARTESIAN_POINT('Ctrl Pts',(-4.35321797362151,6.605561714071,98.3187471771981));
#58097=CARTESIAN_POINT('Ctrl Pts',(-4.34854661675347,6.60863787828811,98.3185235601602));
#58098=CARTESIAN_POINT('Ctrl Pts',(-4.33748690415214,6.61590407454525,98.3179949508565));
#58099=CARTESIAN_POINT('Ctrl Pts',(-4.33109572772815,6.62008981547634,98.3176901225879));
#58100=CARTESIAN_POINT('Ctrl Pts',(-4.30874384170872,6.63468240026392,98.3166262870595));
#58101=CARTESIAN_POINT('Ctrl Pts',(-4.29275154692513,6.64504087337539,98.3158691223763));
#58102=CARTESIAN_POINT('Ctrl Pts',(-4.10150413376521,6.7679364453558,98.3068614933759));
#58103=CARTESIAN_POINT('Ctrl Pts',(-3.92190203461756,6.87357200238294,98.2988760650579));
#58104=CARTESIAN_POINT('Ctrl Pts',(-3.53496792098419,7.08104296237951,98.2825184857444));
#58105=CARTESIAN_POINT('Ctrl Pts',(-3.32692550442964,7.18113790300319,98.2742062002916));
#58106=CARTESIAN_POINT('Ctrl Pts',(-2.97282975724784,7.33280688163681,98.2606186684839));
#58107=CARTESIAN_POINT('Ctrl Pts',(-2.82911022444385,7.38944585188904,98.2552500457254));
#58108=CARTESIAN_POINT('Ctrl Pts',(-2.42160049744456,7.53641001501459,98.2402816425567));
#58109=CARTESIAN_POINT('Ctrl Pts',(-2.15456613759086,7.61705101941511,98.2307696106032));
#58110=CARTESIAN_POINT('Ctrl Pts',(-1.66061579052986,7.73815863733083,98.2129938161668));
#58111=CARTESIAN_POINT('Ctrl Pts',(-1.4351249485373,7.7831324781503,98.2048100142019));
#58112=CARTESIAN_POINT('Ctrl Pts',(-1.09707295936599,7.83536547998387,98.1920607380509));
#58113=CARTESIAN_POINT('Ctrl Pts',(-0.985789996760458,7.85014251977632,
98.1877869993949));
#58114=CARTESIAN_POINT('Ctrl Pts',(-0.819622733686073,7.86861861349604,
98.1812450557757));
#58115=CARTESIAN_POINT('Ctrl Pts',(-0.764952136581349,7.87412141438865,
98.1790661095606));
#58116=CARTESIAN_POINT('Ctrl Pts',(-0.700465852246928,7.87993430857362,
98.1764671723144));
#58117=CARTESIAN_POINT('Ctrl Pts',(-0.690699889029933,7.88079632902611,
98.1760728124853));
#58118=CARTESIAN_POINT('Ctrl Pts',(-0.675724804958643,7.88209009776201,
98.1754669462412));
#58119=CARTESIAN_POINT('Ctrl Pts',(-0.670516792644889,7.88253484304782,
98.1752560245704));
#58120=CARTESIAN_POINT('Ctrl Pts',(-0.661430342221076,7.88330172253212,
98.1748876583817));
#58121=CARTESIAN_POINT('Ctrl Pts',(-0.657552095951879,7.88362615723995,
98.1747303161144));
#58122=CARTESIAN_POINT('Ctrl Pts',(-0.649440117962912,7.88429873729437,
98.1744009656177));
#58123=CARTESIAN_POINT('Ctrl Pts',(-0.645206342919183,7.88464633453357,
98.1742289333189));
#58124=CARTESIAN_POINT('Ctrl Pts',(-0.633492193008744,7.8855985798844,98.1737525680257));
#58125=CARTESIAN_POINT('Ctrl Pts',(-0.626011247001237,7.88619599298329,
98.1734479200408));
#58126=CARTESIAN_POINT('Ctrl Pts',(-0.596619157148946,7.88850109946786,
98.1722493214382));
#58127=CARTESIAN_POINT('Ctrl Pts',(-0.574701921391014,7.89012811701314,
98.1713519236345));
#58128=CARTESIAN_POINT('Ctrl Pts',(-0.190394621470284,7.91704725096131,
98.1555561179059));
#58129=CARTESIAN_POINT('Ctrl Pts',(0.173287754408456,7.91743819494948,98.1396859477806));
#58130=CARTESIAN_POINT('Ctrl Pts',(0.876783607160662,7.86969231320218,98.1085077294422));
#58131=CARTESIAN_POINT('Ctrl Pts',(1.216032846893,7.8244538951565,98.0932554166211));
#58132=CARTESIAN_POINT('Ctrl Pts',(1.99705461786198,7.66826866151834,98.0583952027387));
#58133=CARTESIAN_POINT('Ctrl Pts',(2.43433014304468,7.54086654960135,98.0391066239844));
#58134=CARTESIAN_POINT('Ctrl Pts',(2.89204107640193,7.36351349495035,98.0192029221403));
#58135=CARTESIAN_POINT('Ctrl Pts',(2.9257202941035,7.35019682516418,98.0177396516237));
#58136=CARTESIAN_POINT('Ctrl Pts',(2.97236040762036,7.33138409298264,98.0157147440098));
#58137=CARTESIAN_POINT('Ctrl Pts',(2.98539969212397,7.32608406938041,98.0151487968078));
#58138=CARTESIAN_POINT('Ctrl Pts',(3.00745910818325,7.31704899692897,98.014191595302));
#58139=CARTESIAN_POINT('Ctrl Pts',(3.0164865813896,7.31333200502505,98.0137999461504));
#58140=CARTESIAN_POINT('Ctrl Pts',(3.03424534237298,7.30598149733122,98.0130296270588));
#58141=CARTESIAN_POINT('Ctrl Pts',(3.04297704129478,7.30234901684003,98.0126509351407));
#58142=CARTESIAN_POINT('Ctrl Pts',(3.06375326808353,7.29366214798591,98.0117500192264));
#58143=CARTESIAN_POINT('Ctrl Pts',(3.07579184434141,7.28859356448904,98.0112281084987));
#58144=CARTESIAN_POINT('Ctrl Pts',(3.11512726115402,7.27191742224343,98.0095231621728));
#58145=CARTESIAN_POINT('Ctrl Pts',(3.14237147573479,7.2601861115074,98.0083428788613));
#58146=CARTESIAN_POINT('Ctrl Pts',(3.49152641311007,7.10750707289723,97.9932235847153));
#58147=CARTESIAN_POINT('Ctrl Pts',(3.80377448883215,6.94541114067332,97.9798034219212));
#58148=CARTESIAN_POINT('Ctrl Pts',(4.53682438160458,6.50055438265888,97.9479551901981));
#58149=CARTESIAN_POINT('Ctrl Pts',(4.94322454817824,6.19713655633724,97.9300385815423));
#58150=CARTESIAN_POINT('Ctrl Pts',(5.45146371245044,5.73568052074982,97.9048716968738));
#58151=CARTESIAN_POINT('Ctrl Pts',(5.5808772896782,5.60983891370074,97.8981722591362));
#58152=CARTESIAN_POINT('Ctrl Pts',(5.79597196089109,5.38586581871726,97.8863311581107));
#58153=CARTESIAN_POINT('Ctrl Pts',(5.8837428038153,5.28984025364703,97.881278223978));
#58154=CARTESIAN_POINT('Ctrl Pts',(5.98388133289996,5.17470697560628,97.8751949407279));
#58155=CARTESIAN_POINT('Ctrl Pts',(5.99858677314492,5.15765303214884,97.8742932363095));
#58156=CARTESIAN_POINT('Ctrl Pts',(6.01796247917411,5.13498801229907,97.8730937129871));
#58157=CARTESIAN_POINT('Ctrl Pts',(6.02269817219764,5.12943281594483,97.8727996196094));
#58158=CARTESIAN_POINT('Ctrl Pts',(6.03045320258931,5.12031024587037,97.8723165075815));
#58159=CARTESIAN_POINT('Ctrl Pts',(6.03347708637872,5.11674672918151,97.8721277510668));
#58160=CARTESIAN_POINT('Ctrl Pts',(6.03932441141383,5.10984351806587,97.8717620118368));
#58161=CARTESIAN_POINT('Ctrl Pts',(6.04214824523947,5.10650415723458,97.8715850520534));
#58162=CARTESIAN_POINT('Ctrl Pts',(6.04865190629147,5.0988002223273,97.8711767149903));
#58163=CARTESIAN_POINT('Ctrl Pts',(6.05232977797308,5.09443400674606,97.8709452234577));
#58164=CARTESIAN_POINT('Ctrl Pts',(6.06404827904625,5.08049169106819,97.8702057959547));
#58165=CARTESIAN_POINT('Ctrl Pts',(6.07207090267749,5.07090054168168,97.8696967971465));
#58166=CARTESIAN_POINT('Ctrl Pts',(6.15048601704781,4.97670135573191,97.8646940085584));
#58167=CARTESIAN_POINT('Ctrl Pts',(6.21911944045624,4.89066300621524,97.8600879812803));
#58168=CARTESIAN_POINT('Ctrl Pts',(6.78918291423936,4.14462587330208,97.819916693381));
#58169=CARTESIAN_POINT('Ctrl Pts',(7.18582867158503,3.41101931780166,97.7797379126986));
#58170=CARTESIAN_POINT('Ctrl Pts',(7.56019750592523,2.34857712119468,97.7301028480254));
#58171=CARTESIAN_POINT('Ctrl Pts',(7.64315750718252,2.0626607488169,97.7174316340397));
#58172=CARTESIAN_POINT('Ctrl Pts',(7.71617822900833,1.74508427469245,97.704139359267));
#58173=CARTESIAN_POINT('Ctrl Pts',(7.72238574655146,1.71740618125558,97.7029871603612));
#58174=CARTESIAN_POINT('Ctrl Pts',(7.73144848490893,1.67595440187964,97.7012708971637));
#58175=CARTESIAN_POINT('Ctrl Pts',(7.7344160194328,1.66220566508413,97.700703175499));
#58176=CARTESIAN_POINT('Ctrl Pts',(7.73976473955366,1.63710030728881,97.6996692857803));
#58177=CARTESIAN_POINT('Ctrl Pts',(7.74215763290902,1.62574623741598,97.6992027370078));
#58178=CARTESIAN_POINT('Ctrl Pts',(7.74589706205311,1.60780747421338,97.6984672445526));
#58179=CARTESIAN_POINT('Ctrl Pts',(7.7472601974562,1.6012262810927,97.698197759984));
#58180=CARTESIAN_POINT('Ctrl Pts',(7.7496862370617,1.5894377850813,97.6977156655051));
#58181=CARTESIAN_POINT('Ctrl Pts',(7.75075228285058,1.58423113704496,97.6975029533019));
#58182=CARTESIAN_POINT('Ctrl Pts',(7.75319642646384,1.57223223677979,97.6970132458772));
#58183=CARTESIAN_POINT('Ctrl Pts',(7.75457084785914,1.56543923534461,97.696736370617));
#58184=CARTESIAN_POINT('Ctrl Pts',(7.75830561854607,1.54685472483215,97.6959798828393));
#58185=CARTESIAN_POINT('Ctrl Pts',(7.7606480157795,1.5350596038438,97.695500855593));
#58186=CARTESIAN_POINT('Ctrl Pts',(7.77186746763788,1.47788207416338,97.6931840265366));
#58187=CARTESIAN_POINT('Ctrl Pts',(7.78037347612177,1.43242731956261,97.6913583264785));
#58188=CARTESIAN_POINT('Ctrl Pts',(7.89690744740592,0.778001972829458,97.6652990699414));
#58189=CARTESIAN_POINT('Ctrl Pts',(7.93356207358035,0.15849534543688,97.6436748423889));
#58190=CARTESIAN_POINT('Ctrl Pts',(7.87599193376859,-0.832039215783152,
97.6099191098755));
#58191=CARTESIAN_POINT('Ctrl Pts',(7.82791166507928,-1.2030455904179,97.597400382183));
#58192=CARTESIAN_POINT('Ctrl Pts',(7.72315450416746,-1.72065955025918,97.57871467027));
#58193=CARTESIAN_POINT('Ctrl Pts',(7.68808432706997,-1.87113351773135,97.5731299358965));
#58194=CARTESIAN_POINT('Ctrl Pts',(7.61511522158514,-2.14736213019957,97.5624452902443));
#58195=CARTESIAN_POINT('Ctrl Pts',(7.57844674478341,-2.2733863844321,97.5574003481183));
#58196=CARTESIAN_POINT('Ctrl Pts',(7.53240725752627,-2.41809586659111,97.5513503408022));
#58197=CARTESIAN_POINT('Ctrl Pts',(7.52607501833165,-2.43773286406106,97.5505238223494));
#58198=CARTESIAN_POINT('Ctrl Pts',(7.51783596263814,-2.46294501600872,97.5494552666602));
#58199=CARTESIAN_POINT('Ctrl Pts',(7.51599958616362,-2.46854328166255,97.5492175290945));
#58200=CARTESIAN_POINT('Ctrl Pts',(7.51303246372053,-2.47755466682522,97.5488340865821));
#58201=CARTESIAN_POINT('Ctrl Pts',(7.51190563859322,-2.48096908584139,97.548688623508));
#58202=CARTESIAN_POINT('Ctrl Pts',(7.50974777017838,-2.48749274545329,97.5484103599258));
#58203=CARTESIAN_POINT('Ctrl Pts',(7.50871712600336,-2.49060210631536,97.5482775846585));
#58204=CARTESIAN_POINT('Ctrl Pts',(7.50634746221691,-2.49773632895663,97.5479726048631));
#58205=CARTESIAN_POINT('Ctrl Pts',(7.50500713715356,-2.50176075268644,97.5478003200286));
#58206=CARTESIAN_POINT('Ctrl Pts',(7.50149332571056,-2.51228299163291,97.5473492270486));
#58207=CARTESIAN_POINT('Ctrl Pts',(7.4993146377957,-2.51877905114278,97.5470701015766));
#58208=CARTESIAN_POINT('Ctrl Pts',(7.4854862962818,-2.5598331749768,97.5453020843156));
#58209=CARTESIAN_POINT('Ctrl Pts',(7.47360640837212,-2.59431265371224,97.5437993399137));
#58210=CARTESIAN_POINT('Ctrl Pts',(7.27326670990972,-3.16296930268619,97.5187349091876));
#58211=CARTESIAN_POINT('Ctrl Pts',(7.02822016210335,-3.67543575339453,97.4921630072294));
#58212=CARTESIAN_POINT('Ctrl Pts',(6.53399001681676,-4.47558325333099,97.4486546516073));
#58213=CARTESIAN_POINT('Ctrl Pts',(6.31505682868153,-4.77953603394728,97.431538199999));
#58214=CARTESIAN_POINT('Ctrl Pts',(5.88640863203758,-5.29350579782384,97.4022131556574));
#58215=CARTESIAN_POINT('Ctrl Pts',(5.68485226007152,-5.50940018598597,97.389747079382));
#58216=CARTESIAN_POINT('Ctrl Pts',(5.4614183339711,-5.72337600292911,97.3772429288809));
#58217=CARTESIAN_POINT('Ctrl Pts',(5.45112475483649,-5.73318079250761,97.3766695838246));
#58218=CARTESIAN_POINT('Ctrl Pts',(5.43461007812739,-5.74882658595001,97.3757540563638));
#58219=CARTESIAN_POINT('Ctrl Pts',(5.42840588515143,-5.75468534007516,97.375411085317));
#58220=CARTESIAN_POINT('Ctrl Pts',(5.41656534588007,-5.76583043169145,97.3747583798875));
#58221=CARTESIAN_POINT('Ctrl Pts',(5.41093071220174,-5.77111856934268,97.3744485658628));
#58222=CARTESIAN_POINT('Ctrl Pts',(5.40102613526343,-5.78038681746712,97.3739053614396));
#58223=CARTESIAN_POINT('Ctrl Pts',(5.39675952294974,-5.78437046920302,97.3736718147524));
#58224=CARTESIAN_POINT('Ctrl Pts',(5.38841240834321,-5.79214673086284,97.3732157868127));
#58225=CARTESIAN_POINT('Ctrl Pts',(5.38433230223921,-5.79593975930175,97.3729932871693));
#58226=CARTESIAN_POINT('Ctrl Pts',(5.37462719476904,-5.80494291989034,97.3724650094431));
#58227=CARTESIAN_POINT('Ctrl Pts',(5.36899861373186,-5.81014919534193,97.3721594008083));
#58228=CARTESIAN_POINT('Ctrl Pts',(5.3490837804728,-5.82851619284444,97.3710808250136));
#58229=CARTESIAN_POINT('Ctrl Pts',(5.33475658011445,-5.84163252342766,97.3703098012611));
#58230=CARTESIAN_POINT('Ctrl Pts',(5.15104940200479,-6.00857410413087,97.3604859332803));
#58231=CARTESIAN_POINT('Ctrl Pts',(4.97511535242341,-6.1550394160176,97.3517578594723));
#58232=CARTESIAN_POINT('Ctrl Pts',(4.20555875145421,-6.74110958580798,97.3160106768834));
#58233=CARTESIAN_POINT('Ctrl Pts',(3.55837042889229,-7.10402463619165,97.292126285281));
#58234=CARTESIAN_POINT('Ctrl Pts',(2.58965136890302,-7.4811975796568,97.2552687244209));
#58235=CARTESIAN_POINT('Ctrl Pts',(2.30303676950454,-7.57433831039145,97.2441778146889));
#58236=CARTESIAN_POINT('Ctrl Pts',(2.00159784898675,-7.65360302245741,97.2316829495804));
#58237=CARTESIAN_POINT('Ctrl Pts',(1.99134946309288,-7.65627588898199,97.2312571652177));
#58238=CARTESIAN_POINT('Ctrl Pts',(1.97663439589886,-7.66008216017931,97.2306443587212));
#58239=CARTESIAN_POINT('Ctrl Pts',(1.97217201576983,-7.66123226221728,97.2304583324528));
#58240=CARTESIAN_POINT('Ctrl Pts',(1.96439891896064,-7.66322840347944,97.2301339601485));
#58241=CARTESIAN_POINT('Ctrl Pts',(1.96108864468724,-7.66407620032041,97.2299957178634));
#58242=CARTESIAN_POINT('Ctrl Pts',(1.95470340669017,-7.66570712071519,97.2297288609134));
#58243=CARTESIAN_POINT('Ctrl Pts',(1.95162851841142,-7.66649053966545,97.2296002636309));
#58244=CARTESIAN_POINT('Ctrl Pts',(1.94435507284219,-7.66833900613128,97.2292958659644));
#58245=CARTESIAN_POINT('Ctrl Pts',(1.94015611433258,-7.66940245482756,97.2291199724013));
#58246=CARTESIAN_POINT('Ctrl Pts',(1.92549819789716,-7.67310198216848,97.2285053852268));
#58247=CARTESIAN_POINT('Ctrl Pts',(1.91503476413194,-7.67572010881576,97.2280656549363));
#58248=CARTESIAN_POINT('Ctrl Pts',(1.79171308720687,-7.70630940144599,97.2228713699366));
#58249=CARTESIAN_POINT('Ctrl Pts',(1.67826155591636,-7.73180936952574,97.2179781574631));
#58250=CARTESIAN_POINT('Ctrl Pts',(1.54700860990204,-7.75828565632762,97.2122193604017));
#58251=CARTESIAN_POINT('Ctrl Pts',(1.52971110488684,-7.76171475207178,97.2114584752931));
#58252=CARTESIAN_POINT('Ctrl Pts',(1.47402506449754,-7.77256069769861,97.2090030067418));
#58253=CARTESIAN_POINT('Ctrl Pts',(1.43559331801603,-7.7797507313171,97.2072992900871));
#58254=CARTESIAN_POINT('Ctrl Pts',(0.784062469934928,-7.89665078917537,
97.1782808343046));
#58255=CARTESIAN_POINT('Ctrl Pts',(0.160173348218243,-7.9338659838256,97.1486653187389));
#58256=CARTESIAN_POINT('Ctrl Pts',(-0.944464206621942,-7.86929673197473,
97.0985651305772));
#58257=CARTESIAN_POINT('Ctrl Pts',(-1.42373331740787,-7.79685410944183,
97.0775873709844));
#58258=CARTESIAN_POINT('Ctrl Pts',(-1.91165181435241,-7.6765786788436,97.0572816980415));
#58259=CARTESIAN_POINT('Ctrl Pts',(-1.92984890895361,-7.67202424830974,
97.0565257971353));
#58260=CARTESIAN_POINT('Ctrl Pts',(-1.95613539972124,-7.66534573526553,
97.0554358706597));
#58261=CARTESIAN_POINT('Ctrl Pts',(-1.96423783056654,-7.66327349692795,
97.0551001924466));
#58262=CARTESIAN_POINT('Ctrl Pts',(-1.9783514766435,-7.65964000502872,97.054515951078));
#58263=CARTESIAN_POINT('Ctrl Pts',(-1.98436416020023,-7.65808451583731,
97.0542672042068));
#58264=CARTESIAN_POINT('Ctrl Pts',(-1.99596215424604,-7.65506952316407,
97.0537876810943));
#58265=CARTESIAN_POINT('Ctrl Pts',(-2.00154770952764,-7.65361098386329,
97.0535568742796));
#58266=CARTESIAN_POINT('Ctrl Pts',(-2.01476324621697,-7.65014459403056,
97.0530110865562));
#58267=CARTESIAN_POINT('Ctrl Pts',(-2.02239183716026,-7.64813143881188,
97.0526962752672));
#58268=CARTESIAN_POINT('Ctrl Pts',(-2.04905904217515,-7.64105137943291,
97.051596630049));
#58269=CARTESIAN_POINT('Ctrl Pts',(-2.06808180045149,-7.63592475180237,
97.0508137053821));
#58270=CARTESIAN_POINT('Ctrl Pts',(-2.29707558458299,-7.57329250795526,
97.0414065991472));
#58271=CARTESIAN_POINT('Ctrl Pts',(-2.50461298827936,-7.50721239689595,
97.0330638404919));
#58272=CARTESIAN_POINT('Ctrl Pts',(-3.37448376529839,-7.1901480976028,96.9985912197845));
#58273=CARTESIAN_POINT('Ctrl Pts',(-4.00416266530335,-6.8594443966711,96.9752132996989));
#58274=CARTESIAN_POINT('Ctrl Pts',(-4.73127418515022,-6.34292949258007,
96.9434764196706));
#58275=CARTESIAN_POINT('Ctrl Pts',(-4.87736879414416,-6.23129025629814,
96.9368009531319));
#58276=CARTESIAN_POINT('Ctrl Pts',(-5.11391640284901,-6.03711202913383,
96.9252596042317));
#58277=CARTESIAN_POINT('Ctrl Pts',(-5.20658246249291,-5.95737855214634,
96.9205379163792));
#58278=CARTESIAN_POINT('Ctrl Pts',(-5.3123013031363,-5.86206282547851,96.9148653713794));
#58279=CARTESIAN_POINT('Ctrl Pts',(-5.32719093719876,-5.84853506534418,
96.9140596525386));
#58280=CARTESIAN_POINT('Ctrl Pts',(-5.34650396682319,-5.83085355227314,
96.9130054667608));
#58281=CARTESIAN_POINT('Ctrl Pts',(-5.35097451863605,-5.82675119735221,
96.9127608068036));
#58282=CARTESIAN_POINT('Ctrl Pts',(-5.35821996701821,-5.82008711683847,
96.9123632396936));
#58283=CARTESIAN_POINT('Ctrl Pts',(-5.36099776344828,-5.81752853390104,
96.9122105685375));
#58284=CARTESIAN_POINT('Ctrl Pts',(-5.36632732351144,-5.81261250437512,
96.9119171668694));
#58285=CARTESIAN_POINT('Ctrl Pts',(-5.36887936196677,-5.81025537008366,
96.9117764596559));
#58286=CARTESIAN_POINT('Ctrl Pts',(-5.37473316796677,-5.80484148092104,
96.9114532208598));
#58287=CARTESIAN_POINT('Ctrl Pts',(-5.37803388001659,-5.80178359047776,
96.9112706035782));
#58288=CARTESIAN_POINT('Ctrl Pts',(-5.38680420246663,-5.79364455408345,
96.9107844265311));
#58289=CARTESIAN_POINT('Ctrl Pts',(-5.39226921995256,-5.7885584901245,96.9104804981609));
#58290=CARTESIAN_POINT('Ctrl Pts',(-5.42864588562386,-5.75460802607219,
96.9084509876503));
#58291=CARTESIAN_POINT('Ctrl Pts',(-5.45933233624993,-5.7255043451088,96.9067077044633));
#58292=CARTESIAN_POINT('Ctrl Pts',(-6.04085123980206,-5.16505400895148,
96.8730979799399));
#58293=CARTESIAN_POINT('Ctrl Pts',(-6.51193319830862,-4.55680401131707,
96.8363714951854));
#58294=CARTESIAN_POINT('Ctrl Pts',(-6.98551451496333,-3.71827483474916,
96.7931407226837));
#58295=CARTESIAN_POINT('Ctrl Pts',(-7.07622549551358,-3.54260069036832,
96.7844122518932));
#58296=CARTESIAN_POINT('Ctrl Pts',(-7.25427466057304,-3.16359040556691,
96.7663415805362));
#58297=CARTESIAN_POINT('Ctrl Pts',(-7.33985743820359,-2.9596128293226,96.7570583219185));
#58298=CARTESIAN_POINT('Ctrl Pts',(-7.42962216189515,-2.71771899361371,
96.7465605196102));
#58299=CARTESIAN_POINT('Ctrl Pts',(-7.4422151182252,-2.68304233632671,96.7450674896062));
#58300=CARTESIAN_POINT('Ctrl Pts',(-7.45821650276812,-2.63800048686436,
96.7431433785664));
#58301=CARTESIAN_POINT('Ctrl Pts',(-7.46184659423552,-2.62771485823343,
96.7427050166952));
#58302=CARTESIAN_POINT('Ctrl Pts',(-7.46768573813538,-2.61106035126055,
96.7419968678546));
#58303=CARTESIAN_POINT('Ctrl Pts',(-7.46990793680914,-2.60469611612557,
96.7417266494842));
#58304=CARTESIAN_POINT('Ctrl Pts',(-7.47414020983483,-2.59252519399573,
96.7412106263256));
#58305=CARTESIAN_POINT('Ctrl Pts',(-7.47615165808868,-2.58671899193715,
96.7409647766034));
#58306=CARTESIAN_POINT('Ctrl Pts',(-7.48074276589454,-2.57341631340396,
96.7404022415784));
#58307=CARTESIAN_POINT('Ctrl Pts',(-7.48331792751358,-2.56591828548731,
96.7400857038874));
#58308=CARTESIAN_POINT('Ctrl Pts',(-7.4912067603749,-2.54283569782629,96.7391128836655));
#58309=CARTESIAN_POINT('Ctrl Pts',(-7.49648306633123,-2.52723836493505,
96.7384578251028));
#58310=CARTESIAN_POINT('Ctrl Pts',(-7.53554001963557,-2.4105832081675,96.7335755300657));
#58311=CARTESIAN_POINT('Ctrl Pts',(-7.56732525490818,-2.30886646748193,
96.7294138602341));
#58312=CARTESIAN_POINT('Ctrl Pts',(-7.60067265469127,-2.19405223036691,
96.7248160019466));
#58313=CARTESIAN_POINT('Ctrl Pts',(-7.60426777669348,-2.18155943663766,
96.7243170257901));
#58314=CARTESIAN_POINT('Ctrl Pts',(-7.61592926683549,-2.14065750266921,
96.7226875988423));
#58315=CARTESIAN_POINT('Ctrl Pts',(-7.62386739121038,-2.1122119126991,96.7215610879662));
#58316=CARTESIAN_POINT('Ctrl Pts',(-7.63698072819023,-2.06418423447807,
96.7196700504169));
#58317=CARTESIAN_POINT('Ctrl Pts',(-7.64224033152176,-2.04462561818233,
96.7189030064159));
#58318=CARTESIAN_POINT('Ctrl Pts',(-7.66548484278247,-1.95684461499868,
96.7154738553882));
#58319=CARTESIAN_POINT('Ctrl Pts',(-7.68263194283628,-1.8884028770051,96.7128365084654));
#58320=CARTESIAN_POINT('Ctrl Pts',(-7.83974466683613,-1.2236985072228,96.6875456135794));
#58321=CARTESIAN_POINT('Ctrl Pts',(-7.9109317711384,-0.613344488602599,
96.6670372056062));
#58322=CARTESIAN_POINT('Ctrl Pts',(-7.91101242576093,0.111181534452813,
96.6419010833049));
#58323=CARTESIAN_POINT('Ctrl Pts',(-7.90864379419039,0.223229965881314,
96.6379849084005));
#58324=CARTESIAN_POINT('Ctrl Pts',(-7.89454116945423,0.55577610161645,96.6261922541451));
#58325=CARTESIAN_POINT('Ctrl Pts',(-7.87595655219195,0.775864345783876,
96.6181662688479));
#58326=CARTESIAN_POINT('Ctrl Pts',(-7.84721533378392,1.00259316009575,96.6094266656964));
#58327=CARTESIAN_POINT('Ctrl Pts',(-7.84622545995603,1.01031063063012,96.6091286140298));
#58328=CARTESIAN_POINT('Ctrl Pts',(-7.84440492471485,1.02434023164507,96.6085857293842));
#58329=CARTESIAN_POINT('Ctrl Pts',(-7.84357802507125,1.03065285005739,96.6083410695011));
#58330=CARTESIAN_POINT('Ctrl Pts',(-7.83164117232685,1.12093335521034,96.6048363958647));
#58331=CARTESIAN_POINT('Ctrl Pts',(-7.81919137533511,1.20471588297486,96.6015140913077));
#58332=CARTESIAN_POINT('Ctrl Pts',(-7.80375591026096,1.29823592672715,96.5977119409698));
#58333=CARTESIAN_POINT('Ctrl Pts',(-7.80209358286066,1.30818903485749,96.5973060955238));
#58334=CARTESIAN_POINT('Ctrl Pts',(-7.79966086636241,1.32258523514935,96.5967173209093));
#58335=CARTESIAN_POINT('Ctrl Pts',(-7.79890570888939,1.32703092586222,96.5965352585944));
#58336=CARTESIAN_POINT('Ctrl Pts',(-7.79757215536432,1.33484124043352,96.5962149760306));
#58337=CARTESIAN_POINT('Ctrl Pts',(-7.79699538104706,1.33820614373744,96.5960768488786));
#58338=CARTESIAN_POINT('Ctrl Pts',(-7.79580427132759,1.34512816999395,96.5957924133221));
#58339=CARTESIAN_POINT('Ctrl Pts',(-7.79518967916424,1.34868524731664,96.5956460901138));
#58340=CARTESIAN_POINT('Ctrl Pts',(-7.79361989610751,1.35773376749065,96.5952734672555));
#58341=CARTESIAN_POINT('Ctrl Pts',(-7.79266134349221,1.36322457934425,96.5950469724143));
#58342=CARTESIAN_POINT('Ctrl Pts',(-7.78870571988583,1.38574280563983,96.5941165388882));
#58343=CARTESIAN_POINT('Ctrl Pts',(-7.78565866342316,1.40276123485916,96.5934096979755));
#58344=CARTESIAN_POINT('Ctrl Pts',(-7.76489014763892,1.51660516842505,96.5886575269258));
#58345=CARTESIAN_POINT('Ctrl Pts',(-7.74541928441796,1.61309914602549,96.5845143465535));
#58346=CARTESIAN_POINT('Ctrl Pts',(-7.67484520212179,1.93203479706354,96.5704972841864));
#58347=CARTESIAN_POINT('Ctrl Pts',(-7.61591933615756,2.15261891438979,96.5602798822387));
#58348=CARTESIAN_POINT('Ctrl Pts',(-7.40049836046155,2.83855604864864,96.5275013703022));
#58349=CARTESIAN_POINT('Ctrl Pts',(-7.21018808598541,3.29211219139292,96.5044061538131));
#58350=CARTESIAN_POINT('Ctrl Pts',(-6.77675913635513,4.10415242373941,96.4628974326378));
#58351=CARTESIAN_POINT('Ctrl Pts',(-6.54388146844187,4.46611958430109,96.4443169523507));
#58352=CARTESIAN_POINT('Ctrl Pts',(-6.26576455361047,4.82958534178484,96.4257630011086));
#58353=CARTESIAN_POINT('Ctrl Pts',(-6.24868617022989,4.85166169291655,96.4246362373281));
#58354=CARTESIAN_POINT('Ctrl Pts',(-6.22537607679404,4.88146619689521,96.4231151904258));
#58355=CARTESIAN_POINT('Ctrl Pts',(-6.21924623645517,4.88927354320106,96.4227167639095));
#58356=CARTESIAN_POINT('Ctrl Pts',(-6.20956101399402,4.90156156035102,96.4220896968384));
#58357=CARTESIAN_POINT('Ctrl Pts',(-6.20601544916333,4.90604993465733,96.4218606554426));
#58358=CARTESIAN_POINT('Ctrl Pts',(-6.19917274986115,4.91469290485161,96.4214196115396));
#58359=CARTESIAN_POINT('Ctrl Pts',(-6.19587629957406,4.91884803710618,96.4212075812104));
#58360=CARTESIAN_POINT('Ctrl Pts',(-6.18808238639251,4.92865189624494,96.4207073099323));
#58361=CARTESIAN_POINT('Ctrl Pts',(-6.18358136022797,4.93429779167698,96.4204192153971));
#58362=CARTESIAN_POINT('Ctrl Pts',(-6.17041615704708,4.95076535747961,96.4195789290689));
#58363=CARTESIAN_POINT('Ctrl Pts',(-6.16173123658752,4.96157045164196,96.4190275908163));
#58364=CARTESIAN_POINT('Ctrl Pts',(-6.09891567633802,5.03930131507524,96.4150613168749));
#58365=CARTESIAN_POINT('Ctrl Pts',(-6.04372336392814,5.10536371573891,96.4116905487208));
#58366=CARTESIAN_POINT('Ctrl Pts',(-5.86529457670188,5.31198452574972,96.4011384051676));
#58367=CARTESIAN_POINT('Ctrl Pts',(-5.73814716425488,5.44908547273671,96.3941239854296));
#58368=CARTESIAN_POINT('Ctrl Pts',(-5.37924052860825,5.80958021610153,96.3755058460303));
#58369=CARTESIAN_POINT('Ctrl Pts',(-5.13851793240377,6.02354531109611,96.3642701795929));
#58370=CARTESIAN_POINT('Ctrl Pts',(-4.78131289246753,6.30400584539876,96.3486541259081));
#58371=CARTESIAN_POINT('Ctrl Pts',(-4.67516442566243,6.38312466080315,96.3441315841764));
#58372=CARTESIAN_POINT('Ctrl Pts',(-4.44885679575818,6.54313059641601,96.3346484133025));
#58373=CARTESIAN_POINT('Ctrl Pts',(-4.32836137464931,6.6234561897225,96.3296883597387));
#58374=CARTESIAN_POINT('Ctrl Pts',(-3.8788135012559,6.90562876539424,96.3112882736169));
#58375=CARTESIAN_POINT('Ctrl Pts',(-3.53734659762423,7.08660869166393,96.2975251323113));
#58376=CARTESIAN_POINT('Ctrl Pts',(-3.16033565001871,7.25237011756868,96.2811759425317));
#58377=CARTESIAN_POINT('Ctrl Pts',(-3.13654106038979,7.26269260603235,96.2801393037005));
#58378=CARTESIAN_POINT('Ctrl Pts',(-3.10657306277045,7.27551848111512,96.2788272024673));
#58379=CARTESIAN_POINT('Ctrl Pts',(-3.1004464331563,7.27813144137852,96.2785586167917));
#58380=CARTESIAN_POINT('Ctrl Pts',(-3.09079979236863,7.28223126828615,96.2781351699607));
#58381=CARTESIAN_POINT('Ctrl Pts',(-3.0872819792554,7.28372333231947,96.2779806384275));
#58382=CARTESIAN_POINT('Ctrl Pts',(-3.08107304680822,7.28635151589261,96.2777076865322));
#58383=CARTESIAN_POINT('Ctrl Pts',(-3.07838237409141,7.28748869582368,96.2775893338576));
#58384=CARTESIAN_POINT('Ctrl Pts',(-3.07220750777794,7.29009439756027,96.2773175681336));
#58385=CARTESIAN_POINT('Ctrl Pts',(-3.06872289730959,7.29156190918982,96.2771640905632));
#58386=CARTESIAN_POINT('Ctrl Pts',(-3.05903343260587,7.29563436201795,96.2767370090156));
#58387=CARTESIAN_POINT('Ctrl Pts',(-3.05282631402452,7.298233881009,96.2764630597826));
#58388=CARTESIAN_POINT('Ctrl Pts',(-3.01843808015325,7.31258400356743,96.2749433927296));
#58389=CARTESIAN_POINT('Ctrl Pts',(-2.99019279262271,7.32417915305233,96.2736879343907));
#58390=CARTESIAN_POINT('Ctrl Pts',(-2.90937067494452,7.35681250209504,96.2700763863128));
#58391=CARTESIAN_POINT('Ctrl Pts',(-2.85663492969077,7.3774497285887,96.2676968832453));
#58392=CARTESIAN_POINT('Ctrl Pts',(-2.56208704443017,7.48908432858149,96.254297989862));
#58393=CARTESIAN_POINT('Ctrl Pts',(-2.31616577948795,7.56875362615606,96.2427102251037));
#58394=CARTESIAN_POINT('Ctrl Pts',(-1.69949489723706,7.73566031037718,96.2134164926229));
#58395=CARTESIAN_POINT('Ctrl Pts',(-1.32548972226909,7.80844428460587,96.1954656300268));
#58396=CARTESIAN_POINT('Ctrl Pts',(-0.373670040999901,7.92329465183099,
96.1510911589718));
#58397=CARTESIAN_POINT('Ctrl Pts',(0.206291507140203,7.9294300211983,96.1253621958436));
#58398=CARTESIAN_POINT('Ctrl Pts',(0.821585396059392,7.8683235584578,96.1001591034313));
#58399=CARTESIAN_POINT('Ctrl Pts',(0.861324412788489,7.86407264096575,96.0985398492904));
#58400=CARTESIAN_POINT('Ctrl Pts',(0.912335613862318,7.85822462306197,96.0964719624382));
#58401=CARTESIAN_POINT('Ctrl Pts',(0.92363853841978,7.85690411998279,96.0960144396939));
#58402=CARTESIAN_POINT('Ctrl Pts',(0.941671159765812,7.85475794637879,96.0952855780316));
#58403=CARTESIAN_POINT('Ctrl Pts',(0.948402691753518,7.85394800746179,96.0950137333293));
#58404=CARTESIAN_POINT('Ctrl Pts',(0.961003937724138,7.85241538682511,96.094505289953));
#58405=CARTESIAN_POINT('Ctrl Pts',(0.966873895970737,7.85169477533735,96.0942686248819));
#58406=CARTESIAN_POINT('Ctrl Pts',(0.979968085285564,7.85007239166202,96.0937410927008));
#58407=CARTESIAN_POINT('Ctrl Pts',(0.987191894947225,7.8491672275112,96.0934503348867));
#58408=CARTESIAN_POINT('Ctrl Pts',(1.00828188472015,7.84649501585229,96.092602252508));
#58409=CARTESIAN_POINT('Ctrl Pts',(1.02214467650056,7.84470118333229,96.092045789505));
#58410=CARTESIAN_POINT('Ctrl Pts',(1.12206971331923,7.83150160222718,96.0880418176562));
#58411=CARTESIAN_POINT('Ctrl Pts',(1.20794535777824,7.81871641685071,96.0846388643084));
#58412=CARTESIAN_POINT('Ctrl Pts',(1.47995026465021,7.77363175057574,96.0739703756444));
#58413=CARTESIAN_POINT('Ctrl Pts',(1.66514509046851,7.73607785304665,96.0668729920068));
#58414=CARTESIAN_POINT('Ctrl Pts',(2.19791205870354,7.6080224184368,96.0467817592011));
#58415=CARTESIAN_POINT('Ctrl Pts',(2.5408915497368,7.50044721911272,96.0342751639329));
#58416=CARTESIAN_POINT('Ctrl Pts',(3.22335765049642,7.2341828902578,96.0090172477693));
#58417=CARTESIAN_POINT('Ctrl Pts',(3.56126482398948,7.07395290000678,95.9963035989677));
#58418=CARTESIAN_POINT('Ctrl Pts',(4.10987154105077,6.76451047309412,95.973629768836));
#58419=CARTESIAN_POINT('Ctrl Pts',(4.32691273155878,6.62778045055618,95.9640539688491));
#58420=CARTESIAN_POINT('Ctrl Pts',(4.55208049507337,6.47014883878998,95.9530852815463));
#58421=CARTESIAN_POINT('Ctrl Pts',(4.56718921423601,6.45949266600812,95.952344411044));
#58422=CARTESIAN_POINT('Ctrl Pts',(4.58795927230733,6.44473425297556,95.9513193449102));
#58423=CARTESIAN_POINT('Ctrl Pts',(4.59365282044811,6.44067726567226,95.9510376657455));
#58424=CARTESIAN_POINT('Ctrl Pts',(4.60271302661466,6.43420321184034,95.9505883434147));
#58425=CARTESIAN_POINT('Ctrl Pts',(4.60608318490636,6.43179103129553,95.9504209681172));
#58426=CARTESIAN_POINT('Ctrl Pts',(4.61292012632336,6.42688938167106,95.9500809353272));
#58427=CARTESIAN_POINT('Ctrl Pts',(4.61638679316003,6.42439975343267,95.9499082691961));
#58428=CARTESIAN_POINT('Ctrl Pts',(4.62433833192559,6.41867950149711,95.9495116452716));
#58429=CARTESIAN_POINT('Ctrl Pts',(4.62882183307099,6.41544698275524,95.9492875853979));
#58430=CARTESIAN_POINT('Ctrl Pts',(4.63822938347108,6.40864932281908,95.9488165682628));
#58431=CARTESIAN_POINT('Ctrl Pts',(4.64315271592294,6.40508320108781,95.9485695588241));
#58432=CARTESIAN_POINT('Ctrl Pts',(4.65616594568902,6.3956344281398,95.9479153342462));
#58433=CARTESIAN_POINT('Ctrl Pts',(4.66424878956958,6.38974211372425,95.9475076111499));
#58434=CARTESIAN_POINT('Ctrl Pts',(4.68854045188261,6.37196307676189,95.9462781937171));
#58435=CARTESIAN_POINT('Ctrl Pts',(4.70471508863984,6.36002994844121,95.9454541124694));
#58436=CARTESIAN_POINT('Ctrl Pts',(4.86344359001757,6.24198831145528,95.9373143581233));
#58437=CARTESIAN_POINT('Ctrl Pts',(5.0024237335047,6.13117060847886,95.9297685174195));
#58438=CARTESIAN_POINT('Ctrl Pts',(5.51429814914899,5.69402321241479,95.9006716992088));
#58439=CARTESIAN_POINT('Ctrl Pts',(5.85998946726534,5.33759476389158,95.8783451970682));
#58440=CARTESIAN_POINT('Ctrl Pts',(6.47242387740073,4.57438877954085,95.8354146718432));
#58441=CARTESIAN_POINT('Ctrl Pts',(6.7396453995751,4.17067808196937,95.8148765266282));
#58442=CARTESIAN_POINT('Ctrl Pts',(6.98314797155833,3.71759850361982,95.7940447956728));
#58443=CARTESIAN_POINT('Ctrl Pts',(6.99775387182588,3.69003184204701,95.7927851906566));
#58444=CARTESIAN_POINT('Ctrl Pts',(7.01787030259318,3.65151579844336,95.7910359863309));
#58445=CARTESIAN_POINT('Ctrl Pts',(7.02351896186821,3.64063903782347,95.790543201772));
#58446=CARTESIAN_POINT('Ctrl Pts',(7.03322365724367,3.62184553947672,95.7896937629072));
#58447=CARTESIAN_POINT('Ctrl Pts',(7.03729165348537,3.61393501724022,95.7893368354693));
#58448=CARTESIAN_POINT('Ctrl Pts',(7.04566369985572,3.59758721097279,95.7886004772886));
#58449=CARTESIAN_POINT('Ctrl Pts',(7.04996596030238,3.58914901769213,95.7882210869907));
#58450=CARTESIAN_POINT('Ctrl Pts',(7.05990676247647,3.56956489355508,95.7873421666059));
#58451=CARTESIAN_POINT('Ctrl Pts',(7.0655340867857,3.55841328316873,95.7868428923687));
#58452=CARTESIAN_POINT('Ctrl Pts',(7.08323791279317,3.52312222643507,95.7852666438951));
#58453=CARTESIAN_POINT('Ctrl Pts',(7.09521733419043,3.4989342012077,95.7841918891196));
#58454=CARTESIAN_POINT('Ctrl Pts',(7.30385967126524,3.07218007163691,95.7653272167629));
#58455=CARTESIAN_POINT('Ctrl Pts',(7.46610399375868,2.65367464547184,95.7484151715762));
#58456=CARTESIAN_POINT('Ctrl Pts',(7.77065112702025,1.61388463516782,95.70868260423));
#58457=CARTESIAN_POINT('Ctrl Pts',(7.87512193502151,0.984871284622181,95.6865733832196));
#58458=CARTESIAN_POINT('Ctrl Pts',(7.90781296147897,0.247110931022991,95.6580643207213));
#58459=CARTESIAN_POINT('Ctrl Pts',(7.91036337754415,0.143943204957923,95.6540147659644));
#58460=CARTESIAN_POINT('Ctrl Pts',(7.9109604597805,0.0280537537648842,95.6493701330604));
#58461=CARTESIAN_POINT('Ctrl Pts',(7.91099531099237,0.0153491394390962,
95.6488596630811));
#58462=CARTESIAN_POINT('Ctrl Pts',(7.91100147895069,-0.00310191107860394,
95.6481163626843));
#58463=CARTESIAN_POINT('Ctrl Pts',(7.91099713867137,-0.00884836093567081,
95.6478845938201));
#58464=CARTESIAN_POINT('Ctrl Pts',(7.9109784577727,-0.0189741893473824,
95.6474757052003));
#58465=CARTESIAN_POINT('Ctrl Pts',(7.91096674178525,-0.0233535748588086,
95.6472987013354));
#58466=CARTESIAN_POINT('Ctrl Pts',(7.91093538774854,-0.0322974604931215,
95.6469368794338));
#58467=CARTESIAN_POINT('Ctrl Pts',(7.91091543571675,-0.0368619572749811,
95.6467520474831));
#58468=CARTESIAN_POINT('Ctrl Pts',(7.91085485507063,-0.0484305851894007,
95.6462831414925));
#58469=CARTESIAN_POINT('Ctrl Pts',(7.9108088749487,-0.0554346744395597,
95.6459988270105));
#58470=CARTESIAN_POINT('Ctrl Pts',(7.91068970315355,-0.0705333082266814,
95.6453850108176));
#58471=CARTESIAN_POINT('Ctrl Pts',(7.9106133891904,-0.0786278141427979,
95.6450553669859));
#58472=CARTESIAN_POINT('Ctrl Pts',(7.91036130516155,-0.101622130730678,
95.644117281685));
#58473=CARTESIAN_POINT('Ctrl Pts',(7.9101558622616,-0.116521523949013,95.6435074651082));
#58474=CARTESIAN_POINT('Ctrl Pts',(7.90789931916879,-0.252338191318515,
95.6379299946108));
#58475=CARTESIAN_POINT('Ctrl Pts',(7.90311821115909,-0.373180210877427,
95.6328236809456));
#58476=CARTESIAN_POINT('Ctrl Pts',(7.88418649428543,-0.675852062245692,
95.6197327206794));
#58477=CARTESIAN_POINT('Ctrl Pts',(7.86651429446798,-0.857391148501546,
95.6116138226172));
#58478=CARTESIAN_POINT('Ctrl Pts',(7.7396488046092,-1.8157835800511,95.5678713233792));
#58479=CARTESIAN_POINT('Ctrl Pts',(7.52158521407871,-2.57398035063378,95.5307291673917));
#58480=CARTESIAN_POINT('Ctrl Pts',(7.12630885129493,-3.43909238697278,95.490428268475));
#58481=CARTESIAN_POINT('Ctrl Pts',(7.0523608937518,-3.58829271828867,95.4835338276845));
#58482=CARTESIAN_POINT('Ctrl Pts',(6.96597612026184,-3.74958254701549,95.4761406356499));
#58483=CARTESIAN_POINT('Ctrl Pts',(6.95815001769743,-3.76408566859512,95.4754763723515));
#58484=CARTESIAN_POINT('Ctrl Pts',(6.94646287912882,-3.78558295252171,95.4744925383661));
#58485=CARTESIAN_POINT('Ctrl Pts',(6.94263650005714,-3.79259584586781,95.4741717121122));
#58486=CARTESIAN_POINT('Ctrl Pts',(6.93606874107987,-3.80458982612083,95.4736232180157));
#58487=CARTESIAN_POINT('Ctrl Pts',(6.93333260574277,-3.80957376937896,95.4733953597574));
#58488=CARTESIAN_POINT('Ctrl Pts',(6.92800003494938,-3.81926241456342,95.4729525281461));
#58489=CARTESIAN_POINT('Ctrl Pts',(6.92540417430987,-3.8239674290153,95.4727375340056));
#58490=CARTESIAN_POINT('Ctrl Pts',(6.91918593370908,-3.8352109313663,95.47222389482));
#58491=CARTESIAN_POINT('Ctrl Pts',(6.91555907373427,-3.84174694265455,95.4719254134196));
#58492=CARTESIAN_POINT('Ctrl Pts',(6.90466663136792,-3.86131094659894,95.4710322894314));
#58493=CARTESIAN_POINT('Ctrl Pts',(6.89737343954427,-3.87432357390493,95.4704386567344));
#58494=CARTESIAN_POINT('Ctrl Pts',(6.8342466184071,-3.98621223752896,95.465337782217));
#58495=CARTESIAN_POINT('Ctrl Pts',(6.77632565822755,-4.08389847780468,95.4609079636657));
#58496=CARTESIAN_POINT('Ctrl Pts',(6.55271971283597,-4.44315659688029,95.4446800500562));
#58497=CARTESIAN_POINT('Ctrl Pts',(6.37382339793422,-4.69618696554919,95.4333921661365));
#58498=CARTESIAN_POINT('Ctrl Pts',(6.12826189041585,-5.0035330466164,95.4195294767092));
#58499=CARTESIAN_POINT('Ctrl Pts',(6.07494189191457,-5.06813753133873,95.4166053423248));
#58500=CARTESIAN_POINT('Ctrl Pts',(5.97789021372658,-5.18199628056737,95.411419967502));
#58501=CARTESIAN_POINT('Ctrl Pts',(5.9345507152443,-5.23157383298663,95.4091508968986));
#58502=CARTESIAN_POINT('Ctrl Pts',(5.8730807791824,-5.30014450562309,95.405991042055));
#58503=CARTESIAN_POINT('Ctrl Pts',(5.85546735330848,-5.31959694890057,95.4050921668097));
#58504=CARTESIAN_POINT('Ctrl Pts',(5.55213582317947,-5.65126742785444,95.3897188542991));
#58505=CARTESIAN_POINT('Ctrl Pts',(5.24192488393845,-5.94013769148073,95.3756480182444));
#58506=CARTESIAN_POINT('Ctrl Pts',(4.80148059006422,-6.28879165578663,95.3558333616111));
#58507=CARTESIAN_POINT('Ctrl Pts',(4.6906124217845,-6.37191251300519,95.3508544034811));
#58508=CARTESIAN_POINT('Ctrl Pts',(4.55278050932077,-6.46970157012527,95.3446047539564));
#58509=CARTESIAN_POINT('Ctrl Pts',(4.52783700989365,-6.48718280547461,95.3434714176188));
#58510=CARTESIAN_POINT('Ctrl Pts',(4.49499273027959,-6.50991945924464,95.3419752280939));
#58511=CARTESIAN_POINT('Ctrl Pts',(4.48718237500114,-6.51530546816884,95.3416191495336));
#58512=CARTESIAN_POINT('Ctrl Pts',(4.46081176082387,-6.53342069296401,95.3404158729057));
#58513=CARTESIAN_POINT('Ctrl Pts',(4.44220698416954,-6.54608467805241,95.3395652384501));
#58514=CARTESIAN_POINT('Ctrl Pts',(4.3333908894268,-6.61947659312442,95.334578603352));
#58515=CARTESIAN_POINT('Ctrl Pts',(4.24199269292435,-6.6784162044943,95.3303445840752));
#58516=CARTESIAN_POINT('Ctrl Pts',(4.14063981682945,-6.74085521857821,95.3255685132271));
#58517=CARTESIAN_POINT('Ctrl Pts',(4.13185652479245,-6.74624257102798,95.3251539613083));
#58518=CARTESIAN_POINT('Ctrl Pts',(4.11951277513632,-6.75378062997216,95.324570410515));
#58519=CARTESIAN_POINT('Ctrl Pts',(4.11596107489648,-6.75594573188014,95.3244023933466));
#58520=CARTESIAN_POINT('Ctrl Pts',(4.10979757449692,-6.75969631210862,95.3241106275984));
#58521=CARTESIAN_POINT('Ctrl Pts',(4.10718656696544,-6.76128307641224,95.3239869680038));
#58522=CARTESIAN_POINT('Ctrl Pts',(4.10173077160193,-6.7645943517686,95.3237284499449));
#58523=CARTESIAN_POINT('Ctrl Pts',(4.09888582659349,-6.76631857417094,95.3235935729748));
#58524=CARTESIAN_POINT('Ctrl Pts',(4.0932252602235,-6.76974436682504,95.3233250680442));
#58525=CARTESIAN_POINT('Ctrl Pts',(4.09040966320588,-6.77144597631699,95.3231914428002));
#58526=CARTESIAN_POINT('Ctrl Pts',(4.08076953315591,-6.77726379409537,95.3227336974347));
#58527=CARTESIAN_POINT('Ctrl Pts',(4.07393986171649,-6.78137143354564,95.3224089991073));
#58528=CARTESIAN_POINT('Ctrl Pts',(4.01934903745053,-6.81409232130996,95.3198104914728));
#58529=CARTESIAN_POINT('Ctrl Pts',(3.97129431555447,-6.84221031664508,95.3175039705246));
#58530=CARTESIAN_POINT('Ctrl Pts',(3.88357842027876,-6.8922996915149,95.3132654707816));
#58531=CARTESIAN_POINT('Ctrl Pts',(3.84401702244457,-6.91444208687771,95.3113435409427));
#58532=CARTESIAN_POINT('Ctrl Pts',(3.63155808427749,-7.03096782006894,95.3009769505302));
#58533=CARTESIAN_POINT('Ctrl Pts',(3.45537899008134,-7.11920432783974,95.2922232941175));
#58534=CARTESIAN_POINT('Ctrl Pts',(3.11123331981325,-7.27577873463573,95.2750923021324));
#58535=CARTESIAN_POINT('Ctrl Pts',(2.9438407174519,-7.34510232297456,95.2667461559348));
#58536=CARTESIAN_POINT('Ctrl Pts',(2.06707970768347,-7.6734129808907,95.2234325262404));
#58537=CARTESIAN_POINT('Ctrl Pts',(1.32550737130842,-7.83565855316587,95.1886640535721));
#58538=CARTESIAN_POINT('Ctrl Pts',(0.521653668279351,-7.89394435891763,
95.1557175455155));
#58539=CARTESIAN_POINT('Ctrl Pts',(0.471164131292514,-7.89711875185553,
95.1536652463703));
#58540=CARTESIAN_POINT('Ctrl Pts',(0.409399090820432,-7.90040760074296,
95.1511750679712));
#58541=CARTESIAN_POINT('Ctrl Pts',(0.398149916969068,-7.90098250336392,
95.150722363599));
#58542=CARTESIAN_POINT('Ctrl Pts',(0.379591352055105,-7.90189122570356,
95.1499768633924));
#58543=CARTESIAN_POINT('Ctrl Pts',(0.372282675856617,-7.90223893254604,
95.1496836202885));
#58544=CARTESIAN_POINT('Ctrl Pts',(0.359106631340507,-7.90284745652252,
95.1491555870889));
#58545=CARTESIAN_POINT('Ctrl Pts',(0.35323943976293,-7.90311188027419,95.1489206809553));
#58546=CARTESIAN_POINT('Ctrl Pts',(0.340721676997566,-7.90366206580223,
95.1484199785691));
#58547=CARTESIAN_POINT('Ctrl Pts',(0.334071026284338,-7.90394596775951,
95.1481542424011));
#58548=CARTESIAN_POINT('Ctrl Pts',(0.31615561358695,-7.90468808571513,95.1474391729731));
#58549=CARTESIAN_POINT('Ctrl Pts',(0.304890197781676,-7.90513061708256,
95.1469903451119));
#58550=CARTESIAN_POINT('Ctrl Pts',(0.250163444438829,-7.90716325004988,
95.1448139015453));
#58551=CARTESIAN_POINT('Ctrl Pts',(0.20669004047878,-7.90841904034461,95.1430970606715));
#58552=CARTESIAN_POINT('Ctrl Pts',(-0.140689022857492,-7.91558717594761,
95.1294719355703));
#58553=CARTESIAN_POINT('Ctrl Pts',(-0.444706584661031,-7.90433876599977,
95.1181337303915));
#58554=CARTESIAN_POINT('Ctrl Pts',(-0.835557652057764,-7.86724958881508,
95.1040209634873));
#58555=CARTESIAN_POINT('Ctrl Pts',(-0.923625238184442,-7.85739711939494,
95.1008705287899));
#58556=CARTESIAN_POINT('Ctrl Pts',(-1.07937530838483,-7.83731792219948,
95.0953362966764));
#58557=CARTESIAN_POINT('Ctrl Pts',(-1.14712488797719,-7.8276885414694,95.0929415519603));
#58558=CARTESIAN_POINT('Ctrl Pts',(-1.26982234701836,-7.80862211688347,
95.0886195023416));
#58559=CARTESIAN_POINT('Ctrl Pts',(-1.32481141386337,-7.79948093997826,
95.0866879634762));
#58560=CARTESIAN_POINT('Ctrl Pts',(-1.4257120843574,-7.78160970646244,95.0831490827152));
#58561=CARTESIAN_POINT('Ctrl Pts',(-1.47165165390885,-7.77305255389568,
95.0815398910726));
#58562=CARTESIAN_POINT('Ctrl Pts',(-1.55664063001131,-7.75644122129672,
95.0785636718615));
#58563=CARTESIAN_POINT('Ctrl Pts',(-1.59571011310113,-7.74849790060409,
95.0771958202496));
#58564=CARTESIAN_POINT('Ctrl Pts',(-1.66839039044674,-7.73314805965238,
95.0746498727215));
#58565=CARTESIAN_POINT('Ctrl Pts',(-1.70201610058914,-7.72581688913321,
95.073471439474));
#58566=CARTESIAN_POINT('Ctrl Pts',(-1.76481763856816,-7.71169481851153,
95.0712681943196));
#58567=CARTESIAN_POINT('Ctrl Pts',(-1.79400479677381,-7.70495717451094,
95.070243286642));
#58568=CARTESIAN_POINT('Ctrl Pts',(-2.05607277280654,-7.6428908369447,95.0610279870779));
#58569=CARTESIAN_POINT('Ctrl Pts',(-2.28636442937645,-7.57718607263496,
95.0528430246915));
#58570=CARTESIAN_POINT('Ctrl Pts',(-2.5985746387371,-7.47257757876964,95.0412541892609));
#58571=CARTESIAN_POINT('Ctrl Pts',(-2.68333735706123,-7.44256044172943,
95.0380561930982));
#58572=CARTESIAN_POINT('Ctrl Pts',(-2.8208036564316,-7.39122567103771,95.0327591034406));
#58573=CARTESIAN_POINT('Ctrl Pts',(-2.87382234159582,-7.37077303711419,
95.030688828321));
#58574=CARTESIAN_POINT('Ctrl Pts',(-3.02771963097993,-7.30949230095951,
95.0245876584046));
#58575=CARTESIAN_POINT('Ctrl Pts',(-3.1279791622638,-7.26715271925829,95.0204969962022));
#58576=CARTESIAN_POINT('Ctrl Pts',(-3.29685533113464,-7.19169415343764,
95.0133577850994));
#58577=CARTESIAN_POINT('Ctrl Pts',(-3.36592649425091,-7.15962694649186,
95.0103654147929));
#58578=CARTESIAN_POINT('Ctrl Pts',(-3.44317354892224,-7.12239911465496,
95.0069251974037));
#58579=CARTESIAN_POINT('Ctrl Pts',(-3.45181759066862,-7.11821385992573,
95.0065389007169));
#58580=CARTESIAN_POINT('Ctrl Pts',(-3.46439729215422,-7.11209474285413,
95.0059747497932));
#58581=CARTESIAN_POINT('Ctrl Pts',(-3.46833902625495,-7.11017331912517,
95.0057976956941));
#58582=CARTESIAN_POINT('Ctrl Pts',(-3.47532836852941,-7.10675912404705,
95.0054832510523));
#58583=CARTESIAN_POINT('Ctrl Pts',(-3.47837662203386,-7.10526766501806,
95.0053459442695));
#58584=CARTESIAN_POINT('Ctrl Pts',(-3.48471077716072,-7.10216341672086,
95.005060277344));
#58585=CARTESIAN_POINT('Ctrl Pts',(-3.48799652032283,-7.10055030771549,
95.0049118969289));
#58586=CARTESIAN_POINT('Ctrl Pts',(-3.49464347753956,-7.09728131080127,
95.004611334652));
#58587=CARTESIAN_POINT('Ctrl Pts',(-3.49800463687692,-7.09562531423809,
95.0044591459555));
#58588=CARTESIAN_POINT('Ctrl Pts',(-3.51171456280598,-7.08885851507637,
95.0038375518356));
#58589=CARTESIAN_POINT('Ctrl Pts',(-3.52205326952894,-7.08372747791444,
95.003366880561));
#58590=CARTESIAN_POINT('Ctrl Pts',(-3.54670056530895,-7.07142787736745,
95.0022402792389));
#58591=CARTESIAN_POINT('Ctrl Pts',(-3.56099865858581,-7.06423850612756,
95.0015830760549));
#58592=CARTESIAN_POINT('Ctrl Pts',(-3.61213601179585,-7.03833090575854,
94.9992197514299));
#58593=CARTESIAN_POINT('Ctrl Pts',(-3.64884979673683,-7.01936774610433,
94.9974991058404));
#58594=CARTESIAN_POINT('Ctrl Pts',(-3.82474630719198,-6.92676198961938,
94.9891463181309));
#58595=CARTESIAN_POINT('Ctrl Pts',(-3.96185200239226,-6.84926563281959,
94.9823052165882));
#58596=CARTESIAN_POINT('Ctrl Pts',(-4.24703799965829,-6.67664098756959,
94.9675123647928));
#58597=CARTESIAN_POINT('Ctrl Pts',(-4.39444466433054,-6.58055611967386,
94.9595287808172));
#58598=CARTESIAN_POINT('Ctrl Pts',(-5.22817358315865,-5.99658921201034,
94.912881515185));
#58599=CARTESIAN_POINT('Ctrl Pts',(-5.83648164011667,-5.40638005550013,
94.8735945380329));
#58600=CARTESIAN_POINT('Ctrl Pts',(-6.35351839553867,-4.71351426008008,
94.838188725876));
#58601=CARTESIAN_POINT('Ctrl Pts',(-6.36670511139438,-4.6956872465497,94.837283488634));
#58602=CARTESIAN_POINT('Ctrl Pts',(-6.39796056288868,-4.653059549026,94.8351324641867));
#58603=CARTESIAN_POINT('Ctrl Pts',(-6.4159603599717,-4.62820864026608,94.8338893336724));
#58604=CARTESIAN_POINT('Ctrl Pts',(-6.44150492378747,-4.592505847453,94.8321187169016));
#58605=CARTESIAN_POINT('Ctrl Pts',(-6.44916767898572,-4.58173895945378,
94.8315867354146));
#58606=CARTESIAN_POINT('Ctrl Pts',(-6.46141661383981,-4.56443644798761,
94.8307349989255));
#58607=CARTESIAN_POINT('Ctrl Pts',(-6.46601992554832,-4.5579130167451,94.8304145939304));
#58608=CARTESIAN_POINT('Ctrl Pts',(-6.47416422596977,-4.54633442105535,
94.8298471689599));
#58609=CARTESIAN_POINT('Ctrl Pts',(-6.47770918566968,-4.54128206556374,
94.8295999987868));
#58610=CARTESIAN_POINT('Ctrl Pts',(-6.48506212336788,-4.53077636785321,
94.8290869270475));
#58611=CARTESIAN_POINT('Ctrl Pts',(-6.48886914460541,-4.52532236021936,
94.8288210617022));
#58612=CARTESIAN_POINT('Ctrl Pts',(-6.49867150071204,-4.51124152442456,
94.8281359380797));
#58613=CARTESIAN_POINT('Ctrl Pts',(-6.50465654649882,-4.50260753109031,
94.827717067546));
#58614=CARTESIAN_POINT('Ctrl Pts',(-6.5295641324309,-4.46652267986299,94.8259715463715));
#58615=CARTESIAN_POINT('Ctrl Pts',(-6.54833036445675,-4.43896407750389,
94.8246507634209));
#58616=CARTESIAN_POINT('Ctrl Pts',(-6.9111097859029,-3.89890764743114,94.7990036478572));
#58617=CARTESIAN_POINT('Ctrl Pts',(-7.1941493870557,-3.34801661001925,94.7772041452471));
#58618=CARTESIAN_POINT('Ctrl Pts',(-7.5166397559977,-2.48522205699581,94.7452885636553));
#58619=CARTESIAN_POINT('Ctrl Pts',(-7.60651665330224,-2.19478873464313,
94.7348434541119));
#58620=CARTESIAN_POINT('Ctrl Pts',(-7.68550613291464,-1.87551284303654,
94.7231039859478));
#58621=CARTESIAN_POINT('Ctrl Pts',(-7.69142704885645,-1.85108154474591,
94.7222040048995));
#58622=CARTESIAN_POINT('Ctrl Pts',(-7.75976796656916,-1.56309875417223,
94.7115720109154));
#58623=CARTESIAN_POINT('Ctrl Pts',(-7.80872562243552,-1.29655632823456,
94.7015029458659));
#58624=CARTESIAN_POINT('Ctrl Pts',(-7.84617868433132,-1.01079375066152,
94.6900007419919));
#58625=CARTESIAN_POINT('Ctrl Pts',(-7.84838359321396,-0.993528518801242,
94.6893030667345));
#58626=CARTESIAN_POINT('Ctrl Pts',(-7.85126729831774,-0.970339302682182,
94.6883621782437));
#58627=CARTESIAN_POINT('Ctrl Pts',(-7.85199641434497,-0.964421516102439,
94.688121733019));
#58628=CARTESIAN_POINT('Ctrl Pts',(-7.85312814531741,-0.955149593307012,
94.6877444744673));
#58629=CARTESIAN_POINT('Ctrl Pts',(-7.8535353045176,-0.951796003879657,
94.6876079137751));
#58630=CARTESIAN_POINT('Ctrl Pts',(-7.85431269415618,-0.945358529794674,
94.6873455642451));
#58631=CARTESIAN_POINT('Ctrl Pts',(-7.85468325563197,-0.942274695110274,
94.6872197942365));
#58632=CARTESIAN_POINT('Ctrl Pts',(-7.85544404598348,-0.935911718842001,
94.6869600974984));
#58633=CARTESIAN_POINT('Ctrl Pts',(-7.85583403745094,-0.932632554122576,
94.6868261578452));
#58634=CARTESIAN_POINT('Ctrl Pts',(-7.8567080606465,-0.925244060060944,
94.6865241354947));
#58635=CARTESIAN_POINT('Ctrl Pts',(-7.85719092152125,-0.921134595786033,
94.6863559879775));
#58636=CARTESIAN_POINT('Ctrl Pts',(-7.8583991339679,-0.910781837859483,
94.6859319747023));
#58637=CARTESIAN_POINT('Ctrl Pts',(-7.85912026847479,-0.904538064512101,
94.6856758775308));
#58638=CARTESIAN_POINT('Ctrl Pts',(-7.86114391800167,-0.886831657786628,
94.6849485780216));
#58639=CARTESIAN_POINT('Ctrl Pts',(-7.86242879718593,-0.875367063256885,
94.6844764211321));
#58640=CARTESIAN_POINT('Ctrl Pts',(-7.89514288584353,-0.577585515755989,
94.6721810951628));
#58641=CARTESIAN_POINT('Ctrl Pts',(-7.91093383073369,-0.289793073497133,
94.6595472812891));
#58642=CARTESIAN_POINT('Ctrl Pts',(-7.91099979248103,-0.00181200581611723,
94.6465781220462));
#58643=CARTESIAN_POINT('',(-7.90011696396554,-0.00322646772645097,92.6423315082368));
#58644=CARTESIAN_POINT('Ctrl Pts',(-7.91859353182819,-0.00199197810995973,
94.6422060731203));
#58645=CARTESIAN_POINT('Ctrl Pts',(-7.90063021708447,2.30671988041081,94.5490207070605));
#58646=CARTESIAN_POINT('Ctrl Pts',(-5.62081845448744,7.26898411856701,94.3499009611984));
#58647=CARTESIAN_POINT('Ctrl Pts',(2.82775288885835,8.91884816508282,94.0448468355335));
#58648=CARTESIAN_POINT('Ctrl Pts',(7.97825124714588,3.53469384178973,93.7800108860271));
#58649=CARTESIAN_POINT('Ctrl Pts',(8.0010321747323,-1.8993409012976,93.568142126422));
#58650=CARTESIAN_POINT('Ctrl Pts',(5.53837391557236,-6.74336473053567,93.3562733668169));
#58651=CARTESIAN_POINT('Ctrl Pts',(-1.48249292472398,-9.23819537141634,
93.0914374173105));
#58652=CARTESIAN_POINT('Ctrl Pts',(-7.18564508454347,-4.8210665441833,92.8358010678166));
#58653=CARTESIAN_POINT('Ctrl Pts',(-7.90503420534493,-1.0943581354185,92.6860990981254));
#58654=CARTESIAN_POINT('Ctrl Pts',(-7.90011696396554,-0.00322646772645097,
92.6423315082368));
#58655=CARTESIAN_POINT('',(-7.91099997228721,-0.000662171981131852,88.6422897498906));
#58656=CARTESIAN_POINT('Ctrl Pts',(-7.91099969560253,-0.00219457893313992,
92.6359954548207));
#58657=CARTESIAN_POINT('Ctrl Pts',(-7.91105851759497,0.209846445081939,
92.6268999841067));
#58658=CARTESIAN_POINT('Ctrl Pts',(-7.9025923153044,0.421815546310325,92.6180528499363));
#58659=CARTESIAN_POINT('Ctrl Pts',(-7.88438988738471,0.648500291604092,
92.6088487635085));
#58660=CARTESIAN_POINT('Ctrl Pts',(-7.88311700052855,0.66379430843469,92.6082290211759));
#58661=CARTESIAN_POINT('Ctrl Pts',(-7.88101772303028,0.688159586406447,
92.6072436550318));
#58662=CARTESIAN_POINT('Ctrl Pts',(-7.88022015914638,0.697233254499654,
92.6068771366448));
#58663=CARTESIAN_POINT('Ctrl Pts',(-7.87882641729278,0.712781566837111,
92.6062498227486));
#58664=CARTESIAN_POINT('Ctrl Pts',(-7.87823792579363,0.719256880884172,
92.6059887887333));
#58665=CARTESIAN_POINT('Ctrl Pts',(-7.87711755418358,0.731418246590784,
92.6054989485463));
#58666=CARTESIAN_POINT('Ctrl Pts',(-7.87658749899853,0.737104459807619,
92.6052700858565));
#58667=CARTESIAN_POINT('Ctrl Pts',(-7.87547113004988,0.748941692255273,
92.604794002735));
#58668=CARTESIAN_POINT('Ctrl Pts',(-7.87488376609128,0.755092609830475,
92.604546815086));
#58669=CARTESIAN_POINT('Ctrl Pts',(-7.87351668311397,0.769233704006001,
92.6039789759759));
#58670=CARTESIAN_POINT('Ctrl Pts',(-7.87273200591303,0.777223400451342,
92.6036584787005));
#58671=CARTESIAN_POINT('Ctrl Pts',(-7.87020481733334,0.802559064060222,
92.6026432118215));
#58672=CARTESIAN_POINT('Ctrl Pts',(-7.86841712478824,0.819900526493182,
92.6019498454834));
#58673=CARTESIAN_POINT('Ctrl Pts',(-7.85288242772919,0.965862732405452,
92.5961267035342));
#58674=CARTESIAN_POINT('Ctrl Pts',(-7.83603969881355,1.09413755258958,92.5910939722459));
#58675=CARTESIAN_POINT('Ctrl Pts',(-7.80584624329514,1.28726711135937,92.5836267029349));
#58676=CARTESIAN_POINT('Ctrl Pts',(-7.79481542313479,1.35245884996004,92.5811250777143));
#58677=CARTESIAN_POINT('Ctrl Pts',(-7.77699466231457,1.45030567744718,92.5773956392605));
#58678=CARTESIAN_POINT('Ctrl Pts',(-7.77081347839506,1.48306791736901,92.5761511793994));
#58679=CARTESIAN_POINT('Ctrl Pts',(-7.6015663204633,2.35001297557888,92.5433254814008));
#58680=CARTESIAN_POINT('Ctrl Pts',(-7.30537456069535,3.15238720903557,92.516238157304));
#58681=CARTESIAN_POINT('Ctrl Pts',(-6.81143773150459,4.02641317570069,92.4788927379328));
#58682=CARTESIAN_POINT('Ctrl Pts',(-6.73168681114499,4.15837408036783,92.4729968154714));
#58683=CARTESIAN_POINT('Ctrl Pts',(-6.63556652386427,4.30740243070224,92.4659427291885));
#58684=CARTESIAN_POINT('Ctrl Pts',(-6.62291139060358,4.32683527358116,92.4650149656115));
#58685=CARTESIAN_POINT('Ctrl Pts',(-6.60666146678254,4.35154984729354,92.4638245350057));
#58686=CARTESIAN_POINT('Ctrl Pts',(-6.6031453634022,4.35688341816635,92.4635670051766));
#58687=CARTESIAN_POINT('Ctrl Pts',(-6.59750073511855,4.36542321667416,92.4631536487802));
#58688=CARTESIAN_POINT('Ctrl Pts',(-6.59537631833245,4.36863216923219,92.4629980941192));
#58689=CARTESIAN_POINT('Ctrl Pts',(-6.59134021137476,4.37471909443704,92.4627025899146));
#58690=CARTESIAN_POINT('Ctrl Pts',(-6.58942898139068,4.37759735887083,92.4625626708715));
#58691=CARTESIAN_POINT('Ctrl Pts',(-6.58506060195004,4.38416668594942,92.4622428948387));
#58692=CARTESIAN_POINT('Ctrl Pts',(-6.58260223660566,4.38785693204065,92.46206295701));
#58693=CARTESIAN_POINT('Ctrl Pts',(-6.57620583053257,4.39744108782498,92.4615948353808));
#58694=CARTESIAN_POINT('Ctrl Pts',(-6.57226297632234,4.4033317630924,92.4613063337003));
#58695=CARTESIAN_POINT('Ctrl Pts',(-6.54807674663601,4.43936144908981,92.4595369950926));
#58696=CARTESIAN_POINT('Ctrl Pts',(-6.52763429067639,4.46936568711325,92.4580431850561));
#58697=CARTESIAN_POINT('Ctrl Pts',(-6.00413677071108,5.22647144726505,92.4198534733533));
#58698=CARTESIAN_POINT('Ctrl Pts',(-5.38292425930104,5.86430720502408,92.3768012509461));
#58699=CARTESIAN_POINT('Ctrl Pts',(-4.54610465492637,6.47611322922637,92.3312036225391));
#58700=CARTESIAN_POINT('Ctrl Pts',(-4.42060228472279,6.56242246675968,92.3246124638779));
#58701=CARTESIAN_POINT('Ctrl Pts',(-4.18949681892611,6.71171571718086,92.3129318597991));
#58702=CARTESIAN_POINT('Ctrl Pts',(-4.08477002398745,6.7759624461401,92.3077998653555));
#58703=CARTESIAN_POINT('Ctrl Pts',(-3.94192354482427,6.85907858193862,92.3010135394244));
#58704=CARTESIAN_POINT('Ctrl Pts',(-3.90508950567532,6.88011600570095,92.2992822670268));
#58705=CARTESIAN_POINT('Ctrl Pts',(-3.84322658782748,6.91479158455034,92.2964053739942));
#58706=CARTESIAN_POINT('Ctrl Pts',(-3.81829022167556,6.92859243051359,92.295253998719));
#58707=CARTESIAN_POINT('Ctrl Pts',(-3.78461970882579,6.94699014281267,92.293710372752));
#58708=CARTESIAN_POINT('Ctrl Pts',(-3.77595090210772,6.95170577416422,92.2933139299413));
#58709=CARTESIAN_POINT('Ctrl Pts',(-3.76224404624432,6.95912878510216,92.2926886268815));
#58710=CARTESIAN_POINT('Ctrl Pts',(-3.75721185951068,6.96184693555287,92.2924593871027));
#58711=CARTESIAN_POINT('Ctrl Pts',(-3.74677648450689,6.96746902413583,92.2919846832596));
#58712=CARTESIAN_POINT('Ctrl Pts',(-3.74137285653161,6.97037214040768,92.291739248224));
#58713=CARTESIAN_POINT('Ctrl Pts',(-3.72905217612777,6.97697301030253,92.2911804907319));
#58714=CARTESIAN_POINT('Ctrl Pts',(-3.72213298526401,6.98066677039058,92.2908673088237));
#58715=CARTESIAN_POINT('Ctrl Pts',(-3.70104726704151,6.99188296554728,92.2899147662972));
#58716=CARTESIAN_POINT('Ctrl Pts',(-3.68686330557181,6.99937263236242,92.2892765561656));
#58717=CARTESIAN_POINT('Ctrl Pts',(-3.58598624415169,7.05224780997988,92.2847555245803));
#58718=CARTESIAN_POINT('Ctrl Pts',(-3.49847871492722,7.09606539169732,92.2809277782003));
#58719=CARTESIAN_POINT('Ctrl Pts',(-3.39661733613499,7.14472795544981,92.2765744928683));
#58720=CARTESIAN_POINT('Ctrl Pts',(-3.38303745771577,7.15116804781961,92.2759961946749));
#58721=CARTESIAN_POINT('Ctrl Pts',(-3.3513091810233,7.16610419373216,92.2746498236176));
#58722=CARTESIAN_POINT('Ctrl Pts',(-3.33314665921872,7.17457008448912,92.2738827409246));
#58723=CARTESIAN_POINT('Ctrl Pts',(-3.28587445936161,7.19638628934921,92.2718955196939));
#58724=CARTESIAN_POINT('Ctrl Pts',(-3.25671542540773,7.20962906489997,92.2706788547085));
#58725=CARTESIAN_POINT('Ctrl Pts',(-2.94408995168285,7.34932643068024,92.2577293056811));
#58726=CARTESIAN_POINT('Ctrl Pts',(-2.65348603731244,7.45917514808436,92.2465377561428));
#58727=CARTESIAN_POINT('Ctrl Pts',(-2.19018988732876,7.60378763692748,92.2295013132248));
#58728=CARTESIAN_POINT('Ctrl Pts',(-2.02153022868916,7.65035522292941,92.2234563463252));
#58729=CARTESIAN_POINT('Ctrl Pts',(-1.80418506162899,7.70267499569685,92.2157628921704));
#58730=CARTESIAN_POINT('Ctrl Pts',(-1.75680216213463,7.71361990225679,92.2140913479165));
#58731=CARTESIAN_POINT('Ctrl Pts',(-1.6554992877257,7.7360378607968,92.210525620853));
#58732=CARTESIAN_POINT('Ctrl Pts',(-1.6015542545544,7.74738560019631,92.2086316207692));
#58733=CARTESIAN_POINT('Ctrl Pts',(-1.48518141744433,7.77059808771909,92.2045497162404));
#58734=CARTESIAN_POINT('Ctrl Pts',(-1.4227204399175,7.78227633726094,92.2023612500642));
#58735=CARTESIAN_POINT('Ctrl Pts',(-1.16967108472931,7.82644034014148,92.1934856010407));
#58736=CARTESIAN_POINT('Ctrl Pts',(-0.978066289309218,7.8526862631623,92.1867446703331));
#58737=CARTESIAN_POINT('Ctrl Pts',(-0.630835780870365,7.88734356043161,
92.1742286322654));
#58738=CARTESIAN_POINT('Ctrl Pts',(-0.475556835398854,7.89822664976303,
92.1685237897499));
#58739=CARTESIAN_POINT('Ctrl Pts',(-0.213602466437318,7.90883352515315,
92.158580021996));
#58740=CARTESIAN_POINT('Ctrl Pts',(-0.107068222776297,7.91099288418527,
92.1544470213325));
#58741=CARTESIAN_POINT('Ctrl Pts',(0.0178117056317007,7.91100120425473,
92.1494661920746));
#58742=CARTESIAN_POINT('Ctrl Pts',(0.0361502868546076,7.91093865840583,
92.1487313178149));
#58743=CARTESIAN_POINT('Ctrl Pts',(0.0602682416766564,7.91077253799182,
92.1477601402533));
#58744=CARTESIAN_POINT('Ctrl Pts',(0.0660480795086562,7.91072639266852,
92.1475270430651));
#58745=CARTESIAN_POINT('Ctrl Pts',(0.0754864062318918,7.91064069394077,
92.1471458133601));
#58746=CARTESIAN_POINT('Ctrl Pts',(0.0791449359376056,7.9106049367408,92.1469978949909));
#58747=CARTESIAN_POINT('Ctrl Pts',(0.0861973944782431,7.91053111550779,
92.1467124761048));
#58748=CARTESIAN_POINT('Ctrl Pts',(0.0895913269889974,7.9104934052366,92.1465749957036));
#58749=CARTESIAN_POINT('Ctrl Pts',(0.0973737452483848,7.91040192502701,
92.1462594589034));
#58750=CARTESIAN_POINT('Ctrl Pts',(0.101762210858887,7.91034668734927,92.146081318644));
#58751=CARTESIAN_POINT('Ctrl Pts',(0.113495557822266,7.9101892339032,92.1456044604224));
#58752=CARTESIAN_POINT('Ctrl Pts',(0.120840329490297,7.91008044029093,92.1453053641667));
#58753=CARTESIAN_POINT('Ctrl Pts',(0.172571573389788,7.90924210938661,92.1431946086891));
#58754=CARTESIAN_POINT('Ctrl Pts',(0.216950567435492,7.90814921434101,92.1413623840763));
#58755=CARTESIAN_POINT('Ctrl Pts',(1.04327903554448,7.88083892319907,92.1068788200323));
#58756=CARTESIAN_POINT('Ctrl Pts',(1.81707851426582,7.73914574533819,92.0689208229441));
#58757=CARTESIAN_POINT('Ctrl Pts',(2.77641978593125,7.41140519833461,92.0231714256398));
#58758=CARTESIAN_POINT('Ctrl Pts',(2.99195000986717,7.32705122680046,92.012943285491));
#58759=CARTESIAN_POINT('Ctrl Pts',(3.335583903202,7.17486403319679,91.9968092227138));
#58760=CARTESIAN_POINT('Ctrl Pts',(3.46605983125185,7.11275095054063,91.9907243895281));
#58761=CARTESIAN_POINT('Ctrl Pts',(3.64105116944718,7.02348681896551,91.9826219832238));
#58762=CARTESIAN_POINT('Ctrl Pts',(3.68710274780054,6.99942098899477,91.9804952591379));
#58763=CARTESIAN_POINT('Ctrl Pts',(3.75233349247625,6.96450999501693,91.9774904057377));
#58764=CARTESIAN_POINT('Ctrl Pts',(3.77170909898301,6.95403599305077,91.9765988295734));
#58765=CARTESIAN_POINT('Ctrl Pts',(3.80571597703659,6.93546872687078,91.9750356361475));
#58766=CARTESIAN_POINT('Ctrl Pts',(3.8203657573067,6.92740976442581,91.9743627704967));
#58767=CARTESIAN_POINT('Ctrl Pts',(3.8417791514485,6.91554149754192,91.9733800240035));
#58768=CARTESIAN_POINT('Ctrl Pts',(3.84856283499525,6.91176861290071,91.9730688074556));
#58769=CARTESIAN_POINT('Ctrl Pts',(3.8602224921159,6.90526136817879,91.9725340882551));
#58770=CARTESIAN_POINT('Ctrl Pts',(3.86510113403027,6.90253181632539,91.9723104090511));
#58771=CARTESIAN_POINT('Ctrl Pts',(3.87478876125025,6.89709819372525,91.9718663591969));
#58772=CARTESIAN_POINT('Ctrl Pts',(3.879597818738,6.89439425933837,91.9716459837322));
#58773=CARTESIAN_POINT('Ctrl Pts',(3.89090152200664,6.88802308176808,91.9711281218101));
#58774=CARTESIAN_POINT('Ctrl Pts',(3.89739382351398,6.8843516770843,91.9708307889606));
#58775=CARTESIAN_POINT('Ctrl Pts',(3.91649264885619,6.87351559159765,91.9699564018111));
#58776=CARTESIAN_POINT('Ctrl Pts',(3.92908470926034,6.86632540787878,91.9693802896286));
#58777=CARTESIAN_POINT('Ctrl Pts',(4.03575050220723,6.80502874669055,91.9645032485918));
#58778=CARTESIAN_POINT('Ctrl Pts',(4.12872354670779,6.74902521993854,91.9602732473172));
#58779=CARTESIAN_POINT('Ctrl Pts',(4.23101653106929,6.68450253966849,91.9556354516165));
#58780=CARTESIAN_POINT('Ctrl Pts',(4.24150009486671,6.67785534703741,91.9551603338924));
#58781=CARTESIAN_POINT('Ctrl Pts',(4.25929448415285,6.66651385509158,91.9543541897186));
#58782=CARTESIAN_POINT('Ctrl Pts',(4.26661328583846,6.66183214683053,91.9540227111495));
#58783=CARTESIAN_POINT('Ctrl Pts',(4.28141078327883,6.65233206115481,91.9533526798065));
#58784=CARTESIAN_POINT('Ctrl Pts',(4.28888909376237,6.6475131055954,91.9530141485019));
#58785=CARTESIAN_POINT('Ctrl Pts',(4.73030618450376,6.3620129802022,91.9330367479649));
#58786=CARTESIAN_POINT('Ctrl Pts',(5.13572487761194,6.03948529488066,91.9150848828523));
#58787=CARTESIAN_POINT('Ctrl Pts',(5.58580309405722,5.60310937385431,91.8936207349291));
#58788=CARTESIAN_POINT('Ctrl Pts',(5.66320286701521,5.52486779076524,91.8898618441282));
#58789=CARTESIAN_POINT('Ctrl Pts',(5.78497962464739,5.39651786250108,91.8837979753463));
#58790=CARTESIAN_POINT('Ctrl Pts',(5.83039679853534,5.34741689065184,91.8815012044588));
#58791=CARTESIAN_POINT('Ctrl Pts',(5.93820070393985,5.22786265966529,91.8759495718037));
#58792=CARTESIAN_POINT('Ctrl Pts',(5.99996322696375,5.1568611102235,91.8726856574339));
#58793=CARTESIAN_POINT('Ctrl Pts',(6.21340168416049,4.9024680155054,91.8610459156392));
#58794=CARTESIAN_POINT('Ctrl Pts',(6.35804763520046,4.71336089429345,91.8524927759235));
#58795=CARTESIAN_POINT('Ctrl Pts',(6.55149008387126,4.43531874509479,91.8396254038887));
#58796=CARTESIAN_POINT('Ctrl Pts',(6.60745030550028,4.35151394614097,91.835711093587));
#58797=CARTESIAN_POINT('Ctrl Pts',(6.67123673038275,4.25192052190159,91.8309895518037));
#58798=CARTESIAN_POINT('Ctrl Pts',(6.68063197414507,4.23714338370838,91.8302872203552));
#58799=CARTESIAN_POINT('Ctrl Pts',(6.69295003746793,4.21762632333132,91.829357108169));
#58800=CARTESIAN_POINT('Ctrl Pts',(6.69591708820335,4.21291423540735,91.8291323557244));
#58801=CARTESIAN_POINT('Ctrl Pts',(6.70076065163518,4.20520394274539,91.8287642783993));
#58802=CARTESIAN_POINT('Ctrl Pts',(6.70264013738476,4.2022075983015,91.82862115881));
#58803=CARTESIAN_POINT('Ctrl Pts',(6.70626469944769,4.19642057165022,91.8283445889791));
#58804=CARTESIAN_POINT('Ctrl Pts',(6.70801004464978,4.19363005928078,91.8282111574633));
#58805=CARTESIAN_POINT('Ctrl Pts',(6.71203957803949,4.18717856355431,91.8279025108358));
#58806=CARTESIAN_POINT('Ctrl Pts',(6.71432250580529,4.18351681103088,91.8277272092351));
#58807=CARTESIAN_POINT('Ctrl Pts',(6.72045992298259,4.17365460075944,91.8272547518482));
#58808=CARTESIAN_POINT('Ctrl Pts',(6.72430881778806,4.16745068658818,91.8269572112453));
#58809=CARTESIAN_POINT('Ctrl Pts',(6.75166185439961,4.12322462810395,91.8248337779397));
#58810=CARTESIAN_POINT('Ctrl Pts',(6.77485151406607,4.08500990672952,91.8229866366889));
#58811=CARTESIAN_POINT('Ctrl Pts',(7.1739823285814,3.41452683702469,91.7903935004589));
#58812=CARTESIAN_POINT('Ctrl Pts',(7.46024472898376,2.73308460483765,91.7547431644953));
#58813=CARTESIAN_POINT('Ctrl Pts',(7.7341648173293,1.69694305319584,91.705450632146));
#58814=CARTESIAN_POINT('Ctrl Pts',(7.79928497369899,1.36678738881675,91.6903604151424));
#58815=CARTESIAN_POINT('Ctrl Pts',(7.86861384634824,0.840634469668327,91.6675578410158));
#58816=CARTESIAN_POINT('Ctrl Pts',(7.88690344147466,0.64692473099016,91.6594195857258));
#58817=CARTESIAN_POINT('Ctrl Pts',(7.89931258540803,0.430441597255867,91.6506034591018));
#58818=CARTESIAN_POINT('Ctrl Pts',(7.900495719312,0.408150328583057,91.6496989164236));
#58819=CARTESIAN_POINT('Ctrl Pts',(7.90239526889608,0.369251048749467,91.648126065074));
#58820=CARTESIAN_POINT('Ctrl Pts',(7.90315371397624,0.352645290101455,91.647456413518));
#58821=CARTESIAN_POINT('Ctrl Pts',(7.90419787802373,0.328085728384394,91.6464686287293));
#58822=CARTESIAN_POINT('Ctrl Pts',(7.90452394071199,0.320133739749633,91.6461492053482));
#58823=CARTESIAN_POINT('Ctrl Pts',(7.9050756390237,0.306164016452225,91.6455887643589));
#58824=CARTESIAN_POINT('Ctrl Pts',(7.90530640416391,0.300146497812528,91.6453475829545));
#58825=CARTESIAN_POINT('Ctrl Pts',(7.90573816802365,0.288541638690467,91.6448829054079));
#58826=CARTESIAN_POINT('Ctrl Pts',(7.90594011493599,0.282954338737594,91.6446593791277));
#58827=CARTESIAN_POINT('Ctrl Pts',(7.90640368717738,0.269740554815243,91.6441312141144));
#58828=CARTESIAN_POINT('Ctrl Pts',(7.90666020140344,0.262113890338347,91.6438267387128));
#58829=CARTESIAN_POINT('Ctrl Pts',(7.90751703773239,0.235491988386449,91.6427652049478));
#58830=CARTESIAN_POINT('Ctrl Pts',(7.90805994820152,0.216494897966537,91.6420099786938));
#58831=CARTESIAN_POINT('Ctrl Pts',(7.91368255097154,-0.00865679662528287,
91.633085678986));
#58832=CARTESIAN_POINT('Ctrl Pts',(7.91076830002816,-0.214939291528602,
91.6251763070342));
#58833=CARTESIAN_POINT('Ctrl Pts',(7.87282463497009,-0.927126694883613,
91.5985888920336));
#58834=CARTESIAN_POINT('Ctrl Pts',(7.79725179328093,-1.4296240408593,91.5811707702051));
#58835=CARTESIAN_POINT('Ctrl Pts',(7.59019735496319,-2.25658963339416,91.5518199338051));
#58836=CARTESIAN_POINT('Ctrl Pts',(7.48441898664359,-2.58587376219204,91.5399085395635));
#58837=CARTESIAN_POINT('Ctrl Pts',(7.3298239755355,-2.97712254262954,91.5244786569774));
#58838=CARTESIAN_POINT('Ctrl Pts',(7.30118833010489,-3.04667469000373,91.5216841877781));
#58839=CARTESIAN_POINT('Ctrl Pts',(7.22497729860908,-3.22453346722947,91.5143811006636));
#58840=CARTESIAN_POINT('Ctrl Pts',(7.1759572205056,-3.33219915739021,91.5098057939485));
#58841=CARTESIAN_POINT('Ctrl Pts',(7.11488044280174,-3.45874125915353,91.5042094169378));
#58842=CARTESIAN_POINT('Ctrl Pts',(7.10513688919724,-3.47871306425574,91.503319889227));
#58843=CARTESIAN_POINT('Ctrl Pts',(7.09209717134167,-3.50515783790371,91.5021339741567));
#58844=CARTESIAN_POINT('Ctrl Pts',(7.08887598570677,-3.51166783951926,91.5018413808267));
#58845=CARTESIAN_POINT('Ctrl Pts',(7.08357099117738,-3.52235216584513,91.5013601097756));
#58846=CARTESIAN_POINT('Ctrl Pts',(7.08149244213387,-3.52652910935761,91.501171694133));
#58847=CARTESIAN_POINT('Ctrl Pts',(7.07745693809509,-3.53462069302065,91.500806180636));
#58848=CARTESIAN_POINT('Ctrl Pts',(7.075500426787,-3.538535553664,91.5006291046928));
#58849=CARTESIAN_POINT('Ctrl Pts',(7.07097514305463,-3.547571613319,91.5002198515517));
#58850=CARTESIAN_POINT('Ctrl Pts',(7.06840405592205,-3.55269164540033,91.4999875613087));
#58851=CARTESIAN_POINT('Ctrl Pts',(7.06036317761945,-3.56866087264581,91.499261820975));
#58852=CARTESIAN_POINT('Ctrl Pts',(7.05487396970901,-3.57950022950289,91.4987674343322));
#58853=CARTESIAN_POINT('Ctrl Pts',(7.00760921971471,-3.67230131523403,91.4945197303969));
#58854=CARTESIAN_POINT('Ctrl Pts',(6.96443297884162,-3.75353917035897,91.4907008136383));
#58855=CARTESIAN_POINT('Ctrl Pts',(6.60878412099147,-4.39543667205015,91.459816050411));
#58856=CARTESIAN_POINT('Ctrl Pts',(6.23055008895123,-4.91692655628546,91.4305803681068));
#58857=CARTESIAN_POINT('Ctrl Pts',(5.51647024023934,-5.68488768762701,91.3847582652302));
#58858=CARTESIAN_POINT('Ctrl Pts',(5.21689485469562,-5.96099344088897,91.3674743386727));
#58859=CARTESIAN_POINT('Ctrl Pts',(4.84815191393325,-6.25166177674386,91.3483116490339));
#58860=CARTESIAN_POINT('Ctrl Pts',(4.79845288858413,-6.28988886905801,91.3457685847753));
#58861=CARTESIAN_POINT('Ctrl Pts',(4.73444271552863,-6.33792343860169,91.342542078425));
#58862=CARTESIAN_POINT('Ctrl Pts',(4.72054707528075,-6.34827981846333,91.3418445486037));
#58863=CARTESIAN_POINT('Ctrl Pts',(4.69819923135228,-6.36482165318867,91.3407273299827));
#58864=CARTESIAN_POINT('Ctrl Pts',(4.68976860495549,-6.37103611095264,91.3403069071088));
#58865=CARTESIAN_POINT('Ctrl Pts',(4.67393470523936,-6.38265927594394,91.3395192356602));
#58866=CARTESIAN_POINT('Ctrl Pts',(4.66653432099559,-6.38807189166788,91.339151888711));
#58867=CARTESIAN_POINT('Ctrl Pts',(4.64997430251653,-6.40013969970884,91.3383316309322));
#58868=CARTESIAN_POINT('Ctrl Pts',(4.64080974879188,-6.40678812403415,91.3378788904879));
#58869=CARTESIAN_POINT('Ctrl Pts',(4.61444776255602,-6.42582618029135,91.3365800169426));
#58870=CARTESIAN_POINT('Ctrl Pts',(4.59721472988969,-6.43816643042406,91.3357351266424));
#58871=CARTESIAN_POINT('Ctrl Pts',(4.49652401020729,-6.50965874207843,91.330822795498));
#58872=CARTESIAN_POINT('Ctrl Pts',(4.41197376671182,-6.56725766600531,91.3267948257203));
#58873=CARTESIAN_POINT('Ctrl Pts',(3.77404644271607,-6.98395695642861,91.2970933059629));
#58874=CARTESIAN_POINT('Ctrl Pts',(3.1788284885799,-7.27421179263632,91.2734690803399));
#58875=CARTESIAN_POINT('Ctrl Pts',(2.23527777216359,-7.59613087496458,91.2373270311647));
#58876=CARTESIAN_POINT('Ctrl Pts',(1.909453578009,-7.68450614308912,91.2250007442387));
#58877=CARTESIAN_POINT('Ctrl Pts',(1.48294763486537,-7.77138322814377,91.2081570835866));
#58878=CARTESIAN_POINT('Ctrl Pts',(1.38653695802092,-7.78916203181984,91.2043028896633));
#58879=CARTESIAN_POINT('Ctrl Pts',(1.27869868732133,-7.80698263169832,91.1999184965402));
#58880=CARTESIAN_POINT('Ctrl Pts',(1.2675698495,-7.80879727098547,91.1994651616009));
#58881=CARTESIAN_POINT('Ctrl Pts',(1.25097549686911,-7.81146669380853,91.1987878495902));
#58882=CARTESIAN_POINT('Ctrl Pts',(1.24551287279229,-7.81233955263828,91.1985646720871));
#58883=CARTESIAN_POINT('Ctrl Pts',(1.23616721465634,-7.81382282036077,91.1981824762726));
#58884=CARTESIAN_POINT('Ctrl Pts',(1.23228462708304,-7.81443606720079,91.1980235848994));
#58885=CARTESIAN_POINT('Ctrl Pts',(1.22433433591922,-7.81568572712306,91.1976979969782));
#58886=CARTESIAN_POINT('Ctrl Pts',(1.22026658941661,-7.81632185890083,91.1975312877873));
#58887=CARTESIAN_POINT('Ctrl Pts',(1.21054963936562,-7.81783366739128,91.1971327591652));
#58888=CARTESIAN_POINT('Ctrl Pts',(1.2048999854946,-7.81870639588479,91.1969008058573));
#58889=CARTESIAN_POINT('Ctrl Pts',(1.18466586919018,-7.82180960265599,91.1960691975298));
#58890=CARTESIAN_POINT('Ctrl Pts',(1.17007618469181,-7.82400539361137,91.1954679488935));
#58891=CARTESIAN_POINT('Ctrl Pts',(0.950260351221596,-7.85645973934033,
91.1863837841669));
#58892=CARTESIAN_POINT('Ctrl Pts',(0.743962456177103,-7.87867050852365,
91.1774839310529));
#58893=CARTESIAN_POINT('Ctrl Pts',(-0.0211807592265673,-7.93073417279431,
91.1435842264521));
#58894=CARTESIAN_POINT('Ctrl Pts',(-0.581868266284063,-7.90938929797473,
91.1171747745959));
#58895=CARTESIAN_POINT('Ctrl Pts',(-1.42690149520752,-7.78681611606584,
91.0784354972897));
#58896=CARTESIAN_POINT('Ctrl Pts',(-1.71561666175553,-7.7283396430826,91.0653695573615));
#58897=CARTESIAN_POINT('Ctrl Pts',(-2.17775769513064,-7.60755477159421,
91.0449413266898));
#58898=CARTESIAN_POINT('Ctrl Pts',(-2.35343855390713,-7.55505467615469,
91.0372903870975));
#58899=CARTESIAN_POINT('Ctrl Pts',(-2.55782757103749,-7.48615305007275,
91.0285260113585));
#58900=CARTESIAN_POINT('Ctrl Pts',(-2.58844609119514,-7.47562146168603,
91.0272166719071));
#58901=CARTESIAN_POINT('Ctrl Pts',(-2.62861482409304,-7.4615285930385,91.0255035929168));
#58902=CARTESIAN_POINT('Ctrl Pts',(-2.63822380687272,-7.45813649540232,
91.0250941492467));
#58903=CARTESIAN_POINT('Ctrl Pts',(-2.65390254353873,-7.45256760243809,
91.0244266397378));
#58904=CARTESIAN_POINT('Ctrl Pts',(-2.65997622278917,-7.4504019404303,91.024168197514));
#58905=CARTESIAN_POINT('Ctrl Pts',(-2.67167846343614,-7.44621319607253,
91.0236705213851));
#58906=CARTESIAN_POINT('Ctrl Pts',(-2.67730739033785,-7.44419115224769,
91.023431252509));
#58907=CARTESIAN_POINT('Ctrl Pts',(-2.6902092902807,-7.43953995774249,91.0228831043623));
#58908=CARTESIAN_POINT('Ctrl Pts',(-2.69748071736787,-7.43690652006835,
91.0225743708268));
#58909=CARTESIAN_POINT('Ctrl Pts',(-2.72039117645356,-7.42857119082878,
91.0216022519872));
#58910=CARTESIAN_POINT('Ctrl Pts',(-2.73601612791031,-7.42283058154975,
91.0209401834845));
#58911=CARTESIAN_POINT('Ctrl Pts',(-2.86293482521028,-7.37574544205321,
91.0155696615044));
#58912=CARTESIAN_POINT('Ctrl Pts',(-2.97330574376928,-7.33194865922051,
91.0109456749634));
#58913=CARTESIAN_POINT('Ctrl Pts',(-3.89287881950393,-6.94286721201783,
90.9727458628391));
#58914=CARTESIAN_POINT('Ctrl Pts',(-4.64012222742711,-6.4673785988233,90.9447268046663));
#58915=CARTESIAN_POINT('Ctrl Pts',(-5.53760730902066,-5.65919302882644,
90.9023808821957));
#58916=CARTESIAN_POINT('Ctrl Pts',(-5.76749474851314,-5.42471420250105,
90.8904188083037));
#58917=CARTESIAN_POINT('Ctrl Pts',(-5.99121335698095,-5.16618580200786,
90.8767360084477));
#58918=CARTESIAN_POINT('Ctrl Pts',(-6.00025827479084,-5.15567782749045,
90.8761790589719));
#58919=CARTESIAN_POINT('Ctrl Pts',(-6.01257076010891,-5.14129745554785,
90.8754156805187));
#58920=CARTESIAN_POINT('Ctrl Pts',(-6.01586234700275,-5.13744556111512,
90.8752110883139));
#58921=CARTESIAN_POINT('Ctrl Pts',(-6.02136729150627,-5.13099099723098,
90.8748680582291));
#58922=CARTESIAN_POINT('Ctrl Pts',(-6.02358266247359,-5.12839005743327,
90.874729776476));
#58923=CARTESIAN_POINT('Ctrl Pts',(-6.02794872438443,-5.12325738288254,
90.8744567857774));
#58924=CARTESIAN_POINT('Ctrl Pts',(-6.030099496285,-5.12072573957135,90.8743220848618));
#58925=CARTESIAN_POINT('Ctrl Pts',(-6.03482393522903,-5.1151575650319,90.8740257094361));
#58926=CARTESIAN_POINT('Ctrl Pts',(-6.03739690486433,-5.11212044628599,
90.8738639818439));
#58927=CARTESIAN_POINT('Ctrl Pts',(-6.04630310439021,-5.10159151706491,
90.8733030683934));
#58928=CARTESIAN_POINT('Ctrl Pts',(-6.05262466763104,-5.09408989597374,
90.8729030021323));
#58929=CARTESIAN_POINT('Ctrl Pts',(-6.1123303586295,-5.02297079831646,90.8691063050673));
#58930=CARTESIAN_POINT('Ctrl Pts',(-6.16472182029456,-4.95853022560046,
90.8656369133556));
#58931=CARTESIAN_POINT('Ctrl Pts',(-6.66168682937597,-4.32721984900792,
90.8314772691184));
#58932=CARTESIAN_POINT('Ctrl Pts',(-7.02787940775434,-3.7029553723878,90.7967384002758));
#58933=CARTESIAN_POINT('Ctrl Pts',(-7.42290222059974,-2.75308620273604,
90.7501273254391));
#58934=CARTESIAN_POINT('Ctrl Pts',(-7.52454740478917,-2.46174201257003,
90.736525971094));
#58935=CARTESIAN_POINT('Ctrl Pts',(-7.63927991404165,-2.05854710626559,
90.7187897070337));
#58936=CARTESIAN_POINT('Ctrl Pts',(-7.66738063817991,-1.95127888799704,
90.7141707675575));
#58937=CARTESIAN_POINT('Ctrl Pts',(-7.70707720114953,-1.78561454275931,
90.7071886383224));
#58938=CARTESIAN_POINT('Ctrl Pts',(-7.72028382263607,-1.7276215402261,90.7047725877386));
#58939=CARTESIAN_POINT('Ctrl Pts',(-7.73547006985905,-1.65728080406908,
90.7018754753632));
#58940=CARTESIAN_POINT('Ctrl Pts',(-7.73807585209953,-1.64507111526698,
90.7013738077295));
#58941=CARTESIAN_POINT('Ctrl Pts',(-7.74208200362152,-1.62607970295307,
90.7005953669043));
#58942=CARTESIAN_POINT('Ctrl Pts',(-7.74350238436165,-1.61930224938565,
90.7003179354531));
#58943=CARTESIAN_POINT('Ctrl Pts',(-7.74598940520069,-1.6073571403591,90.6998296190175));
#58944=CARTESIAN_POINT('Ctrl Pts',(-7.74705977629082,-1.60219027111887,
90.6996186114533));
#58945=CARTESIAN_POINT('Ctrl Pts',(-7.74931261494286,-1.591260382961,90.6991727023025));
#58946=CARTESIAN_POINT('Ctrl Pts',(-7.75049382527249,-1.58549710662088,
90.6989378421424));
#58947=CARTESIAN_POINT('Ctrl Pts',(-7.75381292697297,-1.56921044017725,
90.6982748897011));
#58948=CARTESIAN_POINT('Ctrl Pts',(-7.7559358260403,-1.55868398836987,90.6978472899915));
#58949=CARTESIAN_POINT('Ctrl Pts',(-7.7646665462295,-1.51493298752023,90.6960737040128));
#58950=CARTESIAN_POINT('Ctrl Pts',(-7.77108240959782,-1.48167025729222,
90.6947340180458));
#58951=CARTESIAN_POINT('Ctrl Pts',(-7.86620710105452,-0.970880000486219,
90.6742925969767));
#58952=CARTESIAN_POINT('Ctrl Pts',(-7.91097364017281,-0.486193375633732,
90.6567465537409));
#58953=CARTESIAN_POINT('Ctrl Pts',(-7.91103644331997,0.671667830417302,
90.6165305979411));
#58954=CARTESIAN_POINT('Ctrl Pts',(-7.82542677478422,1.34093832443821,90.5947062374235));
#58955=CARTESIAN_POINT('Ctrl Pts',(-7.6528318959326,2.00456340857716,90.5684468110225));
#58956=CARTESIAN_POINT('Ctrl Pts',(-7.64933231993946,2.01787649323009,90.5679179769197));
#58957=CARTESIAN_POINT('Ctrl Pts',(-7.62554163487146,2.10742973079592,90.5643465180999));
#58958=CARTESIAN_POINT('Ctrl Pts',(-7.60414636988768,2.18336953185054,90.5612489019157));
#58959=CARTESIAN_POINT('Ctrl Pts',(-7.57884936431733,2.26827190472345,90.5576949780685));
#58960=CARTESIAN_POINT('Ctrl Pts',(-7.57606200183496,2.27756441479243,90.5573047761293));
#58961=CARTESIAN_POINT('Ctrl Pts',(-7.57198488142962,2.29106641952895,90.5567359970455));
#58962=CARTESIAN_POINT('Ctrl Pts',(-7.57070868308965,2.2952800306039,90.5565582389325));
#58963=CARTESIAN_POINT('Ctrl Pts',(-7.56844176523037,2.30274223073878,90.5562429803134));
#58964=CARTESIAN_POINT('Ctrl Pts',(-7.56745246818332,2.30599125684134,90.5561055650138));
#58965=CARTESIAN_POINT('Ctrl Pts',(-7.56539486989071,2.31273318917736,90.5558201049253));
#58966=CARTESIAN_POINT('Ctrl Pts',(-7.56432624142065,2.31622599393089,90.5556720406734));
#58967=CARTESIAN_POINT('Ctrl Pts',(-7.56156834578994,2.32521789208126,90.5552904136801));
#58968=CARTESIAN_POINT('Ctrl Pts',(-7.5598755011901,2.33071587712521,90.555056639499));
#58969=CARTESIAN_POINT('Ctrl Pts',(-7.55282868431633,2.35351393095204,90.5540854848258));
#58970=CARTESIAN_POINT('Ctrl Pts',(-7.54742134946775,2.37079731763974,90.5533449858794));
#58971=CARTESIAN_POINT('Ctrl Pts',(-7.51043400788925,2.4876103962893,90.5483120952514));
#58972=CARTESIAN_POINT('Ctrl Pts',(-7.4769466009413,2.58652126773107,90.543912421778));
#58973=CARTESIAN_POINT('Ctrl Pts',(-7.36003421414467,2.91057731419382,90.529109004484));
#58974=CARTESIAN_POINT('Ctrl Pts',(-7.26832105776938,3.13258042113028,90.5183425129204));
#58975=CARTESIAN_POINT('Ctrl Pts',(-6.79495912436123,4.1452277344965,90.4673535755859));
#58976=CARTESIAN_POINT('Ctrl Pts',(-6.29336779692856,4.8732506367016,90.4260997860459));
#58977=CARTESIAN_POINT('Ctrl Pts',(-5.65041374680111,5.53704437451131,90.388229622283));
#58978=CARTESIAN_POINT('Ctrl Pts',(-5.61813006991555,5.56979806867234,90.386357475511));
#58979=CARTESIAN_POINT('Ctrl Pts',(-5.57126581387673,5.61652257099746,90.3836813445754));
#58980=CARTESIAN_POINT('Ctrl Pts',(-5.55691479424308,5.63072167103939,90.3828673601251));
#58981=CARTESIAN_POINT('Ctrl Pts',(-5.53682053933631,5.65045156433449,90.3817352489327));
#58982=CARTESIAN_POINT('Ctrl Pts',(-5.53112311775544,5.65602878549963,90.3814151055096));
#58983=CARTESIAN_POINT('Ctrl Pts',(-5.52127040598132,5.66564450698911,90.3808629342966));
#58984=CARTESIAN_POINT('Ctrl Pts',(-5.51711909687641,5.66968706778568,90.3806307307921));
#58985=CARTESIAN_POINT('Ctrl Pts',(-5.5085189140592,5.67804356938654,90.380150601091));
#58986=CARTESIAN_POINT('Ctrl Pts',(-5.5040694045107,5.68235685195471,90.3799027033462));
#58987=CARTESIAN_POINT('Ctrl Pts',(-5.49366228086857,5.69242165661466,90.3793240713696));
#58988=CARTESIAN_POINT('Ctrl Pts',(-5.48770069019601,5.69816906631303,90.3789935141765));
#58989=CARTESIAN_POINT('Ctrl Pts',(-5.46852761298895,5.71659531902221,90.3779333033456));
#58990=CARTESIAN_POINT('Ctrl Pts',(-5.45528108309509,5.72923769847399,90.3772052126631));
#58991=CARTESIAN_POINT('Ctrl Pts',(-5.18302412786111,5.98727717112551,90.3623300416581));
#58992=CARTESIAN_POINT('Ctrl Pts',(-4.90773989433601,6.21492951175404,90.3489674283416));
#58993=CARTESIAN_POINT('Ctrl Pts',(-4.47543237032722,6.52573822362952,90.3297955900048));
#58994=CARTESIAN_POINT('Ctrl Pts',(-4.32948553160389,6.6234667292334,90.3235975338785));
#58995=CARTESIAN_POINT('Ctrl Pts',(-3.60488375268019,7.07448101063024,90.2937785234339));
#58996=CARTESIAN_POINT('Ctrl Pts',(-2.98578643850993,7.35719428982956,90.2713672781674));
#58997=CARTESIAN_POINT('Ctrl Pts',(-2.29962520076352,7.56949719673342,90.2430819346046));
#58998=CARTESIAN_POINT('Ctrl Pts',(-2.26081300272504,7.58117987766749,90.2414702183407));
#58999=CARTESIAN_POINT('Ctrl Pts',(-2.21484979615396,7.594630705138,90.2395458848578));
#59000=CARTESIAN_POINT('Ctrl Pts',(-2.20778336582223,7.59668794777799,90.2392495997125));
#59001=CARTESIAN_POINT('Ctrl Pts',(-2.19642239885298,7.59997826374602,90.2387725357218));
#59002=CARTESIAN_POINT('Ctrl Pts',(-2.19212965862894,7.60121756846702,90.2385921131943));
#59003=CARTESIAN_POINT('Ctrl Pts',(-2.18450183122812,7.6034127065301,90.2382712232249));
#59004=CARTESIAN_POINT('Ctrl Pts',(-2.18116715752563,7.60436998490964,90.2381308389686));
#59005=CARTESIAN_POINT('Ctrl Pts',(-2.17418665322266,7.60636889547045,90.2378367603777));
#59006=CARTESIAN_POINT('Ctrl Pts',(-2.17054071202144,7.60741009768743,90.2376830420841));
#59007=CARTESIAN_POINT('Ctrl Pts',(-2.16099352404171,7.6101291466699,90.2372802069598));
#59008=CARTESIAN_POINT('Ctrl Pts',(-2.15509108091983,7.6118027478709,90.2370308471644));
#59009=CARTESIAN_POINT('Ctrl Pts',(-2.12923451257058,7.61910173203166,90.2359371435879));
#59010=CARTESIAN_POINT('Ctrl Pts',(-2.10926041968613,7.6246554859746,90.2350887579614));
#59011=CARTESIAN_POINT('Ctrl Pts',(-1.57481904687058,7.77099499934802,90.2122996744269));
#59012=CARTESIAN_POINT('Ctrl Pts',(-1.04748248265556,7.85946030993799,90.1876925563904));
#59013=CARTESIAN_POINT('Ctrl Pts',(0.148146788967754,7.93750737468365,90.1326662581752));
#59014=CARTESIAN_POINT('Ctrl Pts',(0.814522869031433,7.89701169705485,90.1027043333793));
#59015=CARTESIAN_POINT('Ctrl Pts',(1.51261333030705,7.76517735044155,90.0737061813983));
#59016=CARTESIAN_POINT('Ctrl Pts',(1.55711100278836,7.75637697540344,90.0718668227398));
#59017=CARTESIAN_POINT('Ctrl Pts',(1.61345217296389,7.74472990314489,90.0695491240123));
#59018=CARTESIAN_POINT('Ctrl Pts',(1.625367656162,7.74223799499316,90.0690595964059));
#59019=CARTESIAN_POINT('Ctrl Pts',(1.64422009331379,7.73824990828686,90.0682860779094));
#59020=CARTESIAN_POINT('Ctrl Pts',(1.65116084421602,7.73677188659604,90.0680015130439));
#59021=CARTESIAN_POINT('Ctrl Pts',(1.66405926572821,7.73400704096028,90.067473086985));
#59022=CARTESIAN_POINT('Ctrl Pts',(1.67001745296989,7.73272266775862,90.0672291484178));
#59023=CARTESIAN_POINT('Ctrl Pts',(1.68319129851719,7.72986691912171,90.066690136323));
#59024=CARTESIAN_POINT('Ctrl Pts',(1.69040625678016,7.72829232250906,90.0663951651149));
#59025=CARTESIAN_POINT('Ctrl Pts',(1.71112168067951,7.72374097940484,90.0655489106209));
#59026=CARTESIAN_POINT('Ctrl Pts',(1.72461659252415,7.72073893706344,90.0649984301003));
#59027=CARTESIAN_POINT('Ctrl Pts',(1.81282493550354,7.70087353558119,90.0614054728505));
#59028=CARTESIAN_POINT('Ctrl Pts',(1.88729914355363,7.68296100537467,90.0583964758123));
#59029=CARTESIAN_POINT('Ctrl Pts',(2.1036882192955,7.62757876659699,90.0497195371574));
#59030=CARTESIAN_POINT('Ctrl Pts',(2.24483704377802,7.5872373904524,90.0441434662331));
#59031=CARTESIAN_POINT('Ctrl Pts',(2.709041785495,7.44047476456881,90.0260133967217));
#59032=CARTESIAN_POINT('Ctrl Pts',(3.02636012445742,7.31715346808188,90.0139775561131));
#59033=CARTESIAN_POINT('Ctrl Pts',(3.95750835273183,6.88430489162142,89.9783720468342));
#59034=CARTESIAN_POINT('Ctrl Pts',(4.53981523142303,6.51500952788348,89.9558549705293));
#59035=CARTESIAN_POINT('Ctrl Pts',(5.08029683888361,6.06422315401861,89.9281702659051));
#59036=CARTESIAN_POINT('Ctrl Pts',(5.09350488234076,6.0531336048777,89.9274889880731));
#59037=CARTESIAN_POINT('Ctrl Pts',(5.1268794965567,6.02492550689082,89.9257551925243));
#59038=CARTESIAN_POINT('Ctrl Pts',(5.14699653313801,6.00774894559352,89.9246986555212));
#59039=CARTESIAN_POINT('Ctrl Pts',(5.17216789066655,5.98603762141822,89.9233616716148));
#59040=CARTESIAN_POINT('Ctrl Pts',(5.17730323096243,5.98159663872512,89.9230881169896));
#59041=CARTESIAN_POINT('Ctrl Pts',(5.18536047374489,5.97461067951697,89.922657662781));
#59042=CARTESIAN_POINT('Ctrl Pts',(5.18828624408523,5.97207014893574,89.9225010948829));
#59043=CARTESIAN_POINT('Ctrl Pts',(5.19368778464296,5.96737287059228,89.9222115569459));
#59044=CARTESIAN_POINT('Ctrl Pts',(5.19616408253067,5.96521672769655,89.9220786324132));
#59045=CARTESIAN_POINT('Ctrl Pts',(5.2010317354334,5.96097307185073,89.9218169715996));
#59046=CARTESIAN_POINT('Ctrl Pts',(5.20342317775739,5.95888566004011,89.921688242974));
#59047=CARTESIAN_POINT('Ctrl Pts',(5.21047258017884,5.95272498770904,89.9213082584521));
#59048=CARTESIAN_POINT('Ctrl Pts',(5.21512697752014,5.94864773673067,89.9210566961871));
#59049=CARTESIAN_POINT('Ctrl Pts',(5.23713000864485,5.9293274153709,89.9198642763862));
#59050=CARTESIAN_POINT('Ctrl Pts',(5.25441645215651,5.91401403888302,89.9189180665562));
#59051=CARTESIAN_POINT('Ctrl Pts',(5.38941391052038,5.79336603334328,89.9114566265191));
#59052=CARTESIAN_POINT('Ctrl Pts',(5.50400698401703,5.68460849406302,89.9046916062721));
#59053=CARTESIAN_POINT('Ctrl Pts',(5.69000864861778,5.49717955558866,89.8930946582375));
#59054=CARTESIAN_POINT('Ctrl Pts',(5.76323128031356,5.42036396287902,89.8883578464256));
#59055=CARTESIAN_POINT('Ctrl Pts',(6.47142951840073,4.64683778879506,89.8410212693392));
#59056=CARTESIAN_POINT('Ctrl Pts',(6.97883726939091,3.84307474239805,89.7959439565106));
#59057=CARTESIAN_POINT('Ctrl Pts',(7.35418555031589,2.91601272883977,89.7549702798263));
#59058=CARTESIAN_POINT('Ctrl Pts',(7.37502215974999,2.86290476091524,89.7526530690141));
#59059=CARTESIAN_POINT('Ctrl Pts',(7.39945926455861,2.79858212039492,89.7498820806442));
#59060=CARTESIAN_POINT('Ctrl Pts',(7.40361122110666,2.78757962769762,89.7494093447176));
#59061=CARTESIAN_POINT('Ctrl Pts',(7.41036068272521,2.7695724153076,89.74863767024));
#59062=CARTESIAN_POINT('Ctrl Pts',(7.41297281858815,2.76257322129083,89.7483382294199));
#59063=CARTESIAN_POINT('Ctrl Pts',(7.41762611777935,2.75005062695556,89.7478033768049));
#59064=CARTESIAN_POINT('Ctrl Pts',(7.41967103429557,2.74452863293776,89.7475678363881));
#59065=CARTESIAN_POINT('Ctrl Pts',(7.42398130900293,2.732849349572,89.7470703096822));
#59066=CARTESIAN_POINT('Ctrl Pts',(7.42624517751905,2.7266915130852,89.7468083745672));
#59067=CARTESIAN_POINT('Ctrl Pts',(7.43223113291634,2.71034665971032,89.7461141287476));
#59068=CARTESIAN_POINT('Ctrl Pts',(7.43593994162164,2.70015477606857,89.7456822727326));
#59069=CARTESIAN_POINT('Ctrl Pts',(7.45286779620974,2.65333729223237,89.7437032596434));
#59070=CARTESIAN_POINT('Ctrl Pts',(7.46583739013405,2.61662173320734,89.7421646307633));
#59071=CARTESIAN_POINT('Ctrl Pts',(7.55892542484002,2.34677172473099,89.7309519969572));
#59072=CARTESIAN_POINT('Ctrl Pts',(7.62838192035115,2.11009305165641,89.7216470141069));
#59073=CARTESIAN_POINT('Ctrl Pts',(7.76931143190361,1.53096737910977,89.6998740487694));
#59074=CARTESIAN_POINT('Ctrl Pts',(7.82935615194035,1.18627942710046,89.6877435992011));
#59075=CARTESIAN_POINT('Ctrl Pts',(7.93160570893311,0.227298638090453,89.6546725653809));
#59076=CARTESIAN_POINT('Ctrl Pts',(7.92528001307849,-0.389579946987129,
89.6342296068678));
#59077=CARTESIAN_POINT('Ctrl Pts',(7.84278711280587,-1.0373398129147,89.6084952837222));
#59078=CARTESIAN_POINT('Ctrl Pts',(7.83768079455049,-1.07524102109694,89.6069733389227));
#59079=CARTESIAN_POINT('Ctrl Pts',(7.83123335987005,-1.12060810542224,89.6051305920217));
#59080=CARTESIAN_POINT('Ctrl Pts',(7.83015598830162,-1.12811154624582,89.6048251233334));
#59081=CARTESIAN_POINT('Ctrl Pts',(7.82849628823628,-1.13955373632641,89.6043582387046));
#59082=CARTESIAN_POINT('Ctrl Pts',(7.82792176550284,-1.14349363179619,89.6041972829286));
#59083=CARTESIAN_POINT('Ctrl Pts',(7.82688350789978,-1.15057622319718,89.6039075892593));
#59084=CARTESIAN_POINT('Ctrl Pts',(7.82642085360621,-1.15371907923898,89.6037789155641));
#59085=CARTESIAN_POINT('Ctrl Pts',(7.82551114225162,-1.15987310924376,89.603526715274));
#59086=CARTESIAN_POINT('Ctrl Pts',(7.82506424104106,-1.16288429799642,89.6034031980997));
#59087=CARTESIAN_POINT('Ctrl Pts',(7.82380430391604,-1.17134005241748,89.603056027072));
#59088=CARTESIAN_POINT('Ctrl Pts',(7.8229873241902,-1.17678401995889,89.6028321384201));
#59089=CARTESIAN_POINT('Ctrl Pts',(7.81959827355985,-1.1992075557689,89.6019084213369));
#59090=CARTESIAN_POINT('Ctrl Pts',(7.81697661659254,-1.2161794638618,89.601205672199));
#59091=CARTESIAN_POINT('Ctrl Pts',(7.79905205139171,-1.32976562046447,89.5964789331431));
#59092=CARTESIAN_POINT('Ctrl Pts',(7.78201416038242,-1.42609382709904,89.592356371783));
#59093=CARTESIAN_POINT('Ctrl Pts',(7.71980619048592,-1.74337901838519,89.5784572399857));
#59094=CARTESIAN_POINT('Ctrl Pts',(7.66697650549332,-1.96271165599338,89.5683341494993));
#59095=CARTESIAN_POINT('Ctrl Pts',(7.38383394785498,-2.95068333325408,89.5212675758226));
#59096=CARTESIAN_POINT('Ctrl Pts',(7.04671261031696,-3.68399408740623,89.4828137421131));
#59097=CARTESIAN_POINT('Ctrl Pts',(6.499159546993,-4.51462525144733,89.4403110165798));
#59098=CARTESIAN_POINT('Ctrl Pts',(6.38747391051129,-4.67130603880937,89.4323109147705));
#59099=CARTESIAN_POINT('Ctrl Pts',(6.25879149078323,-4.83857407053081,89.4237802753773));
#59100=CARTESIAN_POINT('Ctrl Pts',(6.24734851250089,-4.85333972959324,89.4230272956891));
#59101=CARTESIAN_POINT('Ctrl Pts',(6.23119189570707,-4.8740358986809,89.4219719498613));
#59102=CARTESIAN_POINT('Ctrl Pts',(6.22652192100375,-4.88000032278956,89.4216678172619));
#59103=CARTESIAN_POINT('Ctrl Pts',(6.21839918837262,-4.89034391759876,89.4211403957451));
#59104=CARTESIAN_POINT('Ctrl Pts',(6.21495035732997,-4.89472615724815,89.4209169477376));
#59105=CARTESIAN_POINT('Ctrl Pts',(6.20776145957406,-4.90384084621998,89.4204521997571));
#59106=CARTESIAN_POINT('Ctrl Pts',(6.20402060733639,-4.90857267319028,89.4202109319286));
#59107=CARTESIAN_POINT('Ctrl Pts',(6.1951942981292,-4.91971091754983,89.4196430163892));
#59108=CARTESIAN_POINT('Ctrl Pts',(6.19010430556414,-4.92611374113469,89.4193165535764));
#59109=CARTESIAN_POINT('Ctrl Pts',(6.17341553080725,-4.9470402415968,89.4182495719807));
#59110=CARTESIAN_POINT('Ctrl Pts',(6.16177545252874,-4.96153098818865,89.4175107382099));
#59111=CARTESIAN_POINT('Ctrl Pts',(5.98032873670946,-5.18579082547538,89.4060761734248));
#59112=CARTESIAN_POINT('Ctrl Pts',(5.79994125966426,-5.38678528454571,89.3958324919353));
#59113=CARTESIAN_POINT('Ctrl Pts',(5.53659318569436,-5.65161775271878,89.3821427094179));
#59114=CARTESIAN_POINT('Ctrl Pts',(5.46212947239637,-5.72361683266199,89.3783982600544));
#59115=CARTESIAN_POINT('Ctrl Pts',(5.06745547971587,-6.09050884676048,89.3591332550095));
#59116=CARTESIAN_POINT('Ctrl Pts',(4.7247156171568,-6.36006826030291,89.3443877444445));
#59117=CARTESIAN_POINT('Ctrl Pts',(4.33896271471279,-6.61498727071398,89.3283719608302));
#59118=CARTESIAN_POINT('Ctrl Pts',(4.31629827732005,-6.62979812715324,89.3274327848463));
#59119=CARTESIAN_POINT('Ctrl Pts',(4.2716612775224,-6.65864179977781,89.3255858970384));
#59120=CARTESIAN_POINT('Ctrl Pts',(4.24969449197723,-6.67268292414749,89.324678320952));
#59121=CARTESIAN_POINT('Ctrl Pts',(3.9025432626319,-6.89217169318522,89.3103506686897));
#59122=CARTESIAN_POINT('Ctrl Pts',(3.56287649826949,-7.07373798187514,89.2965490421296));
#59123=CARTESIAN_POINT('Ctrl Pts',(3.18654451040363,-7.24089723580959,89.2801986917944));
#59124=CARTESIAN_POINT('Ctrl Pts',(3.16166606070507,-7.25179470120666,89.2791135038575));
#59125=CARTESIAN_POINT('Ctrl Pts',(3.12937872866705,-7.26573973753404,89.2777000202331));
#59126=CARTESIAN_POINT('Ctrl Pts',(3.12202042797337,-7.26890456723875,89.2773775431543));
#59127=CARTESIAN_POINT('Ctrl Pts',(3.11023351509155,-7.27395295846982,89.2768604468178));
#59128=CARTESIAN_POINT('Ctrl Pts',(3.10580795564316,-7.27584366949584,89.2766661751491));
#59129=CARTESIAN_POINT('Ctrl Pts',(3.09742654276568,-7.27941538083581,89.276298025907));
#59130=CARTESIAN_POINT('Ctrl Pts',(3.09347103767822,-7.28109719846654,89.2761241876593));
#59131=CARTESIAN_POINT('Ctrl Pts',(3.08463313487316,-7.28484643182711,89.2757355671302));
#59132=CARTESIAN_POINT('Ctrl Pts',(3.07975002827901,-7.28691216326764,89.2755207049849));
#59133=CARTESIAN_POINT('Ctrl Pts',(3.06550553767511,-7.29292122430907,89.2748935247054));
#59134=CARTESIAN_POINT('Ctrl Pts',(3.0561386533032,-7.29685142482024,89.2744805920009));
#59135=CARTESIAN_POINT('Ctrl Pts',(2.98912729391316,-7.32481669350729,89.2715229097021));
#59136=CARTESIAN_POINT('Ctrl Pts',(2.93120858293906,-7.34818600197914,89.26894789772));
#59137=CARTESIAN_POINT('Ctrl Pts',(2.79937928928677,-7.39957049555669,89.2630537468386));
#59138=CARTESIAN_POINT('Ctrl Pts',(2.72531359035409,-7.42716858938268,89.259718928896));
#59139=CARTESIAN_POINT('Ctrl Pts',(2.48864030209973,-7.51134008422862,89.2490131471434));
#59140=CARTESIAN_POINT('Ctrl Pts',(2.32459649619534,-7.56371656309882,89.241520017253));
#59141=CARTESIAN_POINT('Ctrl Pts',(1.69625746811555,-7.74196188608367,89.2128111863276));
#59142=CARTESIAN_POINT('Ctrl Pts',(1.22250279643838,-7.83075861067771,89.1912226327961));
#59143=CARTESIAN_POINT('Ctrl Pts',(0.355586806039759,-7.91260965087965,
89.1534498721026));
#59144=CARTESIAN_POINT('Ctrl Pts',(-0.0346427271704981,-7.92052217273406,
89.137051902306));
#59145=CARTESIAN_POINT('Ctrl Pts',(-0.454066400820371,-7.89801607180187,
89.1200456741745));
#59146=CARTESIAN_POINT('Ctrl Pts',(-0.484232254232896,-7.89622399050183,
89.1188257751384));
#59147=CARTESIAN_POINT('Ctrl Pts',(-0.526451993314145,-7.89347296662957,
89.1171227557901));
#59148=CARTESIAN_POINT('Ctrl Pts',(-0.538514946732419,-7.89265917352457,
89.1166366676261));
#59149=CARTESIAN_POINT('Ctrl Pts',(-0.559406663639106,-7.8912016540365,
89.1157956590906));
#59150=CARTESIAN_POINT('Ctrl Pts',(-0.568236288369278,-7.89057075761805,
89.1154404782081));
#59151=CARTESIAN_POINT('Ctrl Pts',(-0.586535984417261,-7.88923232775255,
89.1147048870573));
#59152=CARTESIAN_POINT('Ctrl Pts',(-0.596005885657964,-7.88852255920834,
89.1143245220054));
#59153=CARTESIAN_POINT('Ctrl Pts',(-0.618084668208749,-7.88682777143586,
89.1134383992471));
#59154=CARTESIAN_POINT('Ctrl Pts',(-0.630692523789674,-7.88582956289625,
89.1129329107276));
#59155=CARTESIAN_POINT('Ctrl Pts',(-0.671030336334267,-7.88253851827012,
89.1113173048225));
#59156=CARTESIAN_POINT('Ctrl Pts',(-0.698750702845061,-7.88012961015698,
89.1102095691903));
#59157=CARTESIAN_POINT('Ctrl Pts',(-1.35235739907148,-7.8198549976142,89.0841492654076));
#59158=CARTESIAN_POINT('Ctrl Pts',(-1.96914830990073,-7.68775162937227,
89.0610759037641));
#59159=CARTESIAN_POINT('Ctrl Pts',(-2.84946623624924,-7.38617804129616,
89.0274148742448));
#59160=CARTESIAN_POINT('Ctrl Pts',(-3.12925990640804,-7.27205668559302,
89.0165517271842));
#59161=CARTESIAN_POINT('Ctrl Pts',(-3.62789555974646,-7.03455679761102,
88.9960599973247));
#59162=CARTESIAN_POINT('Ctrl Pts',(-3.84870077825114,-6.91622031359848,
88.9865453355541));
#59163=CARTESIAN_POINT('Ctrl Pts',(-4.06694093101584,-6.78556765952266,
88.9763686875647));
#59164=CARTESIAN_POINT('Ctrl Pts',(-4.07037118107815,-6.78351055475691,
88.9762085330883));
#59165=CARTESIAN_POINT('Ctrl Pts',(-4.07915945447243,-6.77823120263155,
88.9757977018391));
#59166=CARTESIAN_POINT('Ctrl Pts',(-4.08451521415381,-6.77500520711007,
88.9755468397382));
#59167=CARTESIAN_POINT('Ctrl Pts',(-4.09743618762421,-6.7672014804172,88.9749404224538));
#59168=CARTESIAN_POINT('Ctrl Pts',(-4.10499755047477,-6.76261741472149,
88.9745845493052));
#59169=CARTESIAN_POINT('Ctrl Pts',(-4.11682830684305,-6.75541788199236,
88.9740261523946));
#59170=CARTESIAN_POINT('Ctrl Pts',(-4.12110294489782,-6.75281101362623,
88.9738240698017));
#59171=CARTESIAN_POINT('Ctrl Pts',(-4.12875011361243,-6.74813745744278,
88.9734619647517));
#59172=CARTESIAN_POINT('Ctrl Pts',(-4.13212357734966,-6.74607229331455,
88.973302021409));
#59173=CARTESIAN_POINT('Ctrl Pts',(-4.13971081869726,-6.74141971607086,
88.9729418298523));
#59174=CARTESIAN_POINT('Ctrl Pts',(-4.14392371937384,-6.73883088217161,
88.9727415072194));
#59175=CARTESIAN_POINT('Ctrl Pts',(-4.15538303274237,-6.73177430715766,
88.9721957346512));
#59176=CARTESIAN_POINT('Ctrl Pts',(-4.16262465106402,-6.72729882529389,
88.9718498744976));
#59177=CARTESIAN_POINT('Ctrl Pts',(-4.19923122548385,-6.7045934065648,88.9700965957868));
#59178=CARTESIAN_POINT('Ctrl Pts',(-4.22848335818853,-6.68618307114781,
88.9686794297301));
#59179=CARTESIAN_POINT('Ctrl Pts',(-4.69752510172632,-6.38667441708362,
88.945681252535));
#59180=CARTESIAN_POINT('Ctrl Pts',(-5.10850401283036,-6.06295370217041,
88.9215726310023));
#59181=CARTESIAN_POINT('Ctrl Pts',(-5.66154109280362,-5.5309294247509,88.8861948247786));
#59182=CARTESIAN_POINT('Ctrl Pts',(-5.83049875783167,-5.35252442675633,
88.8748914044515));
#59183=CARTESIAN_POINT('Ctrl Pts',(-6.28721580259361,-4.82293649576689,
88.8432752308974));
#59184=CARTESIAN_POINT('Ctrl Pts',(-6.55345991249902,-4.45444168925678,
88.8235576805654));
#59185=CARTESIAN_POINT('Ctrl Pts',(-6.80264324137362,-4.03843196793117,
88.8038577727579));
#59186=CARTESIAN_POINT('Ctrl Pts',(-6.81846369651466,-4.01166308127975,
88.8026004478593));
#59187=CARTESIAN_POINT('Ctrl Pts',(-6.83937710423244,-3.97579558135538,
88.8009293820926));
#59188=CARTESIAN_POINT('Ctrl Pts',(-6.84461037545567,-3.96677935962294,
88.800510458813));
#59189=CARTESIAN_POINT('Ctrl Pts',(-6.85275279673124,-3.9526869768047,88.7998574569564));
#59190=CARTESIAN_POINT('Ctrl Pts',(-6.85567415440904,-3.94761790431529,
88.7996229282094));
#59191=CARTESIAN_POINT('Ctrl Pts',(-6.86124633256004,-3.93792434874941,
88.7991751229777));
#59192=CARTESIAN_POINT('Ctrl Pts',(-6.86389810695387,-3.93330041950039,
88.7989618114114));
#59193=CARTESIAN_POINT('Ctrl Pts',(-6.87007894387121,-3.92249753837498,
88.798464142224));
#59194=CARTESIAN_POINT('Ctrl Pts',(-6.87360434974099,-3.91631649348638,
88.7981799192967));
#59195=CARTESIAN_POINT('Ctrl Pts',(-6.88364814905541,-3.89865150148067,
88.7973691297412));
#59196=CARTESIAN_POINT('Ctrl Pts',(-6.89014614972879,-3.88715595359739,
88.7968433129656));
#59197=CARTESIAN_POINT('Ctrl Pts',(-6.93113556606187,-3.81421627517419,
88.7935183714467));
#59198=CARTESIAN_POINT('Ctrl Pts',(-6.96483406765398,-3.75232897935832,
88.7907483851077));
#59199=CARTESIAN_POINT('Ctrl Pts',(-7.06126245321642,-3.56946249255917,
88.7827081949463));
#59200=CARTESIAN_POINT('Ctrl Pts',(-7.12169974173409,-3.44730110506133,
88.7775205647258));
#59201=CARTESIAN_POINT('Ctrl Pts',(-7.25722827981026,-3.1545635264496,88.7654802538966));
#59202=CARTESIAN_POINT('Ctrl Pts',(-7.32950846528954,-2.98277446092834,
88.75872036824));
#59203=CARTESIAN_POINT('Ctrl Pts',(-7.57982224969622,-2.3236406137841,88.7336882429323));
#59204=CARTESIAN_POINT('Ctrl Pts',(-7.71583711485545,-1.82177387711307,
88.7165431482427));
#59205=CARTESIAN_POINT('Ctrl Pts',(-7.86387864189126,-0.940246937721175,
88.6857869976885));
#59206=CARTESIAN_POINT('Ctrl Pts',(-7.89960940394838,-0.566367179265717,
88.6725147964476));
#59207=CARTESIAN_POINT('Ctrl Pts',(-7.90917464792165,-0.171138357543796,
88.6570488046087));
#59208=CARTESIAN_POINT('Ctrl Pts',(-7.90958721712047,-0.150870773477243,
88.6562517007972));
#59209=CARTESIAN_POINT('Ctrl Pts',(-7.91046489100661,-0.097714372109889,
88.6541501364947));
#59210=CARTESIAN_POINT('Ctrl Pts',(-7.91080278230201,-0.0648241440126914,
88.6528387870776));
#59211=CARTESIAN_POINT('Ctrl Pts',(-7.91096447986695,-0.0247662112375243,
88.6512272635093));
#59212=CARTESIAN_POINT('Ctrl Pts',(-7.91098367050681,-0.0175991834095908,
88.6509383740784));
#59213=CARTESIAN_POINT('Ctrl Pts',(-7.91099755755862,-0.00706825328387941,
88.650513055333));
#59214=CARTESIAN_POINT('Ctrl Pts',(-7.91099984791095,-0.00370434700711826,
88.6503770698615));
#59215=CARTESIAN_POINT('Ctrl Pts',(-7.91099999267456,-0.000340445432580282,
88.6502409582738));
#59216=CARTESIAN_POINT('',(-7.91148363736201,-0.000479168433414057,86.6431685549391));
#59217=CARTESIAN_POINT('Ctrl Pts',(-7.91099997228721,-0.000662171981131852,
88.6422897498906));
#59218=CARTESIAN_POINT('Ctrl Pts',(-7.91101617651205,0.192930468445108,
88.6344460078403));
#59219=CARTESIAN_POINT('Ctrl Pts',(-7.90392191612403,0.386827054223198,
88.6266022657899));
#59220=CARTESIAN_POINT('Ctrl Pts',(-7.88967614590761,0.580457847475918,
88.6187585237396));
#59221=CARTESIAN_POINT('Ctrl Pts',(-7.87544710215177,0.773861291994232,
88.6109239913031));
#59222=CARTESIAN_POINT('Ctrl Pts',(-7.8540832936897,0.966999218801397,88.6030894588665));
#59223=CARTESIAN_POINT('Ctrl Pts',(-7.82559557608183,1.15929930544638,88.59525492643));
#59224=CARTESIAN_POINT('Ctrl Pts',(-7.79713576860348,1.35141099088641,88.5874280696808));
#59225=CARTESIAN_POINT('Ctrl Pts',(-7.76156600219742,1.54268612587329,88.5796012129317));
#59226=CARTESIAN_POINT('Ctrl Pts',(-7.71894909251944,1.73255473422727,88.5717743561825));
#59227=CARTESIAN_POINT('Ctrl Pts',(-7.67636565537242,1.92227421438498,88.5639536468689));
#59228=CARTESIAN_POINT('Ctrl Pts',(-7.62674617561062,2.11058902696814,88.5561329375553));
#59229=CARTESIAN_POINT('Ctrl Pts',(-7.57020501125693,2.29693645700976,88.5483122282417));
#59230=CARTESIAN_POINT('Ctrl Pts',(-7.51369727458084,2.48317371666689,88.5404961426063));
#59231=CARTESIAN_POINT('Ctrl Pts',(-7.45027610663762,2.66744557537262,88.5326800569709));
#59232=CARTESIAN_POINT('Ctrl Pts',(-7.38010651687637,2.84920143190315,88.5248639713355));
#59233=CARTESIAN_POINT('Ctrl Pts',(-7.30996478748406,3.03088512347963,88.5170509890249));
#59234=CARTESIAN_POINT('Ctrl Pts',(-7.23308010113027,3.21005447575066,88.5092380067143));
#59235=CARTESIAN_POINT('Ctrl Pts',(-7.14966676290338,3.38617574550328,88.5014250244038));
#59236=CARTESIAN_POINT('Ctrl Pts',(-7.06625658934013,3.56229033329605,88.4936123385141));
#59237=CARTESIAN_POINT('Ctrl Pts',(-6.976318399643,3.73535674746131,88.4857996526245));
#59238=CARTESIAN_POINT('Ctrl Pts',(-6.88011412013965,3.90486244237297,88.4779869667348));
#59239=CARTESIAN_POINT('Ctrl Pts',(-6.78390704196175,4.07437306836749,88.4701740535667));
#59240=CARTESIAN_POINT('Ctrl Pts',(-6.68143368381306,4.24032246244598,88.4623611403986));
#59241=CARTESIAN_POINT('Ctrl Pts',(-6.57300128222326,4.40222388616156,88.4545482272304));
#59242=CARTESIAN_POINT('Ctrl Pts',(-6.46454665411085,4.56415849650404,88.4467337125678));
#59243=CARTESIAN_POINT('Ctrl Pts',(-6.35013074497053,4.72204319132242,88.4389191979052));
#59244=CARTESIAN_POINT('Ctrl Pts',(-6.23010343430226,4.87542123286749,88.4311046832426));
#59245=CARTESIAN_POINT('Ctrl Pts',(-6.1100304073688,5.02885769337723,88.4232871921705));
#59246=CARTESIAN_POINT('Ctrl Pts',(-5.98434193808971,5.17778380469005,88.4154697010984));
#59247=CARTESIAN_POINT('Ctrl Pts',(-5.85342748423666,5.32177674153876,88.4076522100263));
#59248=CARTESIAN_POINT('Ctrl Pts',(-5.72237101359378,5.46592588279459,88.3998262384927));
#59249=CARTESIAN_POINT('Ctrl Pts',(-5.58607747208317,5.60513090081631,88.3920002669591));
#59250=CARTESIAN_POINT('Ctrl Pts',(-5.44497314654521,5.7390058750102,88.3841742954255));
#59251=CARTESIAN_POINT('Ctrl Pts',(-5.30378311612996,5.87296216307021,88.3763435705017));
#59252=CARTESIAN_POINT('Ctrl Pts',(-5.15777674140503,6.00158172369272,88.3685128455778));
#59253=CARTESIAN_POINT('Ctrl Pts',(-5.00741258114924,6.12451959276385,88.3606821206539));
#59254=CARTESIAN_POINT('Ctrl Pts',(-4.85684276259342,6.24762560824114,88.3528406853748));
#59255=CARTESIAN_POINT('Ctrl Pts',(-4.70190353317579,6.365034199289,88.3449992500957));
#59256=CARTESIAN_POINT('Ctrl Pts',(-4.54308248666159,6.47644366295182,88.3371578148165));
#59257=CARTESIAN_POINT('Ctrl Pts',(-4.45688458062388,6.53690959420772,88.3329019852761));
#59258=CARTESIAN_POINT('Ctrl Pts',(-4.36954368044602,6.59560919825888,88.3286461557357));
#59259=CARTESIAN_POINT('Ctrl Pts',(-4.28114058291619,6.65250000445757,88.3243903261953));
#59260=CARTESIAN_POINT('Ctrl Pts',(-4.11680779895752,6.75825449525617,88.316479151859));
#59261=CARTESIAN_POINT('Ctrl Pts',(-3.94833321133267,6.85805839596443,88.3085679775227));
#59262=CARTESIAN_POINT('Ctrl Pts',(-3.77618638520901,6.95157085730715,88.3006568031864));
#59263=CARTESIAN_POINT('Ctrl Pts',(-3.60422618859514,7.04498193900081,88.2927542055903));
#59264=CARTESIAN_POINT('Ctrl Pts',(-3.42860198368221,7.13211500411089,88.2848516079941));
#59265=CARTESIAN_POINT('Ctrl Pts',(-3.24981282724334,7.21267201443991,88.2769490103979));
#59266=CARTESIAN_POINT('Ctrl Pts',(-3.07118431319469,7.29315664414503,88.2690535133004));
#59267=CARTESIAN_POINT('Ctrl Pts',(-2.88939682496358,7.3670768487532,88.2611580162029));
#59268=CARTESIAN_POINT('Ctrl Pts',(-2.7049748219933,7.4341799959634,88.2532625191054));
#59269=CARTESIAN_POINT('Ctrl Pts',(-2.52068429929008,7.50123530322188,88.245372650957));
#59270=CARTESIAN_POINT('Ctrl Pts',(-2.33376332664721,7.5614831186337,88.2374827828085));
#59271=CARTESIAN_POINT('Ctrl Pts',(-2.14475744898914,7.61471841140601,88.2295929146601));
#59272=CARTESIAN_POINT('Ctrl Pts',(-1.9558512535615,7.66792562773547,88.2217072076503));
#59273=CARTESIAN_POINT('Ctrl Pts',(-1.76486267531535,7.7141275977776,88.2138215006405));
#59274=CARTESIAN_POINT('Ctrl Pts',(-1.57235383840462,7.7531686687995,88.2059357936307));
#59275=CARTESIAN_POINT('Ctrl Pts',(-1.37991082109503,7.79219639151094,88.1980527827781));
#59276=CARTESIAN_POINT('Ctrl Pts',(-1.18594891861128,7.82406802638898,88.1901697719255));
#59277=CARTESIAN_POINT('Ctrl Pts',(-0.991042179878032,7.84867864023637,
88.1822867610729));
#59278=CARTESIAN_POINT('Ctrl Pts',(-0.796132532452158,7.8732896213605,88.1744036325781));
#59279=CARTESIAN_POINT('Ctrl Pts',(-0.600278361625732,7.89063931335327,
88.1665205040834));
#59280=CARTESIAN_POINT('Ctrl Pts',(-0.404061179831432,7.900674373935,88.1586373755886));
#59281=CARTESIAN_POINT('Ctrl Pts',(-0.207831865732971,7.91071005499455,
88.1507537596721));
#59282=CARTESIAN_POINT('Ctrl Pts',(-0.0112398404968657,7.91343018521715,
88.1428701437557));
#59283=CARTESIAN_POINT('Ctrl Pts',(0.185130984511696,7.90883351187606,88.1349865278392));
#59284=CARTESIAN_POINT('Ctrl Pts',(0.38154696021655,7.9042357816417,88.1271010992769));
#59285=CARTESIAN_POINT('Ctrl Pts',(0.577741289492026,7.89231790362637,88.1192156707147));
#59286=CARTESIAN_POINT('Ctrl Pts',(0.773132540163403,7.87313070356008,88.1113302421524));
#59287=CARTESIAN_POINT('Ctrl Pts',(0.968601560950822,7.85393586655626,88.1034416750121));
#59288=CARTESIAN_POINT('Ctrl Pts',(1.16326652321196,7.8274659759085,88.0955531078717));
#59289=CARTESIAN_POINT('Ctrl Pts',(1.35655332800381,7.79382345631987,88.0876645407314));
#59290=CARTESIAN_POINT('Ctrl Pts',(1.55004583197328,7.76014513377707,88.0797675784408));
#59291=CARTESIAN_POINT('Ctrl Pts',(1.74215690905336,7.71927899479134,88.0718706161502));
#59292=CARTESIAN_POINT('Ctrl Pts',(1.93232374226966,7.67137836083327,88.0639736538596));
#59293=CARTESIAN_POINT('Ctrl Pts',(2.12260655195499,7.62344851386105,88.0560718754725));
#59294=CARTESIAN_POINT('Ctrl Pts',(2.31094242366053,7.56847571537108,88.0481700970855));
#59295=CARTESIAN_POINT('Ctrl Pts',(2.49678556671969,7.50666256293836,88.0402683186985));
#59296=CARTESIAN_POINT('Ctrl Pts',(2.68286906913444,7.44476946475546,88.0323563205836));
#59297=CARTESIAN_POINT('Ctrl Pts',(2.86645308139283,7.37601846231122,88.0244443224686));
#59298=CARTESIAN_POINT('Ctrl Pts',(3.04701253864999,7.30065994204016,88.0165323243536));
#59299=CARTESIAN_POINT('Ctrl Pts',(3.12266509464356,7.26908549691829,88.0132172784984));
#59300=CARTESIAN_POINT('Ctrl Pts',(3.19778698486359,7.23635163904106,88.0099022326431));
#59301=CARTESIAN_POINT('Ctrl Pts',(3.27234097360833,7.20247912544313,88.0065871867878));
#59302=CARTESIAN_POINT('Ctrl Pts',(3.45025978130267,7.12164431922523,87.9986760204511));
#59303=CARTESIAN_POINT('Ctrl Pts',(3.62542070534692,7.03410441248774,87.9907648541143));
#59304=CARTESIAN_POINT('Ctrl Pts',(3.79728286212815,6.94006944237504,87.9828536877776));
#59305=CARTESIAN_POINT('Ctrl Pts',(3.96895872577255,6.84613640319283,87.9749510968948));
#59306=CARTESIAN_POINT('Ctrl Pts',(4.13734264475762,6.74572248817744,87.9670485060119));
#59307=CARTESIAN_POINT('Ctrl Pts',(4.30191374327858,6.63908571607498,87.9591459151291));
#59308=CARTESIAN_POINT('Ctrl Pts',(4.46633700092785,6.53254474009641,87.9512504234631));
#59309=CARTESIAN_POINT('Ctrl Pts',(4.62695397386723,6.41979222962641,87.9433549317972));
#59310=CARTESIAN_POINT('Ctrl Pts',(4.78326819030697,6.30113215379566,87.9354594401312));
#59311=CARTESIAN_POINT('Ctrl Pts',(4.93947099063381,6.18255665532905,87.9275695761363));
#59312=CARTESIAN_POINT('Ctrl Pts',(5.09137687119333,6.05808218837905,87.9196797121413));
#59313=CARTESIAN_POINT('Ctrl Pts',(5.23851794852022,5.92805623311988,87.9117898481464));
#59314=CARTESIAN_POINT('Ctrl Pts',(5.38558144697159,5.79809883293439,87.9039041440149));
#59315=CARTESIAN_POINT('Ctrl Pts',(5.52788489031669,5.66259600463352,87.8960184398834));
#59316=CARTESIAN_POINT('Ctrl Pts',(5.66499291790816,5.52193591415641,87.8881327357518));
#59317=CARTESIAN_POINT('Ctrl Pts',(5.80205408979531,5.38132389327614,87.8802497265042));
#59318=CARTESIAN_POINT('Ctrl Pts',(5.93392314415944,5.23555836949925,87.8723667172566));
#59319=CARTESIAN_POINT('Ctrl Pts',(6.06020089225338,5.0850650089779,87.864483708009));
#59320=CARTESIAN_POINT('Ctrl Pts',(6.18648055533892,4.93456936623717,87.8566005792162));
#59321=CARTESIAN_POINT('Ctrl Pts',(6.30716851462362,4.77934600219118,87.8487174504234));
#59322=CARTESIAN_POINT('Ctrl Pts',(6.4219049024596,4.61985480548528,87.8408343216306));
#59323=CARTESIAN_POINT('Ctrl Pts',(6.53664840183501,4.46035372326741,87.8329507042292));
#59324=CARTESIAN_POINT('Ctrl Pts',(6.64543939272819,4.29658456102768,87.8250670868279));
#59325=CARTESIAN_POINT('Ctrl Pts',(6.7479604915137,4.1290374429121,87.8171834694265));
#59326=CARTESIAN_POINT('Ctrl Pts',(6.85050517796842,3.96145177618513,87.8092980381921));
#59327=CARTESIAN_POINT('Ctrl Pts',(6.94677691775842,3.79008671576593,87.8014126069577));
#59328=CARTESIAN_POINT('Ctrl Pts',(7.03650344463055,3.61545851500228,87.7935271757232));
#59329=CARTESIAN_POINT('Ctrl Pts',(7.12626569819126,3.44076078198807,87.7856386047223));
#59330=CARTESIAN_POINT('Ctrl Pts',(7.20947738837047,3.26279762621829,87.7777500337213));
#59331=CARTESIAN_POINT('Ctrl Pts',(7.28591359288956,3.08210709044107,87.7698614627204));
#59332=CARTESIAN_POINT('Ctrl Pts',(7.3624311593015,2.90122422010065,87.7619644947945));
#59333=CARTESIAN_POINT('Ctrl Pts',(7.43215870012965,2.71760848876809,87.7540675268687));
#59334=CARTESIAN_POINT('Ctrl Pts',(7.49492018598347,2.53181602920464,87.7461705589428));
#59335=CARTESIAN_POINT('Ctrl Pts',(7.55771995609665,2.34591023697208,87.7382687738976));
#59336=CARTESIAN_POINT('Ctrl Pts',(7.61354510185648,2.15782539911996,87.7303669888524));
#59337=CARTESIAN_POINT('Ctrl Pts',(7.66227023652275,1.96813003190787,87.7224652038072));
#59338=CARTESIAN_POINT('Ctrl Pts',(7.71105839888217,1.77818928699738,87.7145531975222));
#59339=CARTESIAN_POINT('Ctrl Pts',(7.75272813269699,1.5866341875338,87.7066411912373));
#59340=CARTESIAN_POINT('Ctrl Pts',(7.78720544793176,1.39404171806369,87.6987291849523));
#59341=CARTESIAN_POINT('Ctrl Pts',(7.80165107359589,1.31334753695498,87.6954141390949));
#59342=CARTESIAN_POINT('Ctrl Pts',(7.8148346838919,1.23247128898822,87.6920990932375));
#59343=CARTESIAN_POINT('Ctrl Pts',(7.82675355380094,1.15145551718874,87.68878404738));
#59344=CARTESIAN_POINT('Ctrl Pts',(7.85494261024235,0.959846901495308,87.6809437055108));
#59345=CARTESIAN_POINT('Ctrl Pts',(7.87613359187413,0.766914325471691,87.6731033636416));
#59346=CARTESIAN_POINT('Ctrl Pts',(7.89020557749282,0.573216315976064,87.6652630217724));
#59347=CARTESIAN_POINT('Ctrl Pts',(7.9042618302128,0.379734866619543,87.6574314456388));
#59348=CARTESIAN_POINT('Ctrl Pts',(7.91121491034272,0.1854900348259,87.6495998695051));
#59349=CARTESIAN_POINT('Ctrl Pts',(7.91099493745802,-0.00894983315554786,
87.6417682933715));
#59350=CARTESIAN_POINT('Ctrl Pts',(7.91077516773731,-0.203210119100259,
87.6339439503758));
#59351=CARTESIAN_POINT('Ctrl Pts',(7.90339553874417,-0.397664733449155,
87.6261196073801));
#59352=CARTESIAN_POINT('Ctrl Pts',(7.88883795724331,-0.591740385944079,
87.6182952643844));
#59353=CARTESIAN_POINT('Ctrl Pts',(7.87429099179311,-0.785674509644466,
87.6104766272556));
#59354=CARTESIAN_POINT('Ctrl Pts',(7.85257652571912,-0.97922987291739,87.6026579901268));
#59355=CARTESIAN_POINT('Ctrl Pts',(7.82372852464297,-1.17183316760019,87.594839352998));
#59356=CARTESIAN_POINT('Ctrl Pts',(7.79489595650251,-1.36433342449357,87.5870248986381));
#59357=CARTESIAN_POINT('Ctrl Pts',(7.75893750744041,-1.55588228058694,87.5792104442783));
#59358=CARTESIAN_POINT('Ctrl Pts',(7.71593899617526,-1.74591134004619,87.5713959899184));
#59359=CARTESIAN_POINT('Ctrl Pts',(7.67295513663862,-1.93587564716625,87.5635841983313));
#59360=CARTESIAN_POINT('Ctrl Pts',(7.62293607211913,-2.1243208469729,87.5557724067442));
#59361=CARTESIAN_POINT('Ctrl Pts',(7.56601879313652,-2.31068834374196,87.5479606151571));
#59362=CARTESIAN_POINT('Ctrl Pts',(7.50909885033314,-2.49706456281148,87.5401484579655));
#59363=CARTESIAN_POINT('Ctrl Pts',(7.44528014202093,-2.68136254560945,87.5323363007739));
#59364=CARTESIAN_POINT('Ctrl Pts',(7.37474979339316,-2.8630379817333,87.5245241435823));
#59365=CARTESIAN_POINT('Ctrl Pts',(7.30421367884538,-3.04472826998895,87.5167113477398));
#59366=CARTESIAN_POINT('Ctrl Pts',(7.22696495757362,-3.22379525616171,87.5088985518972));
#59367=CARTESIAN_POINT('Ctrl Pts',(7.14323922955342,-3.39971385698401,87.5010857560547));
#59368=CARTESIAN_POINT('Ctrl Pts',(7.05949192461862,-3.57567779369907,87.4932709467805));
#59369=CARTESIAN_POINT('Ctrl Pts',(6.96926443882062,-3.74849141107556,87.4854561375064));
#59370=CARTESIAN_POINT('Ctrl Pts',(6.87283878831291,-3.91765337796257,87.4776413282322));
#59371=CARTESIAN_POINT('Ctrl Pts',(6.77637131962863,-4.08688870753847,87.4698231298072));
#59372=CARTESIAN_POINT('Ctrl Pts',(6.67370050552191,-4.25246892663546,87.4620049313822));
#59373=CARTESIAN_POINT('Ctrl Pts',(6.56515228678159,-4.41392075725952,87.4541867329572));
#59374=CARTESIAN_POINT('Ctrl Pts',(6.45647771850363,-4.57556051693841,87.4463594341917));
#59375=CARTESIAN_POINT('Ctrl Pts',(6.34191227797189,-4.73306199849868,87.4385321354261));
#59376=CARTESIAN_POINT('Ctrl Pts',(6.2218235514863,-4.88598328836381,87.4307048366606));
#59377=CARTESIAN_POINT('Ctrl Pts',(6.10165643059092,-5.03900440586982,87.4228724282025));
#59378=CARTESIAN_POINT('Ctrl Pts',(5.9759590648151,-5.18743910578546,87.4150400197445));
#59379=CARTESIAN_POINT('Ctrl Pts',(5.84513670267974,-5.33088153376027,87.4072076112864));
#59380=CARTESIAN_POINT('Ctrl Pts',(5.71412659201988,-5.47452982183241,87.3993639622185));
#59381=CARTESIAN_POINT('Ctrl Pts',(5.57797704021789,-5.61317127831506,87.3915203131506));
#59382=CARTESIAN_POINT('Ctrl Pts',(5.4371280975494,-5.74643881467808,87.3836766640827));
#59383=CARTESIAN_POINT('Ctrl Pts',(5.36113524400898,-5.81834123851355,87.3794447453792));
#59384=CARTESIAN_POINT('Ctrl Pts',(5.28377495384006,-5.88868004508179,87.3752128266758));
#59385=CARTESIAN_POINT('Ctrl Pts',(5.20511988185005,-5.9574027911137,87.3709809079724));
#59386=CARTESIAN_POINT('Ctrl Pts',(5.05795934123553,-6.08598034120298,87.3630631548195));
#59387=CARTESIAN_POINT('Ctrl Pts',(4.90582489946001,-6.20928263008101,87.3551454016667));
#59388=CARTESIAN_POINT('Ctrl Pts',(4.74912962242098,-6.32690199303289,87.3472276485139));
#59389=CARTESIAN_POINT('Ctrl Pts',(4.5926143769801,-6.44438621980016,87.3393189922896));
#59390=CARTESIAN_POINT('Ctrl Pts',(4.43154900633982,-6.55620032110361,87.3314103360654));
#59391=CARTESIAN_POINT('Ctrl Pts',(4.26638219957893,-6.66197447661848,87.3235016798412));
#59392=CARTESIAN_POINT('Ctrl Pts',(4.10137458291387,-6.76764668551173,87.3156006460914));
#59393=CARTESIAN_POINT('Ctrl Pts',(3.93227369282455,-6.86729036074609,87.3076996123415));
#59394=CARTESIAN_POINT('Ctrl Pts',(3.7595601978472,-6.96057670877659,87.2997985785916));
#59395=CARTESIAN_POINT('Ctrl Pts',(3.58698120608346,-7.05379040867037,87.2919036978897));
#59396=CARTESIAN_POINT('Ctrl Pts',(3.41079551620029,-7.1406564821353,87.2840088171879));
#59397=CARTESIAN_POINT('Ctrl Pts',(3.23151184679387,-7.22088998559256,87.276113936486));
#59398=CARTESIAN_POINT('Ctrl Pts',(3.05233462934893,-7.30107584938555,87.2682237434701));
#59399=CARTESIAN_POINT('Ctrl Pts',(2.87006341120434,-7.3746368500975,87.2603335504542));
#59400=CARTESIAN_POINT('Ctrl Pts',(2.68523078157349,-7.44133433261067,87.2524433574383));
#59401=CARTESIAN_POINT('Ctrl Pts',(2.50047371056953,-7.50800454953655,87.2445563898926));
#59402=CARTESIAN_POINT('Ctrl Pts',(2.31315763840243,-7.56781672335792,87.236669422347));
#59403=CARTESIAN_POINT('Ctrl Pts',(2.12383463325769,-7.62058051926329,87.2287824548013));
#59404=CARTESIAN_POINT('Ctrl Pts',(1.9345280695243,-7.67333973299296,87.220896172185));
#59405=CARTESIAN_POINT('Ctrl Pts',(1.74321524998539,-7.71905168968404,87.2130098895686));
#59406=CARTESIAN_POINT('Ctrl Pts',(1.55046339164132,-7.75757592751628,87.2051236069523));
#59407=CARTESIAN_POINT('Ctrl Pts',(1.35771187208615,-7.79610009763668,87.1972373381973));
#59408=CARTESIAN_POINT('Ctrl Pts',(1.16352165655767,-7.82743650599629,87.1893510694422));
#59409=CARTESIAN_POINT('Ctrl Pts',(0.96847025096779,-7.85149580481263,87.1814648006871));
#59410=CARTESIAN_POINT('Ctrl Pts',(0.773386496578017,-7.87555909380501,
87.1735772240136));
#59411=CARTESIAN_POINT('Ctrl Pts',(0.577441609510269,-7.89234282628704,
87.1656896473401));
#59412=CARTESIAN_POINT('Ctrl Pts',(0.381218567815195,-7.90180950185164,
87.1578020706666));
#59413=CARTESIAN_POINT('Ctrl Pts',(0.184930094871308,-7.91127933411181,
87.1499118638535));
#59414=CARTESIAN_POINT('Ctrl Pts',(-0.0116363735729002,-7.91342723140898,
87.1420216570404));
#59415=CARTESIAN_POINT('Ctrl Pts',(-0.207897251873945,-7.90826780860785,
87.1341314502273));
#59416=CARTESIAN_POINT('Ctrl Pts',(-0.404347651713557,-7.9031034035517,
87.1262336241466));
#59417=CARTESIAN_POINT('Ctrl Pts',(-0.600491527419305,-7.89061759293021,
87.118335798066));
#59418=CARTESIAN_POINT('Ctrl Pts',(-0.795748747031074,-7.87087701159143,
87.1104379719854));
#59419=CARTESIAN_POINT('Ctrl Pts',(-0.991114084255854,-7.85112549951966,
87.1025357727292));
#59420=CARTESIAN_POINT('Ctrl Pts',(-1.18559144598008,-7.82411125464705,
87.094633573473));
#59421=CARTESIAN_POINT('Ctrl Pts',(-1.37860999873653,-7.7899522123941,87.0867313742168));
#59422=CARTESIAN_POINT('Ctrl Pts',(-1.57186153952061,-7.75575193758724,
87.078819636407));
#59423=CARTESIAN_POINT('Ctrl Pts',(-1.76365041813369,-7.71438971118454,
87.0709078985972));
#59424=CARTESIAN_POINT('Ctrl Pts',(-1.9534190268028,-7.66603385759056,87.0629961607873));
#59425=CARTESIAN_POINT('Ctrl Pts',(-2.03191937974922,-7.64603080439449,
87.0597233633798));
#59426=CARTESIAN_POINT('Ctrl Pts',(-2.11007423792459,-7.62483159989217,
87.0564505659722));
#59427=CARTESIAN_POINT('Ctrl Pts',(-2.1878450953644,-7.60245058114092,87.0531777685646));
#59428=CARTESIAN_POINT('Ctrl Pts',(-2.38542943084931,-7.54558945265377,
87.044862912303));
#59429=CARTESIAN_POINT('Ctrl Pts',(-2.58096509958468,-7.48097278119449,
87.0365480560414));
#59430=CARTESIAN_POINT('Ctrl Pts',(-2.77383604934864,-7.40876201340912,
87.0282331997798));
#59431=CARTESIAN_POINT('Ctrl Pts',(-2.9664694852428,-7.33664017067399,87.0199285829747));
#59432=CARTESIAN_POINT('Ctrl Pts',(-3.1564444736579,-7.25694298576827,87.0116239661695));
#59433=CARTESIAN_POINT('Ctrl Pts',(-3.34315965244035,-7.16988176599133,
87.0033193493644));
#59434=CARTESIAN_POINT('Ctrl Pts',(-3.52965721390785,-7.08292201642697,
86.9950244116246));
#59435=CARTESIAN_POINT('Ctrl Pts',(-3.71290227882356,-6.98861547418967,
86.9867294738847));
#59436=CARTESIAN_POINT('Ctrl Pts',(-3.89231224160578,-6.88722196635521,
86.9784345361449));
#59437=CARTESIAN_POINT('Ctrl Pts',(-4.07145330221265,-6.78598042853625,
86.9701520309744));
#59438=CARTESIAN_POINT('Ctrl Pts',(-4.24677047737049,-6.67767326686733,
86.9618695258039));
#59439=CARTESIAN_POINT('Ctrl Pts',(-4.41770452726697,-6.56260677701818,
86.9535870206334));
#59440=CARTESIAN_POINT('Ctrl Pts',(-4.58848154989358,-6.44764599212813,
86.9453121241235));
#59441=CARTESIAN_POINT('Ctrl Pts',(-4.75488323437949,-6.32593842478341,
86.9370372276136));
#59442=CARTESIAN_POINT('Ctrl Pts',(-4.91637660617609,-6.19783527259675,
86.9287623311037));
#59443=CARTESIAN_POINT('Ctrl Pts',(-5.07768525073537,-6.06987865361534,
86.9204968999902));
#59444=CARTESIAN_POINT('Ctrl Pts',(-5.23409655674919,-5.93554122966022,
86.9122314688767));
#59445=CARTESIAN_POINT('Ctrl Pts',(-5.38510788171419,-5.79521648450683,
86.9039660377632));
#59446=CARTESIAN_POINT('Ctrl Pts',(-5.44411974252883,-5.74038070095378,
86.9007360914624));
#59447=CARTESIAN_POINT('Ctrl Pts',(-5.50230731480781,-5.68463106667982,
86.8975061451616));
#59448=CARTESIAN_POINT('Ctrl Pts',(-5.55964191238288,-5.6279927866048,86.8942761988609));
#59449=CARTESIAN_POINT('Ctrl Pts',(-5.70638134036553,-5.48303548034222,
86.8860096287159));
#59450=CARTESIAN_POINT('Ctrl Pts',(-5.84736570408403,-5.33241794497542,
86.8777430585709));
#59451=CARTESIAN_POINT('Ctrl Pts',(-5.98217903531012,-5.17662583054794,
86.8694764884259));
#59452=CARTESIAN_POINT('Ctrl Pts',(-6.11711316084189,-5.02069412458212,
86.8612025113384));
#59453=CARTESIAN_POINT('Ctrl Pts',(-6.24586502313868,-4.85957880544821,
86.8529285342508));
#59454=CARTESIAN_POINT('Ctrl Pts',(-6.36805989143172,-4.69379741990839,
86.8446545571633));
#59455=CARTESIAN_POINT('Ctrl Pts',(-6.49037217927032,-4.52785673164804,
86.8363726294421));
#59456=CARTESIAN_POINT('Ctrl Pts',(-6.6061147200344,-4.35724126169245,86.8280907017209));
#59457=CARTESIAN_POINT('Ctrl Pts',(-6.71495647049175,-4.18249693357939,
86.8198087739998));
#59458=CARTESIAN_POINT('Ctrl Pts',(-6.82397863896027,-4.00746294617651,
86.8115131180087));
#59459=CARTESIAN_POINT('Ctrl Pts',(-6.92607699242537,-3.82828666728563,
86.8032174620176));
#59460=CARTESIAN_POINT('Ctrl Pts',(-7.02096579852531,-3.64553977566257,
86.7949218060265));
#59461=CARTESIAN_POINT('Ctrl Pts',(-7.11594036574239,-3.46262771621598,
86.7866186523678));
#59462=CARTESIAN_POINT('Ctrl Pts',(-7.20369224976595,-3.27613886560742,
86.7783154987092));
#59463=CARTESIAN_POINT('Ctrl Pts',(-7.28398363721479,-3.08666541315823,
86.7700123450505));
#59464=CARTESIAN_POINT('Ctrl Pts',(-7.3643974398656,-2.89690308251565,86.7616965320985));
#59465=CARTESIAN_POINT('Ctrl Pts',(-7.43732790142503,-2.70414732723279,
86.7533807191463));
#59466=CARTESIAN_POINT('Ctrl Pts',(-7.50258627025342,-2.50900782330484,
86.7450649061943));
#59467=CARTESIAN_POINT('Ctrl Pts',(-7.52793443030262,-2.43321022881555,
86.7418348138485));
#59468=CARTESIAN_POINT('Ctrl Pts',(-7.55212559578346,-2.35705311822049,
86.7386047215028));
#59469=CARTESIAN_POINT('Ctrl Pts',(-7.57515077475619,-2.28057267801548,
86.735374629157));
#59470=CARTESIAN_POINT('Ctrl Pts',(-7.64221455117157,-2.0578136215871,86.7259665723887));
#59471=CARTESIAN_POINT('Ctrl Pts',(-7.69948580999344,-1.83197078554786,
86.7165585156204));
#59472=CARTESIAN_POINT('Ctrl Pts',(-7.7467180442272,-1.60383307836095,86.7071504588521));
#59473=CARTESIAN_POINT('Ctrl Pts',(-7.79374174447566,-1.37670261688337,
86.6977839393856));
#59474=CARTESIAN_POINT('Ctrl Pts',(-7.83081481159807,-1.14729754423536,
86.6884174199192));
#59475=CARTESIAN_POINT('Ctrl Pts',(-7.85774156116296,-0.916416148904123,
86.6790509004527));
#59476=CARTESIAN_POINT('Ctrl Pts',(-7.88444665396917,-0.687435332831672,
86.6697614846983));
#59477=CARTESIAN_POINT('Ctrl Pts',(-7.90117173216421,-0.457002455362897,
86.660472068944));
#59478=CARTESIAN_POINT('Ctrl Pts',(-7.90777360586571,-0.225915024674476,
86.6511826531896));
#59479=CARTESIAN_POINT('Ctrl Pts',(-7.90987040587394,-0.152520084316735,
86.6482322715387));
#59480=CARTESIAN_POINT('Ctrl Pts',(-7.91094640363994,-0.0790592559262316,
86.6452818898878));
#59481=CARTESIAN_POINT('Ctrl Pts',(-7.91099804723377,-0.00555847671740886,
86.6423315082369));
#59482=CARTESIAN_POINT('',(-7.911,2.65620858641569E-12,84.6423315082369));
#59483=CARTESIAN_POINT('Ctrl Pts',(-7.911,3.27626814566884E-12,86.6423315082369));
#59484=CARTESIAN_POINT('Ctrl Pts',(-7.91099999999909,2.20167589667007,86.5537440725042));
#59485=CARTESIAN_POINT('Ctrl Pts',(-6.94214576672187,4.38610418338976,86.4651566367714));
#59486=CARTESIAN_POINT('Ctrl Pts',(-3.67820201487972,7.3418068410779,86.287981765306));
#59487=CARTESIAN_POINT('Ctrl Pts',(-1.40868175871393,8.08992666571398,86.1993943295733));
#59488=CARTESIAN_POINT('Ctrl Pts',(2.97309270521611,7.65454228025127,86.0222194581078));
#59489=CARTESIAN_POINT('Ctrl Pts',(5.05102072675891,6.47444880834002,85.9336320223751));
#59490=CARTESIAN_POINT('Ctrl Pts',(7.66951518848004,2.93425195367362,85.7564571509096));
#59491=CARTESIAN_POINT('Ctrl Pts',(8.18956872247099,0.601881960095445,85.6678697151769));
#59492=CARTESIAN_POINT('Ctrl Pts',(7.32306689761172,-3.71537198232788,85.4906948437114));
#59493=CARTESIAN_POINT('Ctrl Pts',(5.94329958849939,-5.66643518936788,85.4021074079787));
#59494=CARTESIAN_POINT('Ctrl Pts',(2.16154501637474,-7.92205913233101,85.2249325365133));
#59495=CARTESIAN_POINT('Ctrl Pts',(-0.210816529304274,-8.20894963712993,
85.1363451007805));
#59496=CARTESIAN_POINT('Ctrl Pts',(-4.42123908576771,-6.91982244717618,
84.9591702293151));
#59497=CARTESIAN_POINT('Ctrl Pts',(-6.22631625634449,-5.35390358803218,
84.8705827935823));
#59498=CARTESIAN_POINT('Ctrl Pts',(-7.65317280859585,-2.31334857514181,
84.735440741312));
#59499=CARTESIAN_POINT('Ctrl Pts',(-7.91100000000039,-1.15702837836213,
84.6888861247745));
#59500=CARTESIAN_POINT('Ctrl Pts',(-7.911,2.65620858641569E-12,84.6423315082369));
#59501=CARTESIAN_POINT('',(-7.91099994247235,0.000954045336348954,82.6424993008866));
#59502=CARTESIAN_POINT('Ctrl Pts',(-7.9109995798286,0.00257836221761484,
84.6423315082369));
#59503=CARTESIAN_POINT('Ctrl Pts',(-7.91093006408187,0.215868426519756,
84.633779099046));
#59504=CARTESIAN_POINT('Ctrl Pts',(-7.90223050541358,0.428942177783995,
84.6252266898552));
#59505=CARTESIAN_POINT('Ctrl Pts',(-7.88497845690452,0.641120686104887,
84.6166742806643));
#59506=CARTESIAN_POINT('Ctrl Pts',(-7.8671728985271,0.860106669964004,84.6078474783842));
#59507=CARTESIAN_POINT('Ctrl Pts',(-7.84025706044039,1.07813871609647,84.5990206761041));
#59508=CARTESIAN_POINT('Ctrl Pts',(-7.80437267238277,1.29448375446159,84.590193873824));
#59509=CARTESIAN_POINT('Ctrl Pts',(-7.76943768043388,1.50510493494078,84.5816006029539));
#59510=CARTESIAN_POINT('Ctrl Pts',(-7.72600276107914,1.71412702819638,84.5730073320837));
#59511=CARTESIAN_POINT('Ctrl Pts',(-7.67424943977649,1.92088951688799,84.5644140612136));
#59512=CARTESIAN_POINT('Ctrl Pts',(-7.62038643993448,2.13608049623799,84.5554704932285));
#59513=CARTESIAN_POINT('Ctrl Pts',(-7.55751280045111,2.34882350066785,84.5465269252435));
#59514=CARTESIAN_POINT('Ctrl Pts',(-7.48588883338284,2.55839585956397,84.5375833572584));
#59515=CARTESIAN_POINT('Ctrl Pts',(-7.41426486631458,2.7679682184601,84.5286397892734));
#59516=CARTESIAN_POINT('Ctrl Pts',(-7.33389072764557,2.97436967862314,84.5196962212883));
#59517=CARTESIAN_POINT('Ctrl Pts',(-7.24508130678783,3.1769038163019,84.5107526533033));
#59518=CARTESIAN_POINT('Ctrl Pts',(-7.16652560102665,3.35605386561449,84.5028416874587));
#59519=CARTESIAN_POINT('Ctrl Pts',(-7.08122200956264,3.53251459720829,84.494930721614));
#59520=CARTESIAN_POINT('Ctrl Pts',(-6.9893770106968,3.70574284082733,84.4870197557694));
#59521=CARTESIAN_POINT('Ctrl Pts',(-6.89762495048163,3.87879579347335,84.4791167950911));
#59522=CARTESIAN_POINT('Ctrl Pts',(-6.79934482819329,4.04862247186651,84.4712138344127));
#59523=CARTESIAN_POINT('Ctrl Pts',(-6.69479123344108,4.21469943657202,84.4633108737344));
#59524=CARTESIAN_POINT('Ctrl Pts',(-6.59032408841021,4.38063908120398,84.4554144475875));
#59525=CARTESIAN_POINT('Ctrl Pts',(-6.47959398724002,4.5428348988684,84.4475180214406));
#59526=CARTESIAN_POINT('Ctrl Pts',(-6.36290162547618,4.70078758342819,84.4396215952936));
#59527=CARTESIAN_POINT('Ctrl Pts',(-6.24628416092563,4.85863888846555,84.4317302373475));
#59528=CARTESIAN_POINT('Ctrl Pts',(-6.1237122643645,5.01225221047996,84.4238388794013));
#59529=CARTESIAN_POINT('Ctrl Pts',(-5.9955303235939,5.16115656988489,84.4159475214551));
#59530=CARTESIAN_POINT('Ctrl Pts',(-5.86740694403511,5.30999290083216,84.4080597687553));
#59531=CARTESIAN_POINT('Ctrl Pts',(-5.73367885193989,5.45412429566728,84.4001720160556));
#59532=CARTESIAN_POINT('Ctrl Pts',(-5.59473132726087,5.59311204748893,84.3922842633558));
#59533=CARTESIAN_POINT('Ctrl Pts',(-5.45582158411724,5.73206200683694,84.3843986554327));
#59534=CARTESIAN_POINT('Ctrl Pts',(-5.31169548047284,5.86587086750381,84.3765130475096));
#59535=CARTESIAN_POINT('Ctrl Pts',(-5.16277602726376,5.99413585867976,84.3686274395865));
#59536=CARTESIAN_POINT('Ctrl Pts',(-5.01383901029741,6.12241597759843,84.3607409016244));
#59537=CARTESIAN_POINT('Ctrl Pts',(-4.86010777076724,6.24515069055797,84.3528543636623));
#59538=CARTESIAN_POINT('Ctrl Pts',(-4.70203984142614,6.36197629118824,84.3449678257001));
#59539=CARTESIAN_POINT('Ctrl Pts',(-4.54395199851371,6.47881660963597,84.3370802941833));
#59540=CARTESIAN_POINT('Ctrl Pts',(-4.38152665391761,6.58974612692609,84.3291927626665));
#59541=CARTESIAN_POINT('Ctrl Pts',(-4.21525184874517,6.69444343105911,84.3213052311496));
#59542=CARTESIAN_POINT('Ctrl Pts',(-4.04892822650996,6.79917147355241,84.3134153839114));
#59543=CARTESIAN_POINT('Ctrl Pts',(-3.87875318305699,6.89766347302662,84.3055255366732));
#59544=CARTESIAN_POINT('Ctrl Pts',(-3.70524118047121,6.98964296617076,84.297635689435));
#59545=CARTESIAN_POINT('Ctrl Pts',(-3.53164915276753,7.08166488098989,84.2897422033363));
#59546=CARTESIAN_POINT('Ctrl Pts',(-3.35471740313413,7.16716814282994,84.2818487172377));
#59547=CARTESIAN_POINT('Ctrl Pts',(-3.17498249196566,7.24592348674146,84.2739552311391));
#59548=CARTESIAN_POINT('Ctrl Pts',(-2.99503980748883,7.32476987172146,84.2660526201815));
#59549=CARTESIAN_POINT('Ctrl Pts',(-2.81228780450381,7.39685261935806,84.2581500092239));
#59550=CARTESIAN_POINT('Ctrl Pts',(-2.62728150413383,7.46199121535507,84.2502473982662));
#59551=CARTESIAN_POINT('Ctrl Pts',(-2.44215249750421,7.52717301481844,84.2423395458664));
#59552=CARTESIAN_POINT('Ctrl Pts',(-2.25476654067875,7.58540137886259,84.2344316934666));
#59553=CARTESIAN_POINT('Ctrl Pts',(-2.0656913623117,7.63654635261719,84.2265238410668));
#59554=CARTESIAN_POINT('Ctrl Pts',(-1.87635747547357,7.68776130720204,84.2186051684819));
#59555=CARTESIAN_POINT('Ctrl Pts',(-1.68533008489886,7.73187343546429,84.2106864958971));
#59556=CARTESIAN_POINT('Ctrl Pts',(-1.49318575785475,7.76880410954863,84.2027678233123));
#59557=CARTESIAN_POINT('Ctrl Pts',(-1.41377293390896,7.78406747518829,84.1994950535068));
#59558=CARTESIAN_POINT('Ctrl Pts',(-1.33416936762576,7.79810475494626,84.1962222837012));
#59559=CARTESIAN_POINT('Ctrl Pts',(-1.25441587480513,7.8109129948449,84.1929495138956));
#59560=CARTESIAN_POINT('Ctrl Pts',(-1.06328808945263,7.84160770725826,84.1851063809771));
#59561=CARTESIAN_POINT('Ctrl Pts',(-0.870733243483305,7.8653311749436,84.1772632480586));
#59562=CARTESIAN_POINT('Ctrl Pts',(-0.677307280746736,7.88195254029403,
84.1694201151401));
#59563=CARTESIAN_POINT('Ctrl Pts',(-0.484108476215863,7.89855438561996,
84.1615861931465));
#59564=CARTESIAN_POINT('Ctrl Pts',(-0.290040938258333,7.90807070657361,
84.1537522711528));
#59565=CARTESIAN_POINT('Ctrl Pts',(-0.0956713935766871,7.91042147957055,
84.1459183491591));
#59566=CARTESIAN_POINT('Ctrl Pts',(0.098507686294237,7.9127699490197,84.13809210371));
#59567=CARTESIAN_POINT('Ctrl Pts',(0.292987834792579,7.9079668492622,84.1302658582608));
#59568=CARTESIAN_POINT('Ctrl Pts',(0.487196402186665,7.89598383139786,84.1224396128117));
#59569=CARTESIAN_POINT('Ctrl Pts',(0.681252410513519,7.88401022670231,84.1146195152104));
#59570=CARTESIAN_POINT('Ctrl Pts',(0.87503691354045,7.86486795881519,84.106799417609));
#59571=CARTESIAN_POINT('Ctrl Pts',(1.0679762583037,7.83858072049396,84.0989793200076));
#59572=CARTESIAN_POINT('Ctrl Pts',(1.26080152720576,7.81230902456691,84.0911638460581));
#59573=CARTESIAN_POINT('Ctrl Pts',(1.45278228592922,7.7789008206446,84.0833483721087));
#59574=CARTESIAN_POINT('Ctrl Pts',(1.6433488114968,7.73843173283528,84.0755328981592));
#59575=CARTESIAN_POINT('Ctrl Pts',(1.8338396792044,7.69797871188014,84.0677205270738));
#59576=CARTESIAN_POINT('Ctrl Pts',(2.02291708901737,7.65047046517733,84.0599081559885));
#59577=CARTESIAN_POINT('Ctrl Pts',(2.21002014796113,7.5960339615885,84.0520957849031));
#59578=CARTESIAN_POINT('Ctrl Pts',(2.39711612438674,7.5415995186155,84.0442837095439));
#59579=CARTESIAN_POINT('Ctrl Pts',(2.58223755879231,7.48023743076533,84.0364716341847));
#59580=CARTESIAN_POINT('Ctrl Pts',(2.7648369391902,7.41212504614496,84.0286595588254));
#59581=CARTESIAN_POINT('Ctrl Pts',(2.94744166005093,7.34401066944959,84.0208472549873));
#59582=CARTESIAN_POINT('Ctrl Pts',(3.12752385005019,7.26914572494176,84.0130349511492));
#59583=CARTESIAN_POINT('Ctrl Pts',(3.30455429656338,7.18775638854466,84.0052226473111));
#59584=CARTESIAN_POINT('Ctrl Pts',(3.48162106973891,7.10635035104896,83.9974087403876));
#59585=CARTESIAN_POINT('Ctrl Pts',(3.65563453234891,7.01841740160396,83.9895948334642));
#59586=CARTESIAN_POINT('Ctrl Pts',(3.82608833512247,6.92423057471657,83.9817809265407));
#59587=CARTESIAN_POINT('Ctrl Pts',(3.9966071090415,6.83000784704005,83.9739640412237));
#59588=CARTESIAN_POINT('Ctrl Pts',(4.16356321280081,6.72952666356001,83.9661471559068));
#59589=CARTESIAN_POINT('Ctrl Pts',(4.32647750921442,6.62310451089682,83.9583302705899));
#59590=CARTESIAN_POINT('Ctrl Pts',(4.48956853317429,6.51656691271213,83.9505049056061));
#59591=CARTESIAN_POINT('Ctrl Pts',(4.64860869820649,6.40407566594995,83.9426795406223));
#59592=CARTESIAN_POINT('Ctrl Pts',(4.8031494704633,6.28599046804783,83.9348541756385));
#59593=CARTESIAN_POINT('Ctrl Pts',(4.95778416575485,6.16783350319396,83.9270240547446));
#59594=CARTESIAN_POINT('Ctrl Pts',(5.10791374803941,6.04407603479396,83.9191939338507));
#59595=CARTESIAN_POINT('Ctrl Pts',(5.25312500948118,5.91511611337963,83.9113638129568));
#59596=CARTESIAN_POINT('Ctrl Pts',(5.39853476509491,5.78597991229827,83.9035229888065));
#59597=CARTESIAN_POINT('Ctrl Pts',(5.53901251867156,5.65162729675949,83.8956821646562));
#59598=CARTESIAN_POINT('Ctrl Pts',(5.67418317873892,5.51249183710201,83.8878413405058));
#59599=CARTESIAN_POINT('Ctrl Pts',(5.74713413828386,5.43740109415764,83.8836096851666));
#59600=CARTESIAN_POINT('Ctrl Pts',(5.81854000132922,5.36091780652849,83.8793780298273));
#59601=CARTESIAN_POINT('Ctrl Pts',(5.88834694540054,5.2831137836121,83.875146374488));
#59602=CARTESIAN_POINT('Ctrl Pts',(6.01885258915522,5.13765742203531,83.867235200155));
#59603=CARTESIAN_POINT('Ctrl Pts',(6.14414076753762,4.98716696520392,83.859324025822));
#59604=CARTESIAN_POINT('Ctrl Pts',(6.26380039774366,4.83205190133823,83.851412851489));
#59605=CARTESIAN_POINT('Ctrl Pts',(6.3833303013745,4.67710500234118,83.8435102538961));
#59606=CARTESIAN_POINT('Ctrl Pts',(6.49724360253856,4.51754375337019,83.8356076563033));
#59607=CARTESIAN_POINT('Ctrl Pts',(6.60516680373139,4.3538135576624,83.8277050587104));
#59608=CARTESIAN_POINT('Ctrl Pts',(6.71299303572663,4.19023047384086,83.8198095616162));
#59609=CARTESIAN_POINT('Ctrl Pts',(6.81483970081807,4.02248619135834,83.811914064522));
#59610=CARTESIAN_POINT('Ctrl Pts',(6.91037409794283,3.85105840341078,83.8040185674278));
#59611=CARTESIAN_POINT('Ctrl Pts',(7.00584038558016,3.67975283174469,83.7961286992827));
#59612=CARTESIAN_POINT('Ctrl Pts',(7.09500320404474,3.50476928666504,83.7882388311377));
#59613=CARTESIAN_POINT('Ctrl Pts',(7.17757350195661,3.32661383752463,83.7803489629926));
#59614=CARTESIAN_POINT('Ctrl Pts',(7.26010025206162,3.14855234806811,83.7724632559861));
#59615=CARTESIAN_POINT('Ctrl Pts',(7.33604126518389,2.96732260008995,83.7645775489797));
#59616=CARTESIAN_POINT('Ctrl Pts',(7.40515360914334,2.78345487209535,83.7566918419732));
#59617=CARTESIAN_POINT('Ctrl Pts',(7.47424232329485,2.59965000926854,83.7488088311239));
#59618=CARTESIAN_POINT('Ctrl Pts',(7.53650690035275,2.41320928641171,83.7409258202746));
#59619=CARTESIAN_POINT('Ctrl Pts',(7.59175259082938,2.22468280876968,83.7330428094253));
#59620=CARTESIAN_POINT('Ctrl Pts',(7.64699910576532,2.03615351765192,83.7251596809339));
#59621=CARTESIAN_POINT('Ctrl Pts',(7.69522641974634,1.84553873806009,83.7172765524424));
#59622=CARTESIAN_POINT('Ctrl Pts',(7.73628953466395,1.65340413566952,83.7093934239509));
#59623=CARTESIAN_POINT('Ctrl Pts',(7.77735518855499,1.46125765340444,83.7015098080378));
#59624=CARTESIAN_POINT('Ctrl Pts',(7.81125568801351,1.26759149838078,83.6936261921246));
#59625=CARTESIAN_POINT('Ctrl Pts',(7.83789708277303,1.07298197555136,83.6857425762115));
#59626=CARTESIAN_POINT('Ctrl Pts',(7.86454460307338,0.878327706994834,83.6778571476526));
#59627=CARTESIAN_POINT('Ctrl Pts',(7.88392964603437,0.682729980179148,83.6699717190937));
#59628=CARTESIAN_POINT('Ctrl Pts',(7.89601007282437,0.486770921333764,83.6620862905347));
#59629=CARTESIAN_POINT('Ctrl Pts',(7.90809530789625,0.290733866370523,83.6541977233977));
#59630=CARTESIAN_POINT('Ctrl Pts',(7.91287011232309,0.0943355368062724,
83.6463091562606));
#59631=CARTESIAN_POINT('Ctrl Pts',(7.91034445603173,-0.101840988448166,
83.6384205891236));
#59632=CARTESIAN_POINT('Ctrl Pts',(7.90781611189303,-0.298226288171213,
83.6305236268363));
#59633=CARTESIAN_POINT('Ctrl Pts',(7.89797179308439,-0.494388967111445,
83.622626664549));
#59634=CARTESIAN_POINT('Ctrl Pts',(7.88087351197409,-0.689749003816036,
83.6147297022616));
#59635=CARTESIAN_POINT('Ctrl Pts',(7.86376480318697,-0.885228184153381,
83.6068279238779));
#59636=CARTESIAN_POINT('Ctrl Pts',(7.83939335506088,-1.07990340504673,83.5989261454941));
#59637=CARTESIAN_POINT('Ctrl Pts',(7.80787253438817,-1.27320363129659,83.5910243671104));
#59638=CARTESIAN_POINT('Ctrl Pts',(7.77631094641002,-1.4667538614867,83.5831123689986));
#59639=CARTESIAN_POINT('Ctrl Pts',(7.73758158461768,-1.65892520793903,83.5752003708869));
#59640=CARTESIAN_POINT('Ctrl Pts',(7.69184828925866,-1.84915951043403,83.5672883727751));
#59641=CARTESIAN_POINT('Ctrl Pts',(7.67268650849822,-1.92886572816683,83.5639733268769));
#59642=CARTESIAN_POINT('Ctrl Pts',(7.65229576417141,-2.00823210367551,83.5606582809786));
#59643=CARTESIAN_POINT('Ctrl Pts',(7.63069063770581,-2.08721857782766,83.5573432350803));
#59644=CARTESIAN_POINT('Ctrl Pts',(7.57913124618991,-2.27571525484348,83.5494320687359));
#59645=CARTESIAN_POINT('Ctrl Pts',(7.52051391840175,-2.46255367042699,83.5415209023915));
#59646=CARTESIAN_POINT('Ctrl Pts',(7.45496014546727,-2.64716645292558,83.533609736047));
#59647=CARTESIAN_POINT('Ctrl Pts',(7.38947743074717,-2.83157912101295,83.5257071451564));
#59648=CARTESIAN_POINT('Ctrl Pts',(7.31707336173238,-3.01377063936993,83.5178045542659));
#59649=CARTESIAN_POINT('Ctrl Pts',(7.23791997929484,-3.19318577181544,83.5099019633753));
#59650=CARTESIAN_POINT('Ctrl Pts',(7.15883770354123,-3.37243972839302,83.5020064717016));
#59651=CARTESIAN_POINT('Ctrl Pts',(7.07301833106893,-3.5489219540993,83.4941109800279));
#59652=CARTESIAN_POINT('Ctrl Pts',(6.98068314507643,-3.72209401117784,83.4862154883542));
#59653=CARTESIAN_POINT('Ctrl Pts',(6.88841377285106,-3.89514263637808,83.4783256243516));
#59654=CARTESIAN_POINT('Ctrl Pts',(6.78963800167896,-4.06488549062608,83.470435760349));
#59655=CARTESIAN_POINT('Ctrl Pts',(6.68462461307415,-4.23080545313576,83.4625458963463));
#59656=CARTESIAN_POINT('Ctrl Pts',(6.57966659188112,-4.39663793576303,83.4546601922071));
#59657=CARTESIAN_POINT('Ctrl Pts',(6.46847769047691,-4.55865125230619,83.4467744880678));
#59658=CARTESIAN_POINT('Ctrl Pts',(6.35137202397273,-4.71635393212771,83.4388887839285));
#59659=CARTESIAN_POINT('Ctrl Pts',(6.23430637750785,-4.87400271816569,83.4310057746733));
#59660=CARTESIAN_POINT('Ctrl Pts',(6.11132820122546,-5.02734352697304,83.423122765418));
#59661=CARTESIAN_POINT('Ctrl Pts',(5.98279437809521,-5.17591464665254,83.4152397561628));
#59662=CARTESIAN_POINT('Ctrl Pts',(5.85425860576046,-5.32448801940046,83.4073566273623));
#59663=CARTESIAN_POINT('Ctrl Pts',(5.72016723743268,-5.46829129220355,83.3994734985619));
#59664=CARTESIAN_POINT('Ctrl Pts',(5.58091718783104,-5.60689614158958,83.3915903697615));
#59665=CARTESIAN_POINT('Ctrl Pts',(5.44165850729581,-5.74550958191869,83.3837067523526));
#59666=CARTESIAN_POINT('Ctrl Pts',(5.29724075248069,-5.8789237129606,83.3758231349436));
#59667=CARTESIAN_POINT('Ctrl Pts',(5.14809743564973,-6.00674735552085,83.3679395175347));
#59668=CARTESIAN_POINT('Ctrl Pts',(4.99891980448622,-6.13460040726329,83.3600540862928));
#59669=CARTESIAN_POINT('Ctrl Pts',(4.84501470672823,-6.25686018301368,83.3521686550508));
#59670=CARTESIAN_POINT('Ctrl Pts',(4.68684861610154,-6.37317589979651,83.3442832238089));
#59671=CARTESIAN_POINT('Ctrl Pts',(4.52861954799558,-6.48953793036641,83.3363946528005));
#59672=CARTESIAN_POINT('Ctrl Pts',(4.36612638401809,-6.59995098178244,83.3285060817922));
#59673=CARTESIAN_POINT('Ctrl Pts',(4.19986462814982,-6.70410755471718,83.3206175107838));
#59674=CARTESIAN_POINT('Ctrl Pts',(4.03342589631608,-6.80837499626364,83.3127205428506));
#59675=CARTESIAN_POINT('Ctrl Pts',(3.86321085248997,-6.90637247412938,83.3048235749174));
#59676=CARTESIAN_POINT('Ctrl Pts',(3.68974062438688,-6.9978378892876,83.2969266069841));
#59677=CARTESIAN_POINT('Ctrl Pts',(3.5161645801288,-7.08935909798834,83.2890248219316));
#59678=CARTESIAN_POINT('Ctrl Pts',(3.33932970295774,-7.17434015126876,83.2811230368791));
#59679=CARTESIAN_POINT('Ctrl Pts',(3.15977738802902,-7.25256698404782,83.2732212518266));
#59680=CARTESIAN_POINT('Ctrl Pts',(2.97999281580384,-7.33089500601344,83.2653092455344));
#59681=CARTESIAN_POINT('Ctrl Pts',(2.79748410483198,-7.40245123103485,83.2573972392423));
#59682=CARTESIAN_POINT('Ctrl Pts',(2.61280917189454,-7.46707099412238,83.2494852329502));
#59683=CARTESIAN_POINT('Ctrl Pts',(2.53543235612082,-7.49414598163819,83.246170187191));
#59684=CARTESIAN_POINT('Ctrl Pts',(2.45767540044514,-7.52000387236544,83.2428551414317));
#59685=CARTESIAN_POINT('Ctrl Pts',(2.37957987550948,-7.54463522087518,83.2395400956725));
#59686=CARTESIAN_POINT('Ctrl Pts',(2.19487786588614,-7.60289028188194,83.2316997538063));
#59687=CARTESIAN_POINT('Ctrl Pts',(2.00775753756321,-7.65444626410038,83.2238594119401));
#59688=CARTESIAN_POINT('Ctrl Pts',(1.81875113205706,-7.69909509745406,83.2160190700738));
#59689=CARTESIAN_POINT('Ctrl Pts',(1.62995604133662,-7.74369401208341,83.2081874939431));
#59690=CARTESIAN_POINT('Ctrl Pts',(1.4392794108911,-7.78140107487166,83.2003559178124));
#59691=CARTESIAN_POINT('Ctrl Pts',(1.24727128131272,-7.81205704989489,83.1925243416816));
#59692=CARTESIAN_POINT('Ctrl Pts',(1.05544048784877,-7.84268471147377,83.1846999986888));
#59693=CARTESIAN_POINT('Ctrl Pts',(0.862280988958657,-7.86627419927192,
83.176875655696));
#59694=CARTESIAN_POINT('Ctrl Pts',(0.668355929292285,-7.88271662257244,
83.1690513127032));
#59695=CARTESIAN_POINT('Ctrl Pts',(0.474572288600763,-7.89914705530995,
83.1612326755772));
#59696=CARTESIAN_POINT('Ctrl Pts',(0.280024547811638,-7.90844077482352,
83.1534140384512));
#59697=CARTESIAN_POINT('Ctrl Pts',(0.0852841351561738,-7.91054028599126,
83.1455954013252));
#59698=CARTESIAN_POINT('Ctrl Pts',(-0.109352096408714,-7.91263867397475,
83.1377809469681));
#59699=CARTESIAN_POINT('Ctrl Pts',(-0.304180443843766,-7.90755051662476,
83.1299664926111));
#59700=CARTESIAN_POINT('Ctrl Pts',(-0.498626095695033,-7.89527029408696,
83.122152038254));
#59701=CARTESIAN_POINT('Ctrl Pts',(-0.693005490256475,-7.88299425603082,
83.1143402466696));
#59702=CARTESIAN_POINT('Ctrl Pts',(-0.88700209858081,-7.86353105783853,
83.1065284550851));
#59703=CARTESIAN_POINT('Ctrl Pts',(-1.08004265994247,-7.83692725835224,
83.0987166635007));
#59704=CARTESIAN_POINT('Ctrl Pts',(-1.27309225591602,-7.81032221376492,
83.0909045063118));
#59705=CARTESIAN_POINT('Ctrl Pts',(-1.46518536595255,-7.77657593916149,
83.0830923491228));
#59706=CARTESIAN_POINT('Ctrl Pts',(-1.65575487304225,-7.73578676027183,
83.0752801919339));
#59707=CARTESIAN_POINT('Ctrl Pts',(-1.84633995936271,-7.69499424682964,
83.067467396094));
#59708=CARTESIAN_POINT('Ctrl Pts',(-2.03540085035699,-7.64715775500881,
83.059654600254));
#59709=CARTESIAN_POINT('Ctrl Pts',(-2.22238171541002,-7.59242652325403,
83.0518418044141));
#59710=CARTESIAN_POINT('Ctrl Pts',(-2.40941076720844,-7.53768118674083,
83.0440269951425));
#59711=CARTESIAN_POINT('Ctrl Pts',(-2.59435838759789,-7.47603766936701,
83.0362121858709));
#59712=CARTESIAN_POINT('Ctrl Pts',(-2.77668482680089,-7.40769480827968,
83.0283973765992));
#59713=CARTESIAN_POINT('Ctrl Pts',(-2.95909033790246,-7.33932230804729,
83.0205791781768));
#59714=CARTESIAN_POINT('Ctrl Pts',(-3.13887207431502,-7.26424479973415,
83.0127609797542));
#59715=CARTESIAN_POINT('Ctrl Pts',(-3.31551100918296,-7.18270894217402,
83.0049427813318));
#59716=CARTESIAN_POINT('Ctrl Pts',(-3.49235555081547,-7.10107817731679,
82.9971154825686));
#59717=CARTESIAN_POINT('Ctrl Pts',(-3.66604966510608,-7.01297419616484,
82.9892881838055));
#59718=CARTESIAN_POINT('Ctrl Pts',(-3.83609867925429,-6.91868975478909,
82.9814608850423));
#59719=CARTESIAN_POINT('Ctrl Pts',(-4.00625870209264,-6.82434376414538,
82.9736284765866));
#59720=CARTESIAN_POINT('Ctrl Pts',(-4.17276858281325,-6.7238094540847,82.9657960681309));
#59721=CARTESIAN_POINT('Ctrl Pts',(-4.33516327038756,-6.61742249059878,
82.9579636596752));
#59722=CARTESIAN_POINT('Ctrl Pts',(-4.49779101722459,-6.5108828468273,82.9501200106095));
#59723=CARTESIAN_POINT('Ctrl Pts',(-4.6562914895126,-6.3984739763138,82.9422763615439));
#59724=CARTESIAN_POINT('Ctrl Pts',(-4.81023238443817,-6.2805720605453,82.9344327124782));
#59725=CARTESIAN_POINT('Ctrl Pts',(-4.89328879763165,-6.21695991747503,
82.9302007937405));
#59726=CARTESIAN_POINT('Ctrl Pts',(-4.97501855115026,-6.15174941395189,
82.9259688750027));
#59727=CARTESIAN_POINT('Ctrl Pts',(-5.05535833089065,-6.08500395614453,
82.921736956265));
#59728=CARTESIAN_POINT('Ctrl Pts',(-5.20399385829731,-5.96151909776858,
82.9139075413031));
#59729=CARTESIAN_POINT('Ctrl Pts',(-5.34833352264433,-5.83239276955187,
82.9060781263413));
#59730=CARTESIAN_POINT('Ctrl Pts',(-5.48791468024828,-5.69795695511255,
82.8982487113795));
#59731=CARTESIAN_POINT('Ctrl Pts',(-5.62733478723547,-5.56367625452385,
82.890428330102));
#59732=CARTESIAN_POINT('Ctrl Pts',(-5.76200706819059,-5.42409850837976,
82.8826079488245));
#59733=CARTESIAN_POINT('Ctrl Pts',(-5.8915001616145,-5.27959722381322,82.8747875675469));
#59734=CARTESIAN_POINT('Ctrl Pts',(-6.02086927695928,-5.13523428632929,
82.8669746735865));
#59735=CARTESIAN_POINT('Ctrl Pts',(-6.14506884560285,-4.98595745894551,
82.859161779626));
#59736=CARTESIAN_POINT('Ctrl Pts',(-6.26370262716065,-4.83217863892684,
82.8513488856655));
#59737=CARTESIAN_POINT('Ctrl Pts',(-6.38224611130333,-4.67851686676558,
82.843541938444));
#59738=CARTESIAN_POINT('Ctrl Pts',(-6.49523203143791,-4.52036020543207,
82.8357349912225));
#59739=CARTESIAN_POINT('Ctrl Pts',(-6.60230278563192,-4.35815545005418,
82.827928044001));
#59740=CARTESIAN_POINT('Ctrl Pts',(-6.70931260165946,-4.19604301176569,
82.8201255400194));
#59741=CARTESIAN_POINT('Ctrl Pts',(-6.81041376450384,-4.02988736331785,
82.8123230360378));
#59742=CARTESIAN_POINT('Ctrl Pts',(-6.90529047660876,-3.8601663738311,82.8045205320562));
#59743=CARTESIAN_POINT('Ctrl Pts',(-7.00013829400394,-3.69049707288436,
82.7967204043277));
#59744=CARTESIAN_POINT('Ctrl Pts',(-7.08876526282641,-3.51726490078991,
82.7889202765993));
#59745=CARTESIAN_POINT('Ctrl Pts',(-7.17090011100932,-3.34097479755932,
82.7811201488709));
#59746=CARTESIAN_POINT('Ctrl Pts',(-7.25302453423391,-3.16470706993443,
82.773321011173));
#59747=CARTESIAN_POINT('Ctrl Pts',(-7.3286583287584,-2.98538250430967,82.765521873475));
#59748=CARTESIAN_POINT('Ctrl Pts',(-7.39757714600128,-2.80352873517636,
82.7577227357771));
#59749=CARTESIAN_POINT('Ctrl Pts',(-7.46649945756484,-2.62166574569638,
82.7499232026475));
#59750=CARTESIAN_POINT('Ctrl Pts',(-7.52870598929783,-2.43727362793176,
82.7421236695178));
#59751=CARTESIAN_POINT('Ctrl Pts',(-7.58402127213157,-2.25089811938608,
82.7343241363882));
#59752=CARTESIAN_POINT('Ctrl Pts',(-7.63937274340732,-2.0644006799935,82.726519500637));
#59753=CARTESIAN_POINT('Ctrl Pts',(-7.68782385647299,-1.87591759612322,
82.7187148648858));
#59754=CARTESIAN_POINT('Ctrl Pts',(-7.72924936756948,-1.68600866365711,
82.7109102291347));
#59755=CARTESIAN_POINT('Ctrl Pts',(-7.7706883216808,-1.4960381037414,82.703103060697));
#59756=CARTESIAN_POINT('Ctrl Pts',(-7.80509706483003,-1.30464112026713,
82.6952958922593));
#59757=CARTESIAN_POINT('Ctrl Pts',(-7.83240185020259,-1.11238583995981,
82.6874887238215));
#59758=CARTESIAN_POINT('Ctrl Pts',(-7.85973685435271,-0.919917786709097,
82.6796729150271));
#59759=CARTESIAN_POINT('Ctrl Pts',(-7.87995215144126,-0.726589889817072,
82.6718571062327));
#59760=CARTESIAN_POINT('Ctrl Pts',(-7.89302597221011,-0.532974672959839,
82.6640412974382));
#59761=CARTESIAN_POINT('Ctrl Pts',(-7.90503736302606,-0.355093388008408,
82.656860631921));
#59762=CARTESIAN_POINT('Ctrl Pts',(-7.91102139961202,-0.176969816629341,
82.6496799664038));
#59763=CARTESIAN_POINT('Ctrl Pts',(-7.91099994247235,0.000954045336348954,
82.6424993008866));
#59764=CARTESIAN_POINT('',(-7.91099999409123,-0.000305758797192468,78.6348799381992));
#59765=CARTESIAN_POINT('Ctrl Pts',(-7.91099993152671,0.00104085748967774,
82.6449938270835));
#59766=CARTESIAN_POINT('Ctrl Pts',(-7.91095410811255,0.349320069428504,
82.6327410013806));
#59767=CARTESIAN_POINT('Ctrl Pts',(-7.88790906178625,0.697220106659238,
82.6200633058441));
#59768=CARTESIAN_POINT('Ctrl Pts',(-7.84031239578766,1.0552673544758,82.6056534138883));
#59769=CARTESIAN_POINT('Ctrl Pts',(-7.83857994710769,1.06805995277639,82.605136902858));
#59770=CARTESIAN_POINT('Ctrl Pts',(-7.8358192623798,1.0880766201622,82.6043261674288));
#59771=CARTESIAN_POINT('Ctrl Pts',(-7.83481232507473,1.09530364481255,82.6040329310423));
#59772=CARTESIAN_POINT('Ctrl Pts',(-7.83310538536042,1.1074319547877,82.6035399628812));
#59773=CARTESIAN_POINT('Ctrl Pts',(-7.83241077663093,1.11233400496469,82.6033404772588));
#59774=CARTESIAN_POINT('Ctrl Pts',(-7.83103186182475,1.12200006380831,82.6029466609751));
#59775=CARTESIAN_POINT('Ctrl Pts',(-7.83034780909842,1.12676410685477,82.6027523418164));
#59776=CARTESIAN_POINT('Ctrl Pts',(-7.82903972718962,1.13581544294007,82.6023827317705));
#59777=CARTESIAN_POINT('Ctrl Pts',(-7.82841652253502,1.14010285497647,82.6022074777285));
#59778=CARTESIAN_POINT('Ctrl Pts',(-7.82699214290545,1.14984581568054,82.6018088184936));
#59779=CARTESIAN_POINT('Ctrl Pts',(-7.8261887859552,1.15530103925643,82.601585316975));
#59780=CARTESIAN_POINT('Ctrl Pts',(-7.82410022827398,1.16938131561839,82.6010077129413));
#59781=CARTESIAN_POINT('Ctrl Pts',(-7.82280647093958,1.17800507670697,82.600653237421));
#59782=CARTESIAN_POINT('Ctrl Pts',(-7.81504522389425,1.22916234804201,82.5985462948037));
#59783=CARTESIAN_POINT('Ctrl Pts',(-7.80824519577419,1.27164412977541,82.5967796408973));
#59784=CARTESIAN_POINT('Ctrl Pts',(-7.74055447517696,1.67349709365284,82.5799189930328));
#59785=CARTESIAN_POINT('Ctrl Pts',(-7.6552444295412,2.02829509620599,82.5639209969348));
#59786=CARTESIAN_POINT('Ctrl Pts',(-7.53364049099852,2.41450153487727,82.5459902384341));
#59787=CARTESIAN_POINT('Ctrl Pts',(-7.52119826841894,2.45298457133671,82.5441974417473));
#59788=CARTESIAN_POINT('Ctrl Pts',(-7.31680728128888,3.06897560740725,82.5154133272331));
#59789=CARTESIAN_POINT('Ctrl Pts',(-7.05912230764937,3.62259623559259,82.4885337622097));
#59790=CARTESIAN_POINT('Ctrl Pts',(-6.67075725325308,4.25472275394273,82.4577336694805));
#59791=CARTESIAN_POINT('Ctrl Pts',(-6.59816353232833,4.36645251706056,82.4522747302298));
#59792=CARTESIAN_POINT('Ctrl Pts',(-6.50698590993662,4.49931490619557,82.4457558860335));
#59793=CARTESIAN_POINT('Ctrl Pts',(-6.4910688198935,4.52224787537569,82.4446296545503));
#59794=CARTESIAN_POINT('Ctrl Pts',(-6.46775471402853,4.55546159448804,82.442996879238));
#59795=CARTESIAN_POINT('Ctrl Pts',(-6.46045392627537,4.56580950625715,82.442487943421));
#59796=CARTESIAN_POINT('Ctrl Pts',(-6.44763347937972,4.58388849668556,82.441598342086));
#59797=CARTESIAN_POINT('Ctrl Pts',(-6.44212469200145,4.59162723744189,82.441217407596));
#59798=CARTESIAN_POINT('Ctrl Pts',(-6.43145803269192,4.60655477069941,82.4404823318367));
#59799=CARTESIAN_POINT('Ctrl Pts',(-6.4263020124273,4.61374487019525,82.4401281456488));
#59800=CARTESIAN_POINT('Ctrl Pts',(-6.41408181961623,4.63072577172773,82.4392913653364));
#59801=CARTESIAN_POINT('Ctrl Pts',(-6.40700726891939,4.64050909047417,82.4388090317134));
#59802=CARTESIAN_POINT('Ctrl Pts',(-6.38220596218085,4.67464171673893,82.4371254101558));
#59803=CARTESIAN_POINT('Ctrl Pts',(-6.36436250542876,4.69890604717129,82.435927076478));
#59804=CARTESIAN_POINT('Ctrl Pts',(-6.11820406375286,5.02966885131248,82.4195708628429));
#59805=CARTESIAN_POINT('Ctrl Pts',(-5.86810265449696,5.31934104552486,82.4050343347008));
#59806=CARTESIAN_POINT('Ctrl Pts',(-5.42488588443359,5.76320895976115,82.3818462421943));
#59807=CARTESIAN_POINT('Ctrl Pts',(-5.24378071055835,5.92846786234193,82.3729589097175));
#59808=CARTESIAN_POINT('Ctrl Pts',(-4.98502196560202,6.14343746088104,82.3607908954917));
#59809=CARTESIAN_POINT('Ctrl Pts',(-4.91374205154513,6.20059729883503,82.3574899009976));
#59810=CARTESIAN_POINT('Ctrl Pts',(-4.65517115362206,6.40068776760248,82.345654461163));
#59811=CARTESIAN_POINT('Ctrl Pts',(-4.46251075846352,6.53646808519185,82.3370937673916));
#59812=CARTESIAN_POINT('Ctrl Pts',(-4.1277686526447,6.75067687240102,82.3222593284048));
#59813=CARTESIAN_POINT('Ctrl Pts',(-3.98881273478963,6.83370189781156,82.3161110370332));
#59814=CARTESIAN_POINT('Ctrl Pts',(-3.80805868169157,6.93430881401271,82.308019196914));
#59815=CARTESIAN_POINT('Ctrl Pts',(-3.76851769623517,6.9558769338767,82.3062434169424));
#59816=CARTESIAN_POINT('Ctrl Pts',(-3.70473674296157,6.98996357603652,82.3033670011697));
#59817=CARTESIAN_POINT('Ctrl Pts',(-3.68061213539441,7.00269658145944,82.3022762865488));
#59818=CARTESIAN_POINT('Ctrl Pts',(-3.65127064892156,7.0179895553017,82.300945890571));
#59819=CARTESIAN_POINT('Ctrl Pts',(-3.64611598531127,7.02066898318087,82.300712026446));
#59820=CARTESIAN_POINT('Ctrl Pts',(-3.63709290071563,7.02534662412765,82.3003023982281));
#59821=CARTESIAN_POINT('Ctrl Pts',(-3.63322576852647,7.02734732828695,82.3001267567561));
#59822=CARTESIAN_POINT('Ctrl Pts',(-3.62544207191943,7.0313661685012,82.2997730599499));
#59823=CARTESIAN_POINT('Ctrl Pts',(-3.6215254693127,7.03338422719767,82.2995950008692));
#59824=CARTESIAN_POINT('Ctrl Pts',(-3.61399856992614,7.03725456423063,82.2992526399619));
#59825=CARTESIAN_POINT('Ctrl Pts',(-3.61038852870959,7.03910733949198,82.2990883630479));
#59826=CARTESIAN_POINT('Ctrl Pts',(-3.60189258473144,7.04345944311424,82.2987015725752));
#59827=CARTESIAN_POINT('Ctrl Pts',(-3.59700550815519,7.04595646401543,82.2984789429059));
#59828=CARTESIAN_POINT('Ctrl Pts',(-3.58016239491584,7.05454025588007,82.2977111708477));
#59829=CARTESIAN_POINT('Ctrl Pts',(-3.56819352276807,7.06060167241029,82.2971647390002));
#59830=CARTESIAN_POINT('Ctrl Pts',(-3.40576436646243,7.1423424558724,82.2897369962797));
#59831=CARTESIAN_POINT('Ctrl Pts',(-3.25296393131615,7.21321691824653,82.2825836462355));
#59832=CARTESIAN_POINT('Ctrl Pts',(-2.94790826134799,7.34304961336763,82.2681025797864));
#59833=CARTESIAN_POINT('Ctrl Pts',(-2.79584831437437,7.40228133953197,82.2607973658941));
#59834=CARTESIAN_POINT('Ctrl Pts',(-2.41032368413647,7.53887992847459,82.2422404171352));
#59835=CARTESIAN_POINT('Ctrl Pts',(-2.17487643449026,7.61014324717112,82.230878467541));
#59836=CARTESIAN_POINT('Ctrl Pts',(-1.90660174055661,7.67787350055613,82.2181281060756));
#59837=CARTESIAN_POINT('Ctrl Pts',(-1.87666264549439,7.68524619038826,82.2167078085039));
#59838=CARTESIAN_POINT('Ctrl Pts',(-1.81218739967203,7.70072439578925,82.2136554823284));
#59839=CARTESIAN_POINT('Ctrl Pts',(-1.77763824057219,7.70877303385118,82.2120237930571));
#59840=CARTESIAN_POINT('Ctrl Pts',(-1.70287219656382,7.72566131299856,82.2085021950472));
#59841=CARTESIAN_POINT('Ctrl Pts',(-1.66263799748794,7.73441991057805,82.2066129895662));
#59842=CARTESIAN_POINT('Ctrl Pts',(-1.57495953243013,7.75279089423254,82.20251033634));
#59843=CARTESIAN_POINT('Ctrl Pts',(-1.52749159201165,7.76228276113119,82.2002982916322));
#59844=CARTESIAN_POINT('Ctrl Pts',(-1.3224718239828,7.80132581797672,82.1907877401182));
#59845=CARTESIAN_POINT('Ctrl Pts',(-1.16412556602665,7.82652097633264,82.183553830554));
#59846=CARTESIAN_POINT('Ctrl Pts',(-0.829913214686822,7.86933070682043,
82.1685803218436));
#59847=CARTESIAN_POINT('Ctrl Pts',(-0.653999002608167,7.88589955955905,
82.1608688060668));
#59848=CARTESIAN_POINT('Ctrl Pts',(-0.301288779858691,7.90723531783254,
82.1457861087256));
#59849=CARTESIAN_POINT('Ctrl Pts',(-0.124592729063699,7.91199262744486,
82.1384193394991));
#59850=CARTESIAN_POINT('Ctrl Pts',(0.0837537802743487,7.91061987934015,
82.1299555262898));
#59851=CARTESIAN_POINT('Ctrl Pts',(0.115383602226224,7.91022175582863,82.1286765980149));
#59852=CARTESIAN_POINT('Ctrl Pts',(0.157109611807178,7.90944622577944,82.1269972528528));
#59853=CARTESIAN_POINT('Ctrl Pts',(0.167208445084067,7.90923917741232,82.1265914093773));
#59854=CARTESIAN_POINT('Ctrl Pts',(0.183733645094483,7.9088687099825,82.125928292224));
#59855=CARTESIAN_POINT('Ctrl Pts',(0.190160243090846,7.90871679896842,82.1256706515571));
#59856=CARTESIAN_POINT('Ctrl Pts',(0.202573040155221,7.90840824833334,82.1251734945852));
#59857=CARTESIAN_POINT('Ctrl Pts',(0.208559259209332,7.90825264483315,82.1249339453727));
#59858=CARTESIAN_POINT('Ctrl Pts',(0.222321433810788,7.90787927909634,82.1243837103068));
#59859=CARTESIAN_POINT('Ctrl Pts',(0.230097262210041,7.90765684403865,82.124073173937));
#59860=CARTESIAN_POINT('Ctrl Pts',(0.250812185412887,7.90703369335008,82.1232468407919));
#59861=CARTESIAN_POINT('Ctrl Pts',(0.26375067119878,7.90661268595191,82.1227316929069));
#59862=CARTESIAN_POINT('Ctrl Pts',(0.305369780605691,7.90515616184067,82.1210777433349));
#59863=CARTESIAN_POINT('Ctrl Pts',(0.334045972032011,7.90399632825828,82.1199429182862));
#59864=CARTESIAN_POINT('Ctrl Pts',(0.874073467301036,7.87921027005688,82.0986602074372));
#59865=CARTESIAN_POINT('Ctrl Pts',(1.3819583440441,7.8061659753496,82.0802488480511));
#59866=CARTESIAN_POINT('Ctrl Pts',(2.15421160008185,7.61730952218602,82.0528403729028));
#59867=CARTESIAN_POINT('Ctrl Pts',(2.42534357515986,7.53536604268906,82.0433097326995));
#59868=CARTESIAN_POINT('Ctrl Pts',(2.99689470121121,7.32857547383105,82.0226135272198));
#59869=CARTESIAN_POINT('Ctrl Pts',(3.29518107289733,7.19938578169494,82.0114331868785));
#59870=CARTESIAN_POINT('Ctrl Pts',(3.70359435723555,6.99178863742319,81.9945814472455));
#59871=CARTESIAN_POINT('Ctrl Pts',(3.82097006817931,6.92834065138982,81.9895466769319));
#59872=CARTESIAN_POINT('Ctrl Pts',(3.96840654540199,6.84375688820602,81.982907472444));
#59873=CARTESIAN_POINT('Ctrl Pts',(4.00000589031312,6.82533601028318,81.9814656651118));
#59874=CARTESIAN_POINT('Ctrl Pts',(4.04394021224102,6.79931455506815,81.979433068216));
#59875=CARTESIAN_POINT('Ctrl Pts',(4.05638415891133,6.79189799754665,81.978854199899));
#59876=CARTESIAN_POINT('Ctrl Pts',(4.07788924572791,6.77900084381976,81.9778482342665));
#59877=CARTESIAN_POINT('Ctrl Pts',(4.08695991682346,6.77353613536682,81.9774221974106));
#59878=CARTESIAN_POINT('Ctrl Pts',(4.09994029212038,6.76568042429072,81.9768100090196));
#59879=CARTESIAN_POINT('Ctrl Pts',(4.103858967697,6.76330419067953,81.9766248644763));
#59880=CARTESIAN_POINT('Ctrl Pts',(4.11061535042323,6.75919917461946,81.9763050750291));
#59881=CARTESIAN_POINT('Ctrl Pts',(4.11345403030612,6.75747201117102,81.9761705413588));
#59882=CARTESIAN_POINT('Ctrl Pts',(4.1189039063083,6.7541513877057,81.9759119197916));
#59883=CARTESIAN_POINT('Ctrl Pts',(4.12151526368354,6.75255820327548,81.9757878509932));
#59884=CARTESIAN_POINT('Ctrl Pts',(4.12765789835115,6.74880570225403,81.9754956599812));
#59885=CARTESIAN_POINT('Ctrl Pts',(4.13118840324481,6.74664512994146,81.9753274519744));
#59886=CARTESIAN_POINT('Ctrl Pts',(4.14334745438269,6.73919100085089,81.9747472180452));
#59887=CARTESIAN_POINT('Ctrl Pts',(4.15196750299662,6.7338836733282,81.9743342584221));
#59888=CARTESIAN_POINT('Ctrl Pts',(4.24571417215149,6.67591580603044,81.9698258428693));
#59889=CARTESIAN_POINT('Ctrl Pts',(4.32984089714907,6.62166269762062,81.9656245351131));
#59890=CARTESIAN_POINT('Ctrl Pts',(4.53171736565351,6.48598098442369,81.9552078245128));
#59891=CARTESIAN_POINT('Ctrl Pts',(4.64832868325318,6.40292500012817,81.9489054984122));
#59892=CARTESIAN_POINT('Ctrl Pts',(4.90792516191172,6.20719814018196,81.9343374883738));
#59893=CARTESIAN_POINT('Ctrl Pts',(5.04940558820169,6.09266260456133,81.9260079742405));
#59894=CARTESIAN_POINT('Ctrl Pts',(5.5297986120203,5.67552586657647,81.896665140721));
#59895=CARTESIAN_POINT('Ctrl Pts',(5.84652500511829,5.34868736937799,81.8754335022059));
#59896=CARTESIAN_POINT('Ctrl Pts',(6.1833718575868,4.93518793006913,81.8515965513555));
#59897=CARTESIAN_POINT('Ctrl Pts',(6.23236844565009,4.87316646557918,81.8480914667673));
#59898=CARTESIAN_POINT('Ctrl Pts',(6.35058417694355,4.71882539065852,81.839545740501));
#59899=CARTESIAN_POINT('Ctrl Pts',(6.41872967928759,4.62570461524448,81.8345412191565));
#59900=CARTESIAN_POINT('Ctrl Pts',(6.56249727213864,4.41994852158946,81.8238169689341));
#59901=CARTESIAN_POINT('Ctrl Pts',(6.63730918255846,4.30679052976544,81.818127790235));
#59902=CARTESIAN_POINT('Ctrl Pts',(6.74620071198438,4.13250277755704,81.8096762095788));
#59903=CARTESIAN_POINT('Ctrl Pts',(6.78243791215391,4.07275576964116,81.8068324143941));
#59904=CARTESIAN_POINT('Ctrl Pts',(6.82452177268674,4.00124918917944,81.8034909722707));
#59905=CARTESIAN_POINT('Ctrl Pts',(6.83113607104152,3.98994642581898,81.8029646240616));
#59906=CARTESIAN_POINT('Ctrl Pts',(6.8412715600567,3.97252743811785,81.8021562414801));
#59907=CARTESIAN_POINT('Ctrl Pts',(6.84481266796036,3.96642286524181,81.8018734647728));
#59908=CARTESIAN_POINT('Ctrl Pts',(6.85125020235128,3.9552908021355,81.8013587580069));
#59909=CARTESIAN_POINT('Ctrl Pts',(6.85414927366205,3.95026485178207,81.8011267296217));
#59910=CARTESIAN_POINT('Ctrl Pts',(6.86045186064145,3.93931059911893,81.8006217829872));
#59911=CARTESIAN_POINT('Ctrl Pts',(6.86385322853061,3.93338106290382,81.8003489446296));
#59912=CARTESIAN_POINT('Ctrl Pts',(6.87308674181776,3.91723601658111,81.7996073824649));
#59913=CARTESIAN_POINT('Ctrl Pts',(6.87890380579557,3.90701187640129,81.7991392180383));
#59914=CARTESIAN_POINT('Ctrl Pts',(6.9064701849403,3.85830847211923,81.7969159116814));
#59915=CARTESIAN_POINT('Ctrl Pts',(6.92791976770768,3.81965999222267,81.7951718547462));
#59916=CARTESIAN_POINT('Ctrl Pts',(7.26051732100637,3.20835687556068,81.7678973235601));
#59917=CARTESIAN_POINT('Ctrl Pts',(7.50005253087681,2.59960697854877,81.7453148272109));
#59918=CARTESIAN_POINT('Ctrl Pts',(7.74077814414052,1.66251646614667,81.7122072572788));
#59919=CARTESIAN_POINT('Ctrl Pts',(7.80095448329226,1.35229551315584,81.701442421204));
#59920=CARTESIAN_POINT('Ctrl Pts',(7.86159249353426,0.894737971947177,81.6849281755559));
#59921=CARTESIAN_POINT('Ctrl Pts',(7.87675082844901,0.749657155091485,81.6795977920532));
#59922=CARTESIAN_POINT('Ctrl Pts',(7.89423124280928,0.521466039641838,81.6709572232594));
#59923=CARTESIAN_POINT('Ctrl Pts',(7.89926886042242,0.438593681160197,81.6677662677672));
#59924=CARTESIAN_POINT('Ctrl Pts',(7.90500286083162,0.311180342830223,81.6627586655194));
#59925=CARTESIAN_POINT('Ctrl Pts',(7.90662899877267,0.266685518775396,81.6609909131456));
#59926=CARTESIAN_POINT('Ctrl Pts',(7.90809181614032,0.214620639765248,81.6588977602746));
#59927=CARTESIAN_POINT('Ctrl Pts',(7.90829336875327,0.207060824881036,81.6585932267067));
#59928=CARTESIAN_POINT('Ctrl Pts',(7.90858665969487,0.195434367222767,81.6581239265766));
#59929=CARTESIAN_POINT('Ctrl Pts',(7.90868610189198,0.19136793727716,81.6579596077544));
#59930=CARTESIAN_POINT('Ctrl Pts',(7.90886177919013,0.183949982951515,81.6576595360611));
#59931=CARTESIAN_POINT('Ctrl Pts',(7.9089390203217,0.180598480971753,81.6575238407844));
#59932=CARTESIAN_POINT('Ctrl Pts',(7.90910144913942,0.173350672660625,81.6572301341967));
#59933=CARTESIAN_POINT('Ctrl Pts',(7.90918588800026,0.169454352100039,81.6570720803693));
#59934=CARTESIAN_POINT('Ctrl Pts',(7.90940704302016,0.158889024909371,81.656643064766));
#59935=CARTESIAN_POINT('Ctrl Pts',(7.90953820336808,0.152219917756961,81.6563717899213));
#59936=CARTESIAN_POINT('Ctrl Pts',(7.91011513058217,0.120867959138215,81.6550943282579));
#59937=CARTESIAN_POINT('Ctrl Pts',(7.9104537891038,0.0961835106746757,81.6540821916067));
#59938=CARTESIAN_POINT('Ctrl Pts',(7.91399145912493,-0.295230367590466,
81.6379368962473));
#59939=CARTESIAN_POINT('Ctrl Pts',(7.89179994655053,-0.661715260893554,
81.6214970964371));
#59940=CARTESIAN_POINT('Ctrl Pts',(7.77738821514561,-1.53704646598482,81.5810738179645));
#59941=CARTESIAN_POINT('Ctrl Pts',(7.66057470335867,-2.04106300048223,81.5569111373424));
#59942=CARTESIAN_POINT('Ctrl Pts',(7.43576308455397,-2.70707035110996,81.5256533045396));
#59943=CARTESIAN_POINT('Ctrl Pts',(7.3697813278697,-2.88186249507884,81.5175034262463));
#59944=CARTESIAN_POINT('Ctrl Pts',(7.2516506401699,-3.16412607353471,81.50446478609));
#59945=CARTESIAN_POINT('Ctrl Pts',(7.20314902896742,-3.27303780911606,81.4994641214581));
#59946=CARTESIAN_POINT('Ctrl Pts',(7.11809171708981,-3.45297878506476,81.4912528491654));
#59947=CARTESIAN_POINT('Ctrl Pts',(7.08288946110985,-3.52462332043045,81.4879971489856));
#59948=CARTESIAN_POINT('Ctrl Pts',(7.04025243632213,-3.60817989743418,81.4842149562247));
#59949=CARTESIAN_POINT('Ctrl Pts',(7.03386357397253,-3.620618699161,81.4836523010286));
#59950=CARTESIAN_POINT('Ctrl Pts',(7.02403480044597,-3.63963063493679,81.4827928981793));
#59951=CARTESIAN_POINT('Ctrl Pts',(7.02061858347789,-3.64621594839851,81.4824953269814));
#59952=CARTESIAN_POINT('Ctrl Pts',(7.01437810045636,-3.6582042086026,81.4819538046204));
#59953=CARTESIAN_POINT('Ctrl Pts',(7.01155684438841,-3.66360871083721,81.4817097488941));
#59954=CARTESIAN_POINT('Ctrl Pts',(7.00545121895645,-3.67527198693532,81.481183212731));
#59955=CARTESIAN_POINT('Ctrl Pts',(7.0021647020214,-3.68152963389216,81.480900807466));
#59956=CARTESIAN_POINT('Ctrl Pts',(6.99325151252046,-3.69844555732297,81.4801376514594));
#59957=CARTESIAN_POINT('Ctrl Pts',(6.98760885257729,-3.70909541301738,81.4796574593718));
#59958=CARTESIAN_POINT('Ctrl Pts',(6.96117166444038,-3.75871804512183,81.4774212610621));
#59959=CARTESIAN_POINT('Ctrl Pts',(6.94007509879729,-3.79752945829967,81.4756758415387));
#59960=CARTESIAN_POINT('Ctrl Pts',(6.60228843886009,-4.40673960485565,81.4483290604531));
#59961=CARTESIAN_POINT('Ctrl Pts',(6.21657185626718,-4.93597740523132,81.4255674108692));
#59962=CARTESIAN_POINT('Ctrl Pts',(5.39617753006396,-5.81069224921571,81.384051081077));
#59963=CARTESIAN_POINT('Ctrl Pts',(4.98183974493874,-6.16960362719655,81.3652417160758));
#59964=CARTESIAN_POINT('Ctrl Pts',(4.52238692721028,-6.49092706742245,81.3429133278599));
#59965=CARTESIAN_POINT('Ctrl Pts',(4.51087206895067,-6.49893459631084,81.3423528163554));
#59966=CARTESIAN_POINT('Ctrl Pts',(4.49076066454459,-6.51284103531373,81.3413721476225));
#59967=CARTESIAN_POINT('Ctrl Pts',(4.48217361027547,-6.51875367098348,81.3409528890094));
#59968=CARTESIAN_POINT('Ctrl Pts',(4.46972587013052,-6.527288366993,81.340344319096));
#59969=CARTESIAN_POINT('Ctrl Pts',(4.4658744831024,-6.52992403332532,81.3401559121244));
#59970=CARTESIAN_POINT('Ctrl Pts',(4.45912744427861,-6.53453255502487,81.3398256508177));
#59971=CARTESIAN_POINT('Ctrl Pts',(4.45623280413449,-6.53650690142316,81.339683896082));
#59972=CARTESIAN_POINT('Ctrl Pts',(4.45064438721672,-6.54031315388104,81.3394100965607));
#59973=CARTESIAN_POINT('Ctrl Pts',(4.44795079405254,-6.54214531678457,81.3392780698327));
#59974=CARTESIAN_POINT('Ctrl Pts',(4.44155164910195,-6.54649219072924,81.3389642825131));
#59975=CARTESIAN_POINT('Ctrl Pts',(4.43784509576301,-6.54900541768312,81.3387824231388));
#59976=CARTESIAN_POINT('Ctrl Pts',(4.4267384622008,-6.55652250718289,81.3382371735094));
#59977=CARTESIAN_POINT('Ctrl Pts',(4.41933206190127,-6.56151696830178,81.3378731641488));
#59978=CARTESIAN_POINT('Ctrl Pts',(4.34917346643827,-6.60865531771014,81.3344212421775));
#59979=CARTESIAN_POINT('Ctrl Pts',(4.28583049611086,-6.64990911498071,81.3312761720035));
#59980=CARTESIAN_POINT('Ctrl Pts',(4.12386226779007,-6.75211982522031,81.3231831251911));
#59981=CARTESIAN_POINT('Ctrl Pts',(4.02447166577212,-6.81182706739457,81.3181699788015));
#59982=CARTESIAN_POINT('Ctrl Pts',(3.83491235761234,-6.92010471198551,81.3085740730283));
#59983=CARTESIAN_POINT('Ctrl Pts',(3.74504054400367,-6.96915148181296,81.3040103501888));
#59984=CARTESIAN_POINT('Ctrl Pts',(3.06456111211367,-7.32355321466,81.2694837001809));
#59985=CARTESIAN_POINT('Ctrl Pts',(2.43841449632265,-7.55514848936832,81.2381622509165));
#59986=CARTESIAN_POINT('Ctrl Pts',(1.59277945183619,-7.75166147393109,81.2003219684324));
#59987=CARTESIAN_POINT('Ctrl Pts',(1.39316952355342,-7.79001209403564,81.1916719248529));
#59988=CARTESIAN_POINT('Ctrl Pts',(1.10158562245328,-7.83446548302403,81.1794604986999));
#59989=CARTESIAN_POINT('Ctrl Pts',(1.01064148290011,-7.84671554332603,81.175710527792));
#59990=CARTESIAN_POINT('Ctrl Pts',(0.905091670906483,-7.85906741221714,
81.1714246899081));
#59991=CARTESIAN_POINT('Ctrl Pts',(0.89067595719092,-7.86071420830755,81.1708407684653));
#59992=CARTESIAN_POINT('Ctrl Pts',(0.868772239969556,-7.86315537767869,
81.1699556926036));
#59993=CARTESIAN_POINT('Ctrl Pts',(0.861287535167033,-7.86397873093686,
81.1696536356744));
#59994=CARTESIAN_POINT('Ctrl Pts',(0.84773398997766,-7.86545010362807,81.1691073499916));
#59995=CARTESIAN_POINT('Ctrl Pts',(0.841665558142616,-7.86610178798091,
81.1688630072369));
#59996=CARTESIAN_POINT('Ctrl Pts',(0.829545608937983,-7.86738915444406,
81.1683755003018));
#59997=CARTESIAN_POINT('Ctrl Pts',(0.823494100307288,-7.86802487869369,
81.1681323349625));
#59998=CARTESIAN_POINT('Ctrl Pts',(0.806504612368069,-7.86978984627448,
81.1674503460731));
#59999=CARTESIAN_POINT('Ctrl Pts',(0.795564984225235,-7.87090326909271,
81.167012015533));
#60000=CARTESIAN_POINT('Ctrl Pts',(0.750909025319721,-7.87535424997989,
81.165226004247));
#60001=CARTESIAN_POINT('Ctrl Pts',(0.717173512987805,-7.87849802406941,
81.1638843621613));
#60002=CARTESIAN_POINT('Ctrl Pts',(0.192208215082014,-7.92401911144263,
81.1431226357622));
#60003=CARTESIAN_POINT('Ctrl Pts',(-0.301919590915243,-7.92060190416507,
81.1252561627711));
#60004=CARTESIAN_POINT('Ctrl Pts',(-1.22547250410126,-7.82760827199199,
81.0928928448127));
#60005=CARTESIAN_POINT('Ctrl Pts',(-1.65403558472917,-7.74837931732449,
81.0782745500247));
#60006=CARTESIAN_POINT('Ctrl Pts',(-2.22817757196753,-7.59241094609808,
81.0572537402212));
#60007=CARTESIAN_POINT('Ctrl Pts',(-2.38114519287338,-7.54583484475337,
81.05150305348));
#60008=CARTESIAN_POINT('Ctrl Pts',(-2.64809556645041,-7.45562710723083,
81.0410462382729));
#60009=CARTESIAN_POINT('Ctrl Pts',(-2.76267786097776,-7.41393245473913,
81.0364173770764));
#60010=CARTESIAN_POINT('Ctrl Pts',(-2.92530418273471,-7.3504618702623,81.0295868800997));
#60011=CARTESIAN_POINT('Ctrl Pts',(-2.97416865641587,-7.33082634086414,
81.0275002187845));
#60012=CARTESIAN_POINT('Ctrl Pts',(-3.03029653294313,-7.30761856971711,
81.0250598717806));
#60013=CARTESIAN_POINT('Ctrl Pts',(-3.03775589137337,-7.30452088651751,
81.0247346599536));
#60014=CARTESIAN_POINT('Ctrl Pts',(-3.04905173236382,-7.29980971364017,
81.0242408163469));
#60015=CARTESIAN_POINT('Ctrl Pts',(-3.05289172582711,-7.29820460334164,
81.0240726952972));
#60016=CARTESIAN_POINT('Ctrl Pts',(-3.05953261170976,-7.29542256679272,
81.0237815283338));
#60017=CARTESIAN_POINT('Ctrl Pts',(-3.06233409940995,-7.2942470546128,81.0236585693276));
#60018=CARTESIAN_POINT('Ctrl Pts',(-3.06813841484015,-7.29180761415803,
81.0234035458553));
#60019=CARTESIAN_POINT('Ctrl Pts',(-3.07114113972537,-7.29054344437614,
81.0232714664692));
#60020=CARTESIAN_POINT('Ctrl Pts',(-3.07932436179535,-7.28709229359252,
81.0229111065713));
#60021=CARTESIAN_POINT('Ctrl Pts',(-3.08450326615387,-7.28490166174089,
81.0226825985884));
#60022=CARTESIAN_POINT('Ctrl Pts',(-3.1044640648564,-7.27643331470342,81.021800144467));
#60023=CARTESIAN_POINT('Ctrl Pts',(-3.11922904227979,-7.27011616744074,
81.0211437471184));
#60024=CARTESIAN_POINT('Ctrl Pts',(-3.36486126244534,-7.16413720416248,
81.0101643522225));
#60025=CARTESIAN_POINT('Ctrl Pts',(-3.59084958190917,-7.0535758314352,80.999189517539));
#60026=CARTESIAN_POINT('Ctrl Pts',(-4.36283522614617,-6.6291707388327,80.9596049269533));
#60027=CARTESIAN_POINT('Ctrl Pts',(-4.87634183917102,-6.26112078069897,
80.9296437927232));
#60028=CARTESIAN_POINT('Ctrl Pts',(-5.49037197959168,-5.69919576410753,
80.8925336947381));
#60029=CARTESIAN_POINT('Ctrl Pts',(-5.63461226004034,-5.55663289245589,
80.8836819762504));
#60030=CARTESIAN_POINT('Ctrl Pts',(-5.88453970221659,-5.289860363415,80.868144174977));
#60031=CARTESIAN_POINT('Ctrl Pts',(-5.99216502846427,-5.16762931389496,
80.8613779520247));
#60032=CARTESIAN_POINT('Ctrl Pts',(-6.11505578713525,-5.01905495792445,
80.8535567561821));
#60033=CARTESIAN_POINT('Ctrl Pts',(-6.13403408823448,-4.99584284994719,
80.8523460403021));
#60034=CARTESIAN_POINT('Ctrl Pts',(-6.15906967581658,-4.96486441875541,
80.8507449640487));
#60035=CARTESIAN_POINT('Ctrl Pts',(-6.16524494942985,-4.95719403318566,
80.850349720776));
#60036=CARTESIAN_POINT('Ctrl Pts',(-6.17537119248089,-4.94456790870893,
80.8497010634125));
#60037=CARTESIAN_POINT('Ctrl Pts',(-6.17933054785953,-4.93961892753841,
80.8494473034487));
#60038=CARTESIAN_POINT('Ctrl Pts',(-6.18699811094366,-4.93001124028371,
80.8489556154404));
#60039=CARTESIAN_POINT('Ctrl Pts',(-6.19070701398151,-4.92535309611299,
80.8487176588349));
#60040=CARTESIAN_POINT('Ctrl Pts',(-6.19926698357264,-4.91457737996965,
80.8481681858024));
#60041=CARTESIAN_POINT('Ctrl Pts',(-6.20411426368553,-4.90845680035173,
80.8478568249644));
#60042=CARTESIAN_POINT('Ctrl Pts',(-6.21924007506219,-4.88929948894017,
80.8468845713691));
#60043=CARTESIAN_POINT('Ctrl Pts',(-6.22948666698175,-4.87623753257832,
80.846224986714));
#60044=CARTESIAN_POINT('Ctrl Pts',(-6.31687753247868,-4.76411003545732,
80.8405911631473));
#60045=CARTESIAN_POINT('Ctrl Pts',(-6.39169626818635,-4.66325067146858,
80.8357120954722));
#60046=CARTESIAN_POINT('Ctrl Pts',(-6.4672863453654,-4.55611228650474,80.8307114852019));
#60047=CARTESIAN_POINT('Ctrl Pts',(-6.47048307297478,-4.55157122790423,
80.8304998690554));
#60048=CARTESIAN_POINT('Ctrl Pts',(-6.47576475550273,-4.54405161173773,
80.8301500016519));
#60049=CARTESIAN_POINT('Ctrl Pts',(-6.47785244120307,-4.54107497942819,
80.8300116497182));
#60050=CARTESIAN_POINT('Ctrl Pts',(-6.48645134802723,-4.52879662026427,
80.8294415463273));
#60051=CARTESIAN_POINT('Ctrl Pts',(-6.49294460622107,-4.51948229998175,
80.8290104552015));
#60052=CARTESIAN_POINT('Ctrl Pts',(-6.50490073938982,-4.50225275424334,
80.8282155661346));
#60053=CARTESIAN_POINT('Ctrl Pts',(-6.51036927188469,-4.49434149090429,
80.827851563085));
#60054=CARTESIAN_POINT('Ctrl Pts',(-6.52786338850867,-4.46893402404727,
80.8266856811337));
#60055=CARTESIAN_POINT('Ctrl Pts',(-6.53983301452147,-4.45139931712575,
80.8258858156482));
#60056=CARTESIAN_POINT('Ctrl Pts',(-6.56062732757918,-4.42067211773139,
80.8244923210264));
#60057=CARTESIAN_POINT('Ctrl Pts',(-6.56948313153249,-4.40750091211186,
80.8238976027076));
#60058=CARTESIAN_POINT('Ctrl Pts',(-6.70908416530263,-4.19851729016821,
80.8145020049814));
#60059=CARTESIAN_POINT('Ctrl Pts',(-6.83106736452198,-3.99698444657958,
80.8060100437487));
#60060=CARTESIAN_POINT('Ctrl Pts',(-7.187272615697,-3.34441175087375,80.7798193897539));
#60061=CARTESIAN_POINT('Ctrl Pts',(-7.38713656546947,-2.87613696774115,
80.7629736062849));
#60062=CARTESIAN_POINT('Ctrl Pts',(-7.61070169582243,-2.17133736910167,
80.7369917311529));
#60063=CARTESIAN_POINT('Ctrl Pts',(-7.6709612878071,-1.94777499839659,80.7286477080544));
#60064=CARTESIAN_POINT('Ctrl Pts',(-7.74241611886805,-1.62735906029986,
80.7161514838298));
#60065=CARTESIAN_POINT('Ctrl Pts',(-7.76176176050609,-1.53243527661734,
80.7123834536608));
#60066=CARTESIAN_POINT('Ctrl Pts',(-7.78246294606769,-1.42038144426406,
80.7078330499648));
#60067=CARTESIAN_POINT('Ctrl Pts',(-7.78551259693344,-1.40356921755494,
80.7071476211443));
#60068=CARTESIAN_POINT('Ctrl Pts',(-7.78947481769972,-1.38131585850794,
80.7062366344355));
#60069=CARTESIAN_POINT('Ctrl Pts',(-7.79043621609811,-1.37588335230544,
80.7060139503231));
#60070=CARTESIAN_POINT('Ctrl Pts',(-7.79200267918132,-1.36697757020063,
80.7056484057416));
#60071=CARTESIAN_POINT('Ctrl Pts',(-7.79261110748777,-1.36350487977847,
80.705505745146));
#60072=CARTESIAN_POINT('Ctrl Pts',(-7.79378382686972,-1.35678499503354,
80.7052294506657));
#60073=CARTESIAN_POINT('Ctrl Pts',(-7.79434841031616,-1.35353785367166,
80.705095834296));
#60074=CARTESIAN_POINT('Ctrl Pts',(-7.79565230182544,-1.34601079240612,
80.704785854506));
#60075=CARTESIAN_POINT('Ctrl Pts',(-7.79639011228957,-1.34173062910365,
80.7046094022217));
#60076=CARTESIAN_POINT('Ctrl Pts',(-7.79877001337654,-1.3278561764917,80.7040368206264));
#60077=CARTESIAN_POINT('Ctrl Pts',(-7.80039791574616,-1.31825949697215,
80.7036398493334));
#60078=CARTESIAN_POINT('Ctrl Pts',(-7.81557074730891,-1.22780165033215,
80.6998894383681));
#60079=CARTESIAN_POINT('Ctrl Pts',(-7.82787512921349,-1.14674018072412,
80.6964640545968));
#60080=CARTESIAN_POINT('Ctrl Pts',(-7.83937863061201,-1.06210895486184,
80.6928315079482));
#60081=CARTESIAN_POINT('Ctrl Pts',(-7.83983802842581,-1.05871263054713,
80.6926856364009));
#60082=CARTESIAN_POINT('Ctrl Pts',(-7.88740827541019,-0.70529737362485,
80.6774967774005));
#60083=CARTESIAN_POINT('Ctrl Pts',(-7.91102585095933,-0.352541444084006,
80.6613572250108));
#60084=CARTESIAN_POINT('Ctrl Pts',(-7.91097302527927,0.368460252008101,
80.6278855848813));
#60085=CARTESIAN_POINT('Ctrl Pts',(-7.88528480223124,0.735903908438486,
80.6105801409096));
#60086=CARTESIAN_POINT('Ctrl Pts',(-7.7647871228187,1.59390167764492,80.5708910084427));
#60087=CARTESIAN_POINT('Ctrl Pts',(-7.64894176064335,2.07996464741413,80.5490279021577));
#60088=CARTESIAN_POINT('Ctrl Pts',(-7.47858398552469,2.57983930427977,80.5275386428139));
#60089=CARTESIAN_POINT('Ctrl Pts',(-7.46892284816607,2.60767727638752,80.5263449113696));
#60090=CARTESIAN_POINT('Ctrl Pts',(-7.45482773537717,2.64757046849945,80.5246384437715));
#60091=CARTESIAN_POINT('Ctrl Pts',(-7.45051964472956,2.65966971171014,80.5241214453457));
#60092=CARTESIAN_POINT('Ctrl Pts',(-7.44356514229715,2.67905188734254,80.5232941316661));
#60093=CARTESIAN_POINT('Ctrl Pts',(-7.44093747023545,2.68634149117227,80.5229831810283));
#60094=CARTESIAN_POINT('Ctrl Pts',(-7.43626178144472,2.69925314100821,80.5224327650337));
#60095=CARTESIAN_POINT('Ctrl Pts',(-7.434218090674,2.70487674061525,80.5221931530464));
#60096=CARTESIAN_POINT('Ctrl Pts',(-7.42996101121678,2.71654962490099,80.5216960363084));
#60097=CARTESIAN_POINT('Ctrl Pts',(-7.4277466098105,2.7225985369603,80.5214385661861));
#60098=CARTESIAN_POINT('Ctrl Pts',(-7.42202048169807,2.73818118342353,80.5207756454288));
#60099=CARTESIAN_POINT('Ctrl Pts',(-7.41849776757067,2.7477108831825,80.5203705685219));
#60100=CARTESIAN_POINT('Ctrl Pts',(-7.40376035055633,2.78734383314351,80.5186872883973));
#60101=CARTESIAN_POINT('Ctrl Pts',(-7.39238062322057,2.81738561890556,80.517414702715));
#60102=CARTESIAN_POINT('Ctrl Pts',(-7.31565623579296,3.01626782886262,80.5090111578946));
#60103=CARTESIAN_POINT('Ctrl Pts',(-7.24471322721281,3.18289697195793,80.5020739594106));
#60104=CARTESIAN_POINT('Ctrl Pts',(-7.02896788073465,3.64495519586056,80.4830193125638));
#60105=CARTESIAN_POINT('Ctrl Pts',(-6.87137100926708,3.93400125750296,80.4713285802795));
#60106=CARTESIAN_POINT('Ctrl Pts',(-6.32322044836416,4.80536571601678,80.4355112141084));
#60107=CARTESIAN_POINT('Ctrl Pts',(-5.87315429183166,5.34606978727673,80.4125810056982));
#60108=CARTESIAN_POINT('Ctrl Pts',(-5.32610102587594,5.849652584334,80.3833197247313));
#60109=CARTESIAN_POINT('Ctrl Pts',(-5.2940764730732,5.87865134837688,80.3816017613637));
#60110=CARTESIAN_POINT('Ctrl Pts',(-5.2552868516254,5.91320197274771,80.3795165511651));
#60111=CARTESIAN_POINT('Ctrl Pts',(-5.24874757090289,5.91900721400563,80.3791648729786));
#60112=CARTESIAN_POINT('Ctrl Pts',(-5.23806040854657,5.92846309666762,80.378589903719));
#60113=CARTESIAN_POINT('Ctrl Pts',(-5.23391829261839,5.93212026496742,80.3783670039762));
#60114=CARTESIAN_POINT('Ctrl Pts',(-5.22652062471598,5.93863805440755,80.3779688220293));
#60115=CARTESIAN_POINT('Ctrl Pts',(-5.22326654215742,5.94150035019,80.3777936385566));
#60116=CARTESIAN_POINT('Ctrl Pts',(-5.21639853891438,5.9475314530496,80.377423836425));
#60117=CARTESIAN_POINT('Ctrl Pts',(-5.21278408006506,5.95069964258606,80.3772291818897));
#60118=CARTESIAN_POINT('Ctrl Pts',(-5.20322519157263,5.95906292390791,80.37671430107));
#60119=CARTESIAN_POINT('Ctrl Pts',(-5.19727587847815,5.96425240643351,80.3763937523235));
#60120=CARTESIAN_POINT('Ctrl Pts',(-5.17031921012709,5.98769527960476,80.3749409382052));
#60121=CARTESIAN_POINT('Ctrl Pts',(-5.14922356154275,6.00584650001665,80.3738029313946));
#60122=CARTESIAN_POINT('Ctrl Pts',(-4.9874166050611,6.14359004184041,80.3650688046558));
#60123=CARTESIAN_POINT('Ctrl Pts',(-4.8426579324136,6.25832893909334,80.3572248425135));
#60124=CARTESIAN_POINT('Ctrl Pts',(-4.51884517720447,6.49702410034487,80.339822949134));
#60125=CARTESIAN_POINT('Ctrl Pts',(-4.33841510465881,6.61886956266665,80.3302174383871));
#60126=CARTESIAN_POINT('Ctrl Pts',(-3.58419945627548,7.08409313952916,80.2909412784782));
#60127=CARTESIAN_POINT('Ctrl Pts',(-2.97293497985739,7.36156924940989,80.261383389688));
#60128=CARTESIAN_POINT('Ctrl Pts',(-2.23454013695276,7.58957131826241,80.22953921955));
#60129=CARTESIAN_POINT('Ctrl Pts',(-2.13445455763394,7.61832441486272,80.2252925580171));
#60130=CARTESIAN_POINT('Ctrl Pts',(-2.01490932629076,7.6501271026298,80.2202975918372));
#60131=CARTESIAN_POINT('Ctrl Pts',(-1.99597116738945,7.6550900310333,80.2195085808122));
#60132=CARTESIAN_POINT('Ctrl Pts',(-1.9653586495349,7.66299101481573,80.2182368113831));
#60133=CARTESIAN_POINT('Ctrl Pts',(-1.95369570384629,7.66597280273699,80.2177531325557));
#60134=CARTESIAN_POINT('Ctrl Pts',(-1.93288015327237,7.67124398798022,80.2168913773492));
#60135=CARTESIAN_POINT('Ctrl Pts',(-1.92373018206954,7.67354365316913,80.2165130866736));
#60136=CARTESIAN_POINT('Ctrl Pts',(-1.9046589560219,7.67830057564779,80.2157256806043));
#60137=CARTESIAN_POINT('Ctrl Pts',(-1.89473700365983,7.68075498609132,80.2153166255628));
#60138=CARTESIAN_POINT('Ctrl Pts',(-1.86907625303962,7.68704998155722,80.2142602472231));
#60139=CARTESIAN_POINT('Ctrl Pts',(-1.85333034109061,7.69086146722528,80.2136135342467));
#60140=CARTESIAN_POINT('Ctrl Pts',(-1.78693152128647,7.70671833765004,80.2108927059853));
#60141=CARTESIAN_POINT('Ctrl Pts',(-1.73617170472421,7.71831197196389,80.2088281374913));
#60142=CARTESIAN_POINT('Ctrl Pts',(-1.39476922160644,7.79275055331919,80.1950433650332));
#60143=CARTESIAN_POINT('Ctrl Pts',(-1.10088901551697,7.83966834999513,80.18368072138));
#60144=CARTESIAN_POINT('Ctrl Pts',(-0.413876672078214,7.90994603746026,
80.1579272271261));
#60145=CARTESIAN_POINT('Ctrl Pts',(-0.0202562489549062,7.92074091160252,
80.1437905274532));
#60146=CARTESIAN_POINT('Ctrl Pts',(0.79281471282269,7.88241051422963,80.1143249393133));
#60147=CARTESIAN_POINT('Ctrl Pts',(1.21081823110053,7.82910078404111,80.0990223079734));
#60148=CARTESIAN_POINT('Ctrl Pts',(1.66717577250144,7.73346776203641,80.080629823665));
#60149=CARTESIAN_POINT('Ctrl Pts',(1.71170609035062,7.72373360667324,80.078816666842));
#60150=CARTESIAN_POINT('Ctrl Pts',(1.76482283271653,7.71164058428669,80.0766294569681));
#60151=CARTESIAN_POINT('Ctrl Pts',(1.77349314098979,7.70965123789846,80.0762716557538));
#60152=CARTESIAN_POINT('Ctrl Pts',(1.78752670113109,7.70640640204375,80.0756912392515));
#60153=CARTESIAN_POINT('Ctrl Pts',(1.7928920449785,7.70515992407334,80.0754690279908));
#60154=CARTESIAN_POINT('Ctrl Pts',(1.80248530329826,7.7029206533843,80.0750711613642));
#60155=CARTESIAN_POINT('Ctrl Pts',(1.80671371405332,7.70192997996482,80.0748956022065));
#60156=CARTESIAN_POINT('Ctrl Pts',(1.81558161612889,7.69984461651287,80.0745270100957));
#60157=CARTESIAN_POINT('Ctrl Pts',(1.82022093678821,7.69874921428125,80.0743339445756));
#60158=CARTESIAN_POINT('Ctrl Pts',(1.8323695314035,7.69586918252703,80.0738277631398));
#60159=CARTESIAN_POINT('Ctrl Pts',(1.83987717598649,7.69407775830387,80.0735143328916));
#60160=CARTESIAN_POINT('Ctrl Pts',(1.8728061548083,7.68616951198746,80.0721368548667));
#60161=CARTESIAN_POINT('Ctrl Pts',(1.89819947466377,7.67993772037388,80.0710674008728));
#60162=CARTESIAN_POINT('Ctrl Pts',(2.07326134877294,7.63605439377818,80.0636421880189));
#60163=CARTESIAN_POINT('Ctrl Pts',(2.22181352760151,7.59416050701445,80.0570619863029));
#60164=CARTESIAN_POINT('Ctrl Pts',(2.59909595537404,7.47574511436507,80.0397782292706));
#60165=CARTESIAN_POINT('Ctrl Pts',(2.82572908799643,7.39305820051112,80.0288544894765));
#60166=CARTESIAN_POINT('Ctrl Pts',(3.79551912462423,6.98811695278454,79.9806897665835));
#60167=CARTESIAN_POINT('Ctrl Pts',(4.49066904129472,6.56308956521699,79.943062755289));
#60168=CARTESIAN_POINT('Ctrl Pts',(5.14988420903908,6.00545201532558,79.9077090766996));
#60169=CARTESIAN_POINT('Ctrl Pts',(5.19022481684917,5.9706220591907,79.905544023911));
#60170=CARTESIAN_POINT('Ctrl Pts',(5.23886786168367,5.92775823250875,79.9029310894273));
#60171=CARTESIAN_POINT('Ctrl Pts',(5.2475081212879,5.92011086498983,79.9024668749909));
#60172=CARTESIAN_POINT('Ctrl Pts',(5.26168735917662,5.90750559830426,79.9017049138386));
#60173=CARTESIAN_POINT('Ctrl Pts',(5.26723612066034,5.90255875949788,79.9014066964705));
#60174=CARTESIAN_POINT('Ctrl Pts',(5.27719626087805,5.89365385397001,79.900871317809));
#60175=CARTESIAN_POINT('Ctrl Pts',(5.28161017616302,5.88969864029509,79.9006340348636));
#60176=CARTESIAN_POINT('Ctrl Pts',(5.29088511752214,5.88136875568284,79.9001353779689));
#60177=CARTESIAN_POINT('Ctrl Pts',(5.29574517358476,5.87699300866216,79.899874050452));
#60178=CARTESIAN_POINT('Ctrl Pts',(5.30850157049156,5.86547912628823,79.8991880464961));
#60179=CARTESIAN_POINT('Ctrl Pts',(5.3163889524539,5.8583310603127,79.8987637975312));
#60180=CARTESIAN_POINT('Ctrl Pts',(5.33370827804382,5.84257136242672,79.8978320194101));
#60181=CARTESIAN_POINT('Ctrl Pts',(5.34313385115761,5.83395275700235,79.8973247927922));
#60182=CARTESIAN_POINT('Ctrl Pts',(5.37084877399009,5.80848713224403,79.8958329352727));
#60183=CARTESIAN_POINT('Ctrl Pts',(5.38907968838866,5.79157659410226,79.8948510611496));
#60184=CARTESIAN_POINT('Ctrl Pts',(5.57668388104208,5.61590683165143,79.8847410443292));
#60185=CARTESIAN_POINT('Ctrl Pts',(5.73907712141885,5.44984559648409,79.8759429556149));
#60186=CARTESIAN_POINT('Ctrl Pts',(6.137684155715,5.00462620193725,79.8540118248301));
#60187=CARTESIAN_POINT('Ctrl Pts',(6.36228007263128,4.71580985524251,79.8413319640221));
#60188=CARTESIAN_POINT('Ctrl Pts',(6.93845064220596,3.85842570922307,79.8061025996344));
#60189=CARTESIAN_POINT('Ctrl Pts',(7.23911062469615,3.25953675898994,79.7843081166348));
#60190=CARTESIAN_POINT('Ctrl Pts',(7.46355999082669,2.62283303601201,79.7577483753527));
#60191=CARTESIAN_POINT('Ctrl Pts',(7.46612177787413,2.61553177550486,79.7574433585223));
#60192=CARTESIAN_POINT('Ctrl Pts',(7.47995227390394,2.57592806833074,79.7557863888887));
#60193=CARTESIAN_POINT('Ctrl Pts',(7.49102190842974,2.54355698439586,79.7544230541428));
#60194=CARTESIAN_POINT('Ctrl Pts',(7.50399967711359,2.50478629713728,79.7527784216497));
#60195=CARTESIAN_POINT('Ctrl Pts',(7.50611027313306,2.49845434529178,79.7525094493681));
#60196=CARTESIAN_POINT('Ctrl Pts',(7.50951356640925,2.48820096548872,79.7520732842098));
#60197=CARTESIAN_POINT('Ctrl Pts',(7.51081121467751,2.48428117290919,79.7519063958055));
#60198=CARTESIAN_POINT('Ctrl Pts',(7.51312968093741,2.47725938526742,79.7516071738112));
#60199=CARTESIAN_POINT('Ctrl Pts',(7.51415164659003,2.47415777516295,79.7514749115497));
#60200=CARTESIAN_POINT('Ctrl Pts',(7.51630450244715,2.46761033779156,79.7511955151536));
#60201=CARTESIAN_POINT('Ctrl Pts',(7.51743494458023,2.46416436274076,79.7510483533837));
#60202=CARTESIAN_POINT('Ctrl Pts',(7.52041961663174,2.45504489094875,79.7506586063866));
#60203=CARTESIAN_POINT('Ctrl Pts',(7.52226979280268,2.44937008038857,79.7504157737379));
#60204=CARTESIAN_POINT('Ctrl Pts',(7.53064390351867,2.42358625453281,79.7493110923044));
#60205=CARTESIAN_POINT('Ctrl Pts',(7.53709358235142,2.40345340066538,79.7484447730924));
#60206=CARTESIAN_POINT('Ctrl Pts',(7.58456167742715,2.25321024023933,79.7419532894421));
#60207=CARTESIAN_POINT('Ctrl Pts',(7.6222871205614,2.12209035710128,79.7361404023714));
#60208=CARTESIAN_POINT('Ctrl Pts',(7.71029246483093,1.78349794802351,79.7208791567034));
#60209=CARTESIAN_POINT('Ctrl Pts',(7.75559910892461,1.57484880563962,79.7112388799914));
#60210=CARTESIAN_POINT('Ctrl Pts',(7.83521536941418,1.12021955223917,79.6900906088558));
#60211=CARTESIAN_POINT('Ctrl Pts',(7.86649478672846,0.873928003626052,79.6785473503489));
#60212=CARTESIAN_POINT('Ctrl Pts',(7.92227047051475,0.171929409369034,79.645990134639));
#60213=CARTESIAN_POINT('Ctrl Pts',(7.91901289184965,-0.285028556764483,
79.6252614688054));
#60214=CARTESIAN_POINT('Ctrl Pts',(7.85752424863358,-0.940210731153474,
79.5971025091756));
#60215=CARTESIAN_POINT('Ctrl Pts',(7.83097021654703,-1.14043727857879,79.5886983746942));
#60216=CARTESIAN_POINT('Ctrl Pts',(7.79360045864102,-1.35796397947993,79.5797841820767));
#60217=CARTESIAN_POINT('Ctrl Pts',(7.79035206873331,-1.37647699952185,79.5790272203026));
#60218=CARTESIAN_POINT('Ctrl Pts',(7.78570466647016,-1.40241969362595,79.5779688274373));
#60219=CARTESIAN_POINT('Ctrl Pts',(7.78436094857258,-1.40985913243631,79.5776655898506));
#60220=CARTESIAN_POINT('Ctrl Pts',(7.78201350263977,-1.42275000262988,79.5771406161085));
#60221=CARTESIAN_POINT('Ctrl Pts',(7.78101470618975,-1.42820232022114,79.5769187188093));
#60222=CARTESIAN_POINT('Ctrl Pts',(7.77894956359659,-1.43940923275327,79.5764629199714));
#60223=CARTESIAN_POINT('Ctrl Pts',(7.77788256023152,-1.44516370413895,79.5762290400876));
#60224=CARTESIAN_POINT('Ctrl Pts',(7.77537362948569,-1.45861138978029,79.5756828596188));
#60225=CARTESIAN_POINT('Ctrl Pts',(7.7739266672065,-1.46630366495492,79.5753707240387));
#60226=CARTESIAN_POINT('Ctrl Pts',(7.77085231195023,-1.48251494672703,79.5747135089549));
#60227=CARTESIAN_POINT('Ctrl Pts',(7.76922232038534,-1.49103345316784,79.5743685149121));
#60228=CARTESIAN_POINT('Ctrl Pts',(7.76481981989393,-1.51383815043945,79.5734458736839));
#60229=CARTESIAN_POINT('Ctrl Pts',(7.76202188779973,-1.52811943166562,79.5728690588144));
#60230=CARTESIAN_POINT('Ctrl Pts',(7.75337808704979,-1.57160306193506,79.5711157304031));
#60231=CARTESIAN_POINT('Ctrl Pts',(7.74740668009732,-1.60078034200157,79.5699433247036));
#60232=CARTESIAN_POINT('Ctrl Pts',(7.70046947317296,-1.82370714750096,79.5610158764868));
#60233=CARTESIAN_POINT('Ctrl Pts',(7.65240509641148,-2.01589699467982,79.5534969407213));
#60234=CARTESIAN_POINT('Ctrl Pts',(7.54323288431402,-2.39185658241609,79.5390347286315));
#60235=CARTESIAN_POINT('Ctrl Pts',(7.48249259642664,-2.57558716398644,79.5320869407689));
#60236=CARTESIAN_POINT('Ctrl Pts',(7.14228368897107,-3.49062358935137,79.4976913598856));
#60237=CARTESIAN_POINT('Ctrl Pts',(6.76216051405794,-4.1796506963553,79.4728900337485));
#60238=CARTESIAN_POINT('Ctrl Pts',(6.24808266806303,-4.8527865246023,79.4400027022402));
#60239=CARTESIAN_POINT('Ctrl Pts',(6.20834487169694,-4.90352195937002,79.4374612513421));
#60240=CARTESIAN_POINT('Ctrl Pts',(6.16283406394189,-4.96018801741824,79.434544334826));
#60241=CARTESIAN_POINT('Ctrl Pts',(6.15766540368655,-4.96660302853843,79.4342129715344));
#60242=CARTESIAN_POINT('Ctrl Pts',(6.14983351659487,-4.97629244847395,79.4337107140808));
#60243=CARTESIAN_POINT('Ctrl Pts',(6.14717766843573,-4.97957282575399,79.4335403678943));
#60244=CARTESIAN_POINT('Ctrl Pts',(6.14253857056091,-4.985293451475,79.4332427707029));
#60245=CARTESIAN_POINT('Ctrl Pts',(6.14055648427698,-4.9877346512719,79.4331156059192));
#60246=CARTESIAN_POINT('Ctrl Pts',(6.13640407572047,-4.99284266141862,79.4328491709072));
#60247=CARTESIAN_POINT('Ctrl Pts',(6.13423346986049,-4.99550923924397,79.4327098797955));
#60248=CARTESIAN_POINT('Ctrl Pts',(6.12907387219671,-5.00183934415124,79.4323787433379));
#60249=CARTESIAN_POINT('Ctrl Pts',(6.12608333591701,-5.00550160491037,79.4321867849442));
#60250=CARTESIAN_POINT('Ctrl Pts',(6.11610453983743,-5.01769946790715,79.4315461680771));
#60251=CARTESIAN_POINT('Ctrl Pts',(6.10910173666164,-5.02622310102447,79.4310964538033));
#60252=CARTESIAN_POINT('Ctrl Pts',(5.90687112156473,-5.27132604237178,79.4181058013499));
#60253=CARTESIAN_POINT('Ctrl Pts',(5.69808231253967,-5.49634686213858,79.4046050386651));
#60254=CARTESIAN_POINT('Ctrl Pts',(5.1993742622261,-5.97479823347969,79.3733159158589));
#60255=CARTESIAN_POINT('Ctrl Pts',(4.90293846429737,-6.220361833413,79.3553660769933));
#60256=CARTESIAN_POINT('Ctrl Pts',(4.34963794773614,-6.614494227712,79.3242186194346));
#60257=CARTESIAN_POINT('Ctrl Pts',(4.10005992832687,-6.77203153815581,79.3109056383335));
#60258=CARTESIAN_POINT('Ctrl Pts',(3.58993270007486,-7.05546775563662,79.2854194196948));
#60259=CARTESIAN_POINT('Ctrl Pts',(3.33011316986904,-7.18175544236608,79.2732469964317));
#60260=CARTESIAN_POINT('Ctrl Pts',(3.0444149158597,-7.30177429469146,79.2607104027392));
#60261=CARTESIAN_POINT('Ctrl Pts',(3.02484543341494,-7.30990288194682,79.2598557732196));
#60262=CARTESIAN_POINT('Ctrl Pts',(2.99704442625382,-7.32131984465816,79.2586474095015));
#60263=CARTESIAN_POINT('Ctrl Pts',(2.98883975503528,-7.32467313128044,79.2582915035208));
#60264=CARTESIAN_POINT('Ctrl Pts',(2.97485153381493,-7.33036276450165,79.2576859173835));
#60265=CARTESIAN_POINT('Ctrl Pts',(2.96907083334839,-7.33270606899126,79.257436004928));
#60266=CARTESIAN_POINT('Ctrl Pts',(2.95754665489451,-7.33736172738178,79.2569384825089));
#60267=CARTESIAN_POINT('Ctrl Pts',(2.95180322187117,-7.33967418036374,79.2566908693619));
#60268=CARTESIAN_POINT('Ctrl Pts',(2.94024468285565,-7.34431218211625,79.2561932402019));
#60269=CARTESIAN_POINT('Ctrl Pts',(2.93442951805531,-7.34663757287899,79.2559432295743));
#60270=CARTESIAN_POINT('Ctrl Pts',(2.913592252244,-7.35494137244679,79.2550486229524));
#60271=CARTESIAN_POINT('Ctrl Pts',(2.89855454613194,-7.36088065053992,79.2544053287518));
#60272=CARTESIAN_POINT('Ctrl Pts',(2.74515299566154,-7.42092500372552,79.2478664351905));
#60273=CARTESIAN_POINT('Ctrl Pts',(2.60530552162057,-7.4711698467326,79.2421000878005));
#60274=CARTESIAN_POINT('Ctrl Pts',(2.22950887252862,-7.59435106602856,79.2270670596992));
#60275=CARTESIAN_POINT('Ctrl Pts',(1.99141756078703,-7.66023131092465,79.2180215579339));
#60276=CARTESIAN_POINT('Ctrl Pts',(0.953196788596171,-7.89581983280163,
79.1799727570577));
#60277=CARTESIAN_POINT('Ctrl Pts',(0.132689807819647,-7.95201374208558,
79.1538743071341));
#60278=CARTESIAN_POINT('Ctrl Pts',(-0.723066059411459,-7.87799591481916,
79.1200659384808));
#60279=CARTESIAN_POINT('Ctrl Pts',(-0.764393145535784,-7.87409341873729,
79.1184158186872));
#60280=CARTESIAN_POINT('Ctrl Pts',(-0.813067159633271,-7.86911035839927,
79.1164499045633));
#60281=CARTESIAN_POINT('Ctrl Pts',(-0.820446306517562,-7.8683444190132,
79.1161512565424));
#60282=CARTESIAN_POINT('Ctrl Pts',(-0.832285229273103,-7.86709872932681,
79.1156711212081));
#60283=CARTESIAN_POINT('Ctrl Pts',(-0.836745706032739,-7.86662556265975,
79.1154899976521));
#60284=CARTESIAN_POINT('Ctrl Pts',(-0.844657851658747,-7.86577943796962,
79.1151683099738));
#60285=CARTESIAN_POINT('Ctrl Pts',(-0.848109685983407,-7.86540800045981,
79.1150278304882));
#60286=CARTESIAN_POINT('Ctrl Pts',(-0.855322027190808,-7.86462710742375,
79.1147340223114));
#60287=CARTESIAN_POINT('Ctrl Pts',(-0.859082476448986,-7.86421722789931,
79.1145806705307));
#60288=CARTESIAN_POINT('Ctrl Pts',(-0.868902412748709,-7.8631397520487,
79.114179789123));
#60289=CARTESIAN_POINT('Ctrl Pts',(-0.874961415132839,-7.86246784952252,
79.1139320207558));
#60290=CARTESIAN_POINT('Ctrl Pts',(-0.901271790409248,-7.8595194166701,
79.1128543137748));
#60291=CARTESIAN_POINT('Ctrl Pts',(-0.921514946826898,-7.85717165970015,
79.1120204768454));
#60292=CARTESIAN_POINT('Ctrl Pts',(-1.27348219138459,-7.81497237240634,
79.0974444134725));
#60293=CARTESIAN_POINT('Ctrl Pts',(-1.60233683013468,-7.75422649654075,
79.0826276786597));
#60294=CARTESIAN_POINT('Ctrl Pts',(-2.25829195044068,-7.58954412142652,
79.0519304291025));
#60295=CARTESIAN_POINT('Ctrl Pts',(-2.58449083708362,-7.48474931647354,
79.036070613588));
#60296=CARTESIAN_POINT('Ctrl Pts',(-3.08781728245134,-7.28620815438222,
79.0114219608624));
#60297=CARTESIAN_POINT('Ctrl Pts',(-3.26994497427875,-7.20631040466761,
79.0024598851414));
#60298=CARTESIAN_POINT('Ctrl Pts',(-3.76553098955796,-6.9662398813804,78.9781079404444));
#60299=CARTESIAN_POINT('Ctrl Pts',(-4.07162117289454,-6.79188217995465,
78.9631260975853));
#60300=CARTESIAN_POINT('Ctrl Pts',(-4.38379834759552,-6.58534244119041,
78.9479751911803));
#60301=CARTESIAN_POINT('Ctrl Pts',(-4.40243208634364,-6.57290002631632,
78.94707124155));
#60302=CARTESIAN_POINT('Ctrl Pts',(-4.42853992690136,-6.55530605719133,
78.9458052381632));
#60303=CARTESIAN_POINT('Ctrl Pts',(-4.43605832085272,-6.55022060409479,
78.9454407229093));
#60304=CARTESIAN_POINT('Ctrl Pts',(-4.44876670448191,-6.54159271839358,
78.9448246812294));
#60305=CARTESIAN_POINT('Ctrl Pts',(-4.45396124757696,-6.53805702709628,
78.9445729031083));
#60306=CARTESIAN_POINT('Ctrl Pts',(-4.46423481696767,-6.53104634578861,
78.9440750008553));
#60307=CARTESIAN_POINT('Ctrl Pts',(-4.46931401162571,-6.52757161106412,
78.9438288674296));
#60308=CARTESIAN_POINT('Ctrl Pts',(-4.47950172504379,-6.52058461551426,
78.943335231553));
#60309=CARTESIAN_POINT('Ctrl Pts',(-4.48461018019155,-6.51707226940881,
78.9430877325681));
#60310=CARTESIAN_POINT('Ctrl Pts',(-4.50253636826754,-6.50471596320192,
78.9422193182891));
#60311=CARTESIAN_POINT('Ctrl Pts',(-4.51533214954109,-6.4958401375304,78.9415996021579));
#60312=CARTESIAN_POINT('Ctrl Pts',(-4.62957516886812,-6.41609451314089,
78.9360679902825));
#60313=CARTESIAN_POINT('Ctrl Pts',(-4.7293751475187,-6.34288951913152,78.9312454788173));
#60314=CARTESIAN_POINT('Ctrl Pts',(-5.07967108090469,-6.07307536378398,
78.9143197396728));
#60315=CARTESIAN_POINT('Ctrl Pts',(-5.31997250147967,-5.86372028647672,
78.9027255588542));
#60316=CARTESIAN_POINT('Ctrl Pts',(-6.04589473124956,-5.14982191876501,
78.8667663534886));
#60317=CARTESIAN_POINT('Ctrl Pts',(-6.4774195546405,-4.59525263197187,78.8441097279409));
#60318=CARTESIAN_POINT('Ctrl Pts',(-6.86426259511397,-3.9332346530885,78.8153463276482));
#60319=CARTESIAN_POINT('Ctrl Pts',(-6.89742120020961,-3.87479240943078,
78.8127915211652));
#60320=CARTESIAN_POINT('Ctrl Pts',(-6.96706733055241,-3.74831338380656,
78.8072146239791));
#60321=CARTESIAN_POINT('Ctrl Pts',(-7.0033111507173,-3.6801511704084,78.80417992099));
#60322=CARTESIAN_POINT('Ctrl Pts',(-7.04303734580938,-3.60272709785791,
78.8006885061703));
#60323=CARTESIAN_POINT('Ctrl Pts',(-7.04750778531265,-3.59397434749516,
78.8002931704507));
#60324=CARTESIAN_POINT('Ctrl Pts',(-7.05398357179348,-3.58123675135194,
78.7997169002466));
#60325=CARTESIAN_POINT('Ctrl Pts',(-7.05600189206206,-3.57725847534528,
78.7995367817612));
#60326=CARTESIAN_POINT('Ctrl Pts',(-7.05955517299863,-3.57023995812577,
78.7992187739788));
#60327=CARTESIAN_POINT('Ctrl Pts',(-7.06109153898057,-3.56720042572293,
78.799080973737));
#60328=CARTESIAN_POINT('Ctrl Pts',(-7.06426068371198,-3.56092054929427,
78.7987961031376));
#60329=CARTESIAN_POINT('Ctrl Pts',(-7.06589319657912,-3.55768007278312,
78.7986490159099));
#60330=CARTESIAN_POINT('Ctrl Pts',(-7.07006705555556,-3.5493809148498,78.7982720756711));
#60331=CARTESIAN_POINT('Ctrl Pts',(-7.07260518124568,-3.54432066813838,
78.7980420181973));
#60332=CARTESIAN_POINT('Ctrl Pts',(-7.08320168672602,-3.5231377693434,78.7970780223262));
#60333=CARTESIAN_POINT('Ctrl Pts',(-7.09121031415583,-3.50699046859701,
78.79634091263));
#60334=CARTESIAN_POINT('Ctrl Pts',(-7.14559453173661,-3.39639098360176,
78.7912774029081));
#60335=CARTESIAN_POINT('Ctrl Pts',(-7.19013506836218,-3.30105268276544,
78.7868393009624));
#60336=CARTESIAN_POINT('Ctrl Pts',(-7.29552514498684,-3.06320723047647,
78.7756432051801));
#60337=CARTESIAN_POINT('Ctrl Pts',(-7.3541138662016,-2.91974840812836,78.7687826402078));
#60338=CARTESIAN_POINT('Ctrl Pts',(-7.74065183677902,-1.88768026220992,
78.7191456988919));
#60339=CARTESIAN_POINT('Ctrl Pts',(-7.91096337093462,-0.947868983073772,
78.6737611126276));
#60340=CARTESIAN_POINT('Ctrl Pts',(-7.91099999409123,-0.000305758797192468,
78.6348799381992));
#60341=CARTESIAN_POINT('',(-7.91099994932565,-0.00089541584189321,74.6422459153707));
#60342=CARTESIAN_POINT('Ctrl Pts',(-7.91099999420061,-0.000302915639028901,
78.6348798215365));
#60343=CARTESIAN_POINT('Ctrl Pts',(-7.91100231916487,0.0604162741918949,
78.6323883437237));
#60344=CARTESIAN_POINT('Ctrl Pts',(-7.91030558913058,0.121134580029745,
78.6299192893085));
#60345=CARTESIAN_POINT('Ctrl Pts',(-7.90868088875777,0.191798936417204,
78.6270712755329));
#60346=CARTESIAN_POINT('Ctrl Pts',(-7.90843310492471,0.201757423937507,
78.626670503395));
#60347=CARTESIAN_POINT('Ctrl Pts',(-7.90798595190084,0.218459845575327,
78.6259993091337));
#60348=CARTESIAN_POINT('Ctrl Pts',(-7.90779676433721,0.22520402711425,78.625728559936));
#60349=CARTESIAN_POINT('Ctrl Pts',(-7.90743603391781,0.237502093317745,
78.6252353350452));
#60350=CARTESIAN_POINT('Ctrl Pts',(-7.90726726694386,0.243056051391161,
78.6250127702498));
#60351=CARTESIAN_POINT('Ctrl Pts',(-7.90692663841683,0.253889819597429,
78.624578979869));
#60352=CARTESIAN_POINT('Ctrl Pts',(-7.90675533968934,0.259169643744248,
78.6243677363077));
#60353=CARTESIAN_POINT('Ctrl Pts',(-7.90635168343451,0.271238270803548,
78.6238852485638));
#60354=CARTESIAN_POINT('Ctrl Pts',(-7.90611587016403,0.278026958299536,
78.6236141156283));
#60355=CARTESIAN_POINT('Ctrl Pts',(-7.90545459447109,0.296382572294297,
78.6228817385796));
#60356=CARTESIAN_POINT('Ctrl Pts',(-7.90501248885136,0.307948903244428,
78.6224210297718));
#60357=CARTESIAN_POINT('Ctrl Pts',(-7.90283522523646,0.361812785545211,
78.6202791368633));
#60358=CARTESIAN_POINT('Ctrl Pts',(-7.90078594296876,0.404097321005026,
78.6186080622735));
#60359=CARTESIAN_POINT('Ctrl Pts',(-7.89646648899367,0.480529959756134,
78.6156056221322));
#60360=CARTESIAN_POINT('Ctrl Pts',(-7.89431396640791,0.514683486387897,
78.614270560532));
#60361=CARTESIAN_POINT('Ctrl Pts',(-7.83204462021638,1.41010260908118,78.5794354094257));
#60362=CARTESIAN_POINT('Ctrl Pts',(-7.63159789404408,2.25563136562526,78.5514712961313));
#60363=CARTESIAN_POINT('Ctrl Pts',(-7.19648694551417,3.29613080851428,78.5118978442765));
#60364=CARTESIAN_POINT('Ctrl Pts',(-7.08225547351034,3.53490336060398,78.5023490873609));
#60365=CARTESIAN_POINT('Ctrl Pts',(-6.91740883185871,3.8392761291715,78.4890078640274));
#60366=CARTESIAN_POINT('Ctrl Pts',(-6.87742122981216,3.91045553774849,78.4858002875659));
#60367=CARTESIAN_POINT('Ctrl Pts',(-6.83196954441888,3.98850706289354,78.4821710952793));
#60368=CARTESIAN_POINT('Ctrl Pts',(-6.82758620217426,3.99600589305646,78.4818212634931));
#60369=CARTESIAN_POINT('Ctrl Pts',(-6.82106141939508,4.00712612893741,78.4813007475243));
#60370=CARTESIAN_POINT('Ctrl Pts',(-6.81892941325859,4.01075309103175,78.4811307013922));
#60371=CARTESIAN_POINT('Ctrl Pts',(-6.81528802322958,4.01693651607664,78.4808403255222));
#60372=CARTESIAN_POINT('Ctrl Pts',(-6.81378008904254,4.01949383777388,78.4807200946844));
#60373=CARTESIAN_POINT('Ctrl Pts',(-6.81069582667807,4.0247177481155,78.4804742123688));
#60374=CARTESIAN_POINT('Ctrl Pts',(-6.80911937695788,4.02738425107126,78.4803485524277));
#60375=CARTESIAN_POINT('Ctrl Pts',(-6.80533848481893,4.03377091642562,78.4800472162309));
#60376=CARTESIAN_POINT('Ctrl Pts',(-6.80313256252285,4.03749019017393,78.4798714386365));
#60377=CARTESIAN_POINT('Ctrl Pts',(-6.79516225420659,4.05090337322374,78.4792364570196));
#60378=CARTESIAN_POINT('Ctrl Pts',(-6.78938021369226,4.06058672011185,78.4787760514448));
#60379=CARTESIAN_POINT('Ctrl Pts',(-6.7050674897427,4.20110409069561,78.4720663694254));
#60380=CARTESIAN_POINT('Ctrl Pts',(-6.62279256766777,4.32964418097776,78.4655677578941));
#60381=CARTESIAN_POINT('Ctrl Pts',(-6.47828565925252,4.54164622718403,78.4543425047208));
#60382=CARTESIAN_POINT('Ctrl Pts',(-6.41802665673729,4.62640984825984,78.4497115052583));
#60383=CARTESIAN_POINT('Ctrl Pts',(-5.914926715161,5.30534615218292,78.4116005711583));
#60384=CARTESIAN_POINT('Ctrl Pts',(-5.39225904924774,5.83582361271461,78.3758003975096));
#60385=CARTESIAN_POINT('Ctrl Pts',(-4.65315047291624,6.40061189385736,78.3347024824383));
#60386=CARTESIAN_POINT('Ctrl Pts',(-4.49890656263372,6.50995300942389,78.3265356314296));
#60387=CARTESIAN_POINT('Ctrl Pts',(-4.26070365078017,6.66629765427585,78.3145423480617));
#60388=CARTESIAN_POINT('Ctrl Pts',(-4.17956854109272,6.71746438070253,78.3105600496442));
#60389=CARTESIAN_POINT('Ctrl Pts',(-4.06760348778155,6.78525947052007,78.3052016020811));
#60390=CARTESIAN_POINT('Ctrl Pts',(-4.0375659115222,6.8031761529855,78.3037772453164));
#60391=CARTESIAN_POINT('Ctrl Pts',(-3.993240622965,6.82921814043955,78.3016945167937));
#60392=CARTESIAN_POINT('Ctrl Pts',(-3.97904504087964,6.83749893233023,78.301030367026));
#60393=CARTESIAN_POINT('Ctrl Pts',(-3.95340464433383,6.85234900248835,78.2998358911431));
#60394=CARTESIAN_POINT('Ctrl Pts',(-3.94196902241155,6.85893398148249,78.2993049847743));
#60395=CARTESIAN_POINT('Ctrl Pts',(-3.92545019911769,6.86839106489527,78.2985407117115));
#60396=CARTESIAN_POINT('Ctrl Pts',(-3.92038024093545,6.87128618620726,78.2983064965909));
#60397=CARTESIAN_POINT('Ctrl Pts',(-3.91038506852408,6.8769791115831,78.2978454517607));
#60398=CARTESIAN_POINT('Ctrl Pts',(-3.90546004571132,6.87977724325514,78.2976186100745));
#60399=CARTESIAN_POINT('Ctrl Pts',(-3.8956539285142,6.8853346256848,78.2971676120563));
#60400=CARTESIAN_POINT('Ctrl Pts',(-3.89077289799772,6.88809398126724,78.2969434519563));
#60401=CARTESIAN_POINT('Ctrl Pts',(-3.87918670626357,6.89462766960905,78.2964121297934));
#60402=CARTESIAN_POINT('Ctrl Pts',(-3.87247895790787,6.89839741719799,78.2961051358746));
#60403=CARTESIAN_POINT('Ctrl Pts',(-3.84886115456022,6.91162529498397,78.2950263614381));
#60404=CARTESIAN_POINT('Ctrl Pts',(-3.83192179851748,6.92103111843563,78.2942564933217));
#60405=CARTESIAN_POINT('Ctrl Pts',(-3.62044332119733,7.03744320714579,78.2846927052242));
#60406=CARTESIAN_POINT('Ctrl Pts',(-3.42151039836307,7.1362800266393,78.2762009262083));
#60407=CARTESIAN_POINT('Ctrl Pts',(-2.95474596563154,7.34417268838938,78.2572387840704));
#60408=CARTESIAN_POINT('Ctrl Pts',(-2.68457011616749,7.44718011530263,78.2469615141587));
#60409=CARTESIAN_POINT('Ctrl Pts',(-2.23397009589962,7.59125834307041,78.2304685780765));
#60410=CARTESIAN_POINT('Ctrl Pts',(-2.05667982513524,7.64119719606544,78.2241342117598));
#60411=CARTESIAN_POINT('Ctrl Pts',(-1.82680316116796,7.69736760348467,78.2159887550091));
#60412=CARTESIAN_POINT('Ctrl Pts',(-1.77567563327268,7.70932252846788,78.2141812339163));
#60413=CARTESIAN_POINT('Ctrl Pts',(-1.66512333359709,7.73401437749425,78.2102761550466));
#60414=CARTESIAN_POINT('Ctrl Pts',(-1.605663225567,7.74657728738832,78.2081778701038));
#60415=CARTESIAN_POINT('Ctrl Pts',(-1.47518452392972,7.77257840689903,78.2035686872149));
#60416=CARTESIAN_POINT('Ctrl Pts',(-1.40411478023519,7.78573092406636,78.2010550960429));
#60417=CARTESIAN_POINT('Ctrl Pts',(-1.08182289928625,7.84081940454443,78.1896091839499));
#60418=CARTESIAN_POINT('Ctrl Pts',(-0.828856897134209,7.87158004969096,
78.1804989140836));
#60419=CARTESIAN_POINT('Ctrl Pts',(-0.459077700770658,7.89852176828448,
78.1664913289405));
#60420=CARTESIAN_POINT('Ctrl Pts',(-0.343123456843648,7.90440794374743,
78.1619977948945));
#60421=CARTESIAN_POINT('Ctrl Pts',(-0.205144416257173,7.90837013854216,
78.1564991474161));
#60422=CARTESIAN_POINT('Ctrl Pts',(-0.183208454968984,7.90890871908443,
78.155620715135));
#60423=CARTESIAN_POINT('Ctrl Pts',(-0.154052257859593,7.90950321003464,
78.1544477278793));
#60424=CARTESIAN_POINT('Ctrl Pts',(-0.14683362647866,7.90964051100411,78.1541568726735));
#60425=CARTESIAN_POINT('Ctrl Pts',(-0.134965396109451,7.90984999642044,
78.1536779591542));
#60426=CARTESIAN_POINT('Ctrl Pts',(-0.130315892847507,7.90992796376515,
78.1534901592951));
#60427=CARTESIAN_POINT('Ctrl Pts',(-0.121295849598588,7.91007126534257,
78.1531254804098));
#60428=CARTESIAN_POINT('Ctrl Pts',(-0.116925317915763,7.91013707693145,
78.1529486225397));
#60429=CARTESIAN_POINT('Ctrl Pts',(-0.106820304696355,7.91028086182249,
78.1525393511727));
#60430=CARTESIAN_POINT('Ctrl Pts',(-0.101085792920875,7.91035622160142,
78.1523068234726));
#60431=CARTESIAN_POINT('Ctrl Pts',(-0.0856753322377926,7.91054197724541,
78.1516812314373));
#60432=CARTESIAN_POINT('Ctrl Pts',(-0.0759992740138839,7.91064085554851,
78.1512876705758));
#60433=CARTESIAN_POINT('Ctrl Pts',(-0.00738691801866201,7.91121609804258,
78.1484916813759));
#60434=CARTESIAN_POINT('Ctrl Pts',(0.051551899159381,7.91105156525361,78.1460623192176));
#60435=CARTESIAN_POINT('Ctrl Pts',(0.85606681164321,7.89981489411712,78.1125703051692));
#60436=CARTESIAN_POINT('Ctrl Pts',(1.59644498514849,7.78404704202496,78.0782842033726));
#60437=CARTESIAN_POINT('Ctrl Pts',(2.66758803932621,7.45707254141298,78.0297598429838));
#60438=CARTESIAN_POINT('Ctrl Pts',(3.01731143721459,7.3225557329619,78.0140221120751));
#60439=CARTESIAN_POINT('Ctrl Pts',(3.38726620545399,7.14923241046205,77.997464356031));
#60440=CARTESIAN_POINT('Ctrl Pts',(3.41821741103616,7.13448569708714,77.9960795401645));
#60441=CARTESIAN_POINT('Ctrl Pts',(3.46141270124571,7.11355966786809,77.9941472607883));
#60442=CARTESIAN_POINT('Ctrl Pts',(3.47373791654928,7.10754908005618,77.9935959509269));
#60443=CARTESIAN_POINT('Ctrl Pts',(3.49470317765288,7.0972574756243,77.9926582172941));
#60444=CARTESIAN_POINT('Ctrl Pts',(3.50335112431588,7.09299266004929,77.9922714259811));
#60445=CARTESIAN_POINT('Ctrl Pts',(3.52046062435258,7.08451602644398,77.9915061979984));
#60446=CARTESIAN_POINT('Ctrl Pts',(3.52892247272547,7.08030483232313,77.9911277474641));
#60447=CARTESIAN_POINT('Ctrl Pts',(3.54921036562249,7.07016278526083,77.9902204024781));
#60448=CARTESIAN_POINT('Ctrl Pts',(3.56102913233528,7.06421740531984,77.9896918406233));
#60449=CARTESIAN_POINT('Ctrl Pts',(3.60029128030229,7.04434318051033,77.9879359861837));
#60450=CARTESIAN_POINT('Ctrl Pts',(3.62766839378471,7.03028379161677,77.9867117078243));
#60451=CARTESIAN_POINT('Ctrl Pts',(4.05965783436255,6.80524234844587,77.967393682055));
#60452=CARTESIAN_POINT('Ctrl Pts',(4.44536444974195,6.55979594754333,77.9502185071955));
#60453=CARTESIAN_POINT('Ctrl Pts',(4.94558274176568,6.1769930124541,77.9271717512549));
#60454=CARTESIAN_POINT('Ctrl Pts',(5.0798786734273,6.0670309761633,77.9208892620471));
#60455=CARTESIAN_POINT('Ctrl Pts',(5.47297596501409,5.72295183978091,77.9020066888085));
#60456=CARTESIAN_POINT('Ctrl Pts',(5.72000420124256,5.47605513487731,77.8894722384593));
#60457=CARTESIAN_POINT('Ctrl Pts',(6.0703907473165,5.07618869416702,77.8695227018381));
#60458=CARTESIAN_POINT('Ctrl Pts',(6.18605461758261,4.934577782092,77.8625133364679));
#60459=CARTESIAN_POINT('Ctrl Pts',(6.31342845790513,4.76710659522269,77.8541458548615));
#60460=CARTESIAN_POINT('Ctrl Pts',(6.33003687807857,4.74503079848753,77.853041340772));
#60461=CARTESIAN_POINT('Ctrl Pts',(6.35121747269816,4.71656859225312,77.8516147840125));
#60462=CARTESIAN_POINT('Ctrl Pts',(6.35589636996666,4.71026156434367,77.8512985113994));
#60463=CARTESIAN_POINT('Ctrl Pts',(6.36341083734249,4.70010068061032,77.8507887136673));
#60464=CARTESIAN_POINT('Ctrl Pts',(6.36625232352464,4.69625119065728,77.8505955127517));
#60465=CARTESIAN_POINT('Ctrl Pts',(6.3716505796384,4.68892402607748,77.8502276494979));
#60466=CARTESIAN_POINT('Ctrl Pts',(6.37420799986258,4.68544683095546,77.8500530231984));
#60467=CARTESIAN_POINT('Ctrl Pts',(6.38002148224989,4.67752896384282,77.8496552615541));
#60468=CARTESIAN_POINT('Ctrl Pts',(6.3832757555163,4.67308698297217,77.8494320266161));
#60469=CARTESIAN_POINT('Ctrl Pts',(6.39167158689314,4.66160180278562,77.8488545950351));
#60470=CARTESIAN_POINT('Ctrl Pts',(6.39680613142137,4.65455350795798,77.8485000048074));
#60471=CARTESIAN_POINT('Ctrl Pts',(6.42730197276014,4.61254547201776,77.8463851956824));
#60472=CARTESIAN_POINT('Ctrl Pts',(6.45238788924219,4.57738755031577,77.8446093100112));
#60473=CARTESIAN_POINT('Ctrl Pts',(6.87938253865093,3.96846926671857,77.8137211143665));
#60474=CARTESIAN_POINT('Ctrl Pts',(7.20360383596858,3.34405568174492,77.7803109243016));
#60475=CARTESIAN_POINT('Ctrl Pts',(7.55247212101249,2.3772335206943,77.733467319325));
#60476=CARTESIAN_POINT('Ctrl Pts',(7.64436688840126,2.06270644022127,77.7188696471438));
#60477=CARTESIAN_POINT('Ctrl Pts',(7.74719008779793,1.607589407616,77.6989104348551));
#60478=CARTESIAN_POINT('Ctrl Pts',(7.77427808397464,1.4710203439894,77.6930636567347));
#60479=CARTESIAN_POINT('Ctrl Pts',(7.80563577354967,1.28769532773097,77.685406343059));
#60480=CARTESIAN_POINT('Ctrl Pts',(7.81311341061418,1.24151843315557,77.6834935913614));
#60481=CARTESIAN_POINT('Ctrl Pts',(7.82326171629309,1.17512247400958,77.6807660694483));
#60482=CARTESIAN_POINT('Ctrl Pts',(7.82626438459986,1.15495562736639,77.6799406271924));
#60483=CARTESIAN_POINT('Ctrl Pts',(7.83144331836407,1.119224518043,77.678483414497));
#60484=CARTESIAN_POINT('Ctrl Pts',(7.83365122691017,1.10366499874473,77.6778506266134));
#60485=CARTESIAN_POINT('Ctrl Pts',(7.83685752771419,1.08057521180894,77.6769142042168));
#60486=CARTESIAN_POINT('Ctrl Pts',(7.83789145560915,1.07304996555702,77.6766094239358));
#60487=CARTESIAN_POINT('Ctrl Pts',(7.83967947706338,1.05989572638289,77.676077380198));
#60488=CARTESIAN_POINT('Ctrl Pts',(7.84043834956631,1.05426739526424,77.675849962723));
#60489=CARTESIAN_POINT('Ctrl Pts',(7.84193762258739,1.04305658311968,77.6753974356517));
#60490=CARTESIAN_POINT('Ctrl Pts',(7.8426781244356,1.03747411958261,77.6751723229211));
#60491=CARTESIAN_POINT('Ctrl Pts',(7.84443099184918,1.02415055701102,77.6746355854301));
#60492=CARTESIAN_POINT('Ctrl Pts',(7.84543786135467,1.01640873343652,77.6743241381114));
#60493=CARTESIAN_POINT('Ctrl Pts',(7.84844404255318,0.993023575417423,77.6733846681491));
#60494=CARTESIAN_POINT('Ctrl Pts',(7.85040804422048,0.977375697179887,77.6727577848543));
#60495=CARTESIAN_POINT('Ctrl Pts',(7.8696245667757,0.820475484113165,77.666489478042));
#60496=CARTESIAN_POINT('Ctrl Pts',(7.8831101623419,0.678783948545217,77.6609708393846));
#60497=CARTESIAN_POINT('Ctrl Pts',(7.89321217839241,0.530250516965052,77.6553186097386));
#60498=CARTESIAN_POINT('Ctrl Pts',(7.89364951669848,0.523699734232348,77.6550695972594));
#60499=CARTESIAN_POINT('Ctrl Pts',(7.94117090326282,-0.201696615509884,
77.627524871233));
#60500=CARTESIAN_POINT('Ctrl Pts',(7.88986275843466,-0.923549114174577,
77.6037352115985));
#60501=CARTESIAN_POINT('Ctrl Pts',(7.73395698996074,-1.66469142808705,77.5778108903933));
#60502=CARTESIAN_POINT('Ctrl Pts',(7.72609163869864,-1.70082222652563,77.5765422039061));
#60503=CARTESIAN_POINT('Ctrl Pts',(7.70902584912639,-1.77665478956118,77.5738670925913));
#60504=CARTESIAN_POINT('Ctrl Pts',(7.6997713593883,-1.81634324041259,77.572459874676));
#60505=CARTESIAN_POINT('Ctrl Pts',(7.67949497124513,-1.90035897647471,77.5694628867353));
#60506=CARTESIAN_POINT('Ctrl Pts',(7.66839501181587,-1.94466581777949,77.5678716589156));
#60507=CARTESIAN_POINT('Ctrl Pts',(7.57272807113169,-2.3129714225212,77.5545384753036));
#60508=CARTESIAN_POINT('Ctrl Pts',(7.46805917087179,-2.63136772578305,77.5423333106155));
#60509=CARTESIAN_POINT('Ctrl Pts',(7.33957161452393,-2.95207112716206,77.5284738619634));
#60510=CARTESIAN_POINT('Ctrl Pts',(7.33557325037546,-2.96199265879721,77.5280435036701));
#60511=CARTESIAN_POINT('Ctrl Pts',(7.32984099370864,-2.97613387113643,77.5274278001698));
#60512=CARTESIAN_POINT('Ctrl Pts',(7.32812353957319,-2.98036024677558,77.5272434902558));
#60513=CARTESIAN_POINT('Ctrl Pts',(7.32514793858423,-2.98766459542355,77.52692443777));
#60514=CARTESIAN_POINT('Ctrl Pts',(7.32389150559794,-2.990743263973,77.526789804038));
#60515=CARTESIAN_POINT('Ctrl Pts',(7.32147126040238,-2.99666297890638,77.5265306251937));
#60516=CARTESIAN_POINT('Ctrl Pts',(7.32030773322601,-2.99950414516599,77.5264060980802));
#60517=CARTESIAN_POINT('Ctrl Pts',(7.31756205014327,-3.00619759590852,77.526112411856));
#60518=CARTESIAN_POINT('Ctrl Pts',(7.31597850708423,-3.01004930642219,77.5259431655809));
#60519=CARTESIAN_POINT('Ctrl Pts',(7.31049188756423,-3.02336470797847,77.525357233144));
#60520=CARTESIAN_POINT('Ctrl Pts',(7.30657349827935,-3.03282203697197,77.5249395923981));
#60521=CARTESIAN_POINT('Ctrl Pts',(7.26277413660642,-3.13795756135698,77.5202805150726));
#60522=CARTESIAN_POINT('Ctrl Pts',(7.22103628742296,-3.23284688478919,77.5159258199844));
#60523=CARTESIAN_POINT('Ctrl Pts',(6.82759351987256,-4.08166350484498,77.4758045933944));
#60524=CARTESIAN_POINT('Ctrl Pts',(6.36087258131209,-4.77656920304409,77.435219030916));
#60525=CARTESIAN_POINT('Ctrl Pts',(5.56804532416279,-5.62950117403064,77.3837615681504));
#60526=CARTESIAN_POINT('Ctrl Pts',(5.32660281141983,-5.85847683406975,77.3696372159281));
#60527=CARTESIAN_POINT('Ctrl Pts',(5.06017875101148,-6.08101369337981,77.3556012863157));
#60528=CARTESIAN_POINT('Ctrl Pts',(5.04888504766168,-6.09039377297291,77.3550089995715));
#60529=CARTESIAN_POINT('Ctrl Pts',(5.03083115031956,-6.10530385935583,77.3540664563381));
#60530=CARTESIAN_POINT('Ctrl Pts',(5.02408782364861,-6.11085418080099,77.3537153526063));
#60531=CARTESIAN_POINT('Ctrl Pts',(5.0112459541367,-6.12138848782573,77.353048510475));
#60532=CARTESIAN_POINT('Ctrl Pts',(5.00514913552611,-6.12637455297636,77.3527326857101));
#60533=CARTESIAN_POINT('Ctrl Pts',(4.99449102271124,-6.13506438001627,77.352181911525));
#60534=CARTESIAN_POINT('Ctrl Pts',(4.98993303486546,-6.13877217614726,77.351946794867));
#60535=CARTESIAN_POINT('Ctrl Pts',(4.9810597443088,-6.14597393853123,77.3514899032317));
#60536=CARTESIAN_POINT('Ctrl Pts',(4.97674488663466,-6.1494684455644,77.3512681059312));
#60537=CARTESIAN_POINT('Ctrl Pts',(4.96654899581844,-6.15770811057429,77.3507448942524));
#60538=CARTESIAN_POINT('Ctrl Pts',(4.96066483053207,-6.16244939471723,77.3504436398686));
#60539=CARTESIAN_POINT('Ctrl Pts',(4.94019038982152,-6.17889875841927,77.3493978146356));
#60540=CARTESIAN_POINT('Ctrl Pts',(4.92556533205801,-6.19056355434743,77.3486550257474));
#60541=CARTESIAN_POINT('Ctrl Pts',(4.75655828216668,-6.32438376377872,77.3401199275047));
#60542=CARTESIAN_POINT('Ctrl Pts',(4.59770441856821,-6.44079167902885,77.3325656292473));
#60543=CARTESIAN_POINT('Ctrl Pts',(3.80355381121651,-6.97837486647673,77.2967810192411));
#60544=CARTESIAN_POINT('Ctrl Pts',(3.11410864959702,-7.31210936672008,77.2721192410177));
#60545=CARTESIAN_POINT('Ctrl Pts',(2.33059918364441,-7.56014579225543,77.243031830625));
#60546=CARTESIAN_POINT('Ctrl Pts',(2.27338622944995,-7.57754655878987,77.2408992192569));
#60547=CARTESIAN_POINT('Ctrl Pts',(2.14326951117135,-7.61551404054068,77.2360191549871));
#60548=CARTESIAN_POINT('Ctrl Pts',(2.07025715466929,-7.63568550983528,77.2332596699371));
#60549=CARTESIAN_POINT('Ctrl Pts',(1.84399728050741,-7.69471166036746,77.2246133085429));
#60550=CARTESIAN_POINT('Ctrl Pts',(1.68987284640951,-7.73002186009024,77.218590258445));
#60551=CARTESIAN_POINT('Ctrl Pts',(1.51210421096783,-7.76517850641759,77.2113873666949));
#60552=CARTESIAN_POINT('Ctrl Pts',(1.48938617109232,-7.76956788976854,77.2104621124243));
#60553=CARTESIAN_POINT('Ctrl Pts',(1.46054722279686,-7.77500876991651,77.209281173533));
#60554=CARTESIAN_POINT('Ctrl Pts',(1.45444372678084,-7.77615284107149,77.2090308749559));
#60555=CARTESIAN_POINT('Ctrl Pts',(1.44464103028577,-7.77797836469603,77.2086282886564));
#60556=CARTESIAN_POINT('Ctrl Pts',(1.44094272873539,-7.77866435838931,77.2084762697823));
#60557=CARTESIAN_POINT('Ctrl Pts',(1.43391147359225,-7.77996339132317,77.2081869977246));
#60558=CARTESIAN_POINT('Ctrl Pts',(1.4305786113852,-7.78057692725982,77.20804977325));
#60559=CARTESIAN_POINT('Ctrl Pts',(1.42299938880114,-7.78196712755142,77.2077374697973));
#60560=CARTESIAN_POINT('Ctrl Pts',(1.41875278787592,-7.78274245761574,77.2075623144046));
#60561=CARTESIAN_POINT('Ctrl Pts',(1.4058779796865,-7.78508220892517,77.2070307591244));
#60562=CARTESIAN_POINT('Ctrl Pts',(1.39724782833438,-7.78663575612422,77.2066737420667));
#60563=CARTESIAN_POINT('Ctrl Pts',(1.33731457122617,-7.79732172928878,77.2041895590107));
#60564=CARTESIAN_POINT('Ctrl Pts',(1.28592594848808,-7.80596122444017,77.2020349878189));
#60565=CARTESIAN_POINT('Ctrl Pts',(1.22847977350406,-7.81503647227574,77.1996020464743));
#60566=CARTESIAN_POINT('Ctrl Pts',(1.22250164093129,-7.81597385835489,77.1993485682365));
#60567=CARTESIAN_POINT('Ctrl Pts',(1.21338518862078,-7.81739262573166,77.1989615799654));
#60568=CARTESIAN_POINT('Ctrl Pts',(1.21024763467186,-7.81787897984678,77.1988283126916));
#60569=CARTESIAN_POINT('Ctrl Pts',(1.20416611463337,-7.81881793113046,77.1985698471283));
#60570=CARTESIAN_POINT('Ctrl Pts',(1.20122218354781,-7.81927075484094,77.1984446598325));
#60571=CARTESIAN_POINT('Ctrl Pts',(1.19262831629414,-7.82058766127101,77.1980790133012));
#60572=CARTESIAN_POINT('Ctrl Pts',(1.18697770738704,-7.82144728233434,77.1978383396742));
#60573=CARTESIAN_POINT('Ctrl Pts',(0.616437759188743,-7.90761039457926,
77.173512217628));
#60574=CARTESIAN_POINT('Ctrl Pts',(0.0439985209837045,-7.93147570018103,
77.1467131300235));
#60575=CARTESIAN_POINT('Ctrl Pts',(-0.885033914973852,-7.86956960938423,
77.1039127658265));
#60576=CARTESIAN_POINT('Ctrl Pts',(-1.24205478758606,-7.82117279129737,
77.0876079380365));
#60577=CARTESIAN_POINT('Ctrl Pts',(-1.83607688144374,-7.69893126866916,
77.061247148098));
#60578=CARTESIAN_POINT('Ctrl Pts',(-2.07514836208777,-7.63796402727584,
77.0508475949108));
#60579=CARTESIAN_POINT('Ctrl Pts',(-2.34883700456367,-7.55436636609084,
77.0391938746435));
#60580=CARTESIAN_POINT('Ctrl Pts',(-2.38659023234631,-7.54252435122402,
77.0375918281125));
#60581=CARTESIAN_POINT('Ctrl Pts',(-2.43491342263068,-7.52696771864853,
77.0355480973403));
#60582=CARTESIAN_POINT('Ctrl Pts',(-2.44556618081232,-7.5235133062868,77.0350979889858));
#60583=CARTESIAN_POINT('Ctrl Pts',(-2.46268796596274,-7.51792094932336,
77.0343752284431));
#60584=CARTESIAN_POINT('Ctrl Pts',(-2.46916161068641,-7.51579725369055,
77.034102114042));
#60585=CARTESIAN_POINT('Ctrl Pts',(-2.48146414867605,-7.5117437641795,77.033583383063));
#60586=CARTESIAN_POINT('Ctrl Pts',(-2.48729355250034,-7.50981554259232,
77.0333377156408));
#60587=CARTESIAN_POINT('Ctrl Pts',(-2.50054644826687,-7.50541469087283,
77.0327794879836));
#60588=CARTESIAN_POINT('Ctrl Pts',(-2.50796853364924,-7.50293782838312,
77.0324670656315));
#60589=CARTESIAN_POINT('Ctrl Pts',(-2.5304704087447,-7.49539149140103,77.0315204962075));
#60590=CARTESIAN_POINT('Ctrl Pts',(-2.5455386333882,-7.4902875224231,77.0308874721892));
#60591=CARTESIAN_POINT('Ctrl Pts',(-2.65051315125114,-7.45437678234964,
77.0264831868576));
#60592=CARTESIAN_POINT('Ctrl Pts',(-2.7398750074953,-7.42199696107769,77.0227635318252));
#60593=CARTESIAN_POINT('Ctrl Pts',(-2.90834175663681,-7.35749644392028,
77.0157992602163));
#60594=CARTESIAN_POINT('Ctrl Pts',(-2.98755197485169,-7.32569037067155,
77.0125453283614));
#60595=CARTESIAN_POINT('Ctrl Pts',(-3.76791252860589,-6.99758174459804,
76.98064994306));
#60596=CARTESIAN_POINT('Ctrl Pts',(-4.42326166250249,-6.60287579068143,
76.9556592818221));
#60597=CARTESIAN_POINT('Ctrl Pts',(-5.15293580172315,-6.00535565591328,
76.922070489555));
#60598=CARTESIAN_POINT('Ctrl Pts',(-5.28971880859796,-5.88522842024651,
76.9154525529069));
#60599=CARTESIAN_POINT('Ctrl Pts',(-5.48644488400944,-5.70005439946176,
76.9052498439001));
#60600=CARTESIAN_POINT('Ctrl Pts',(-5.54964108693638,-5.63854418526118,
76.9018604170419));
#60601=CARTESIAN_POINT('Ctrl Pts',(-5.64481793100041,-5.54275624049307,
76.8965580407421));
#60602=CARTESIAN_POINT('Ctrl Pts',(-5.67754539181419,-5.50922811097333,
76.8946977003734));
#60603=CARTESIAN_POINT('Ctrl Pts',(-5.71547321328777,-5.46967550335932,
76.8924952797971));
#60604=CARTESIAN_POINT('Ctrl Pts',(-5.72096527006593,-5.46393086904646,
76.8921752090447));
#60605=CARTESIAN_POINT('Ctrl Pts',(-5.72933476981539,-5.45515000653364,
76.8916856627141));
#60606=CARTESIAN_POINT('Ctrl Pts',(-5.73221848981751,-5.45211974219841,
76.8915166651458));
#60607=CARTESIAN_POINT('Ctrl Pts',(-5.73745555006345,-5.44660779825621,
76.8912091602321));
#60608=CARTESIAN_POINT('Ctrl Pts',(-5.73980968870466,-5.44412687529991,
76.8910707141094));
#60609=CARTESIAN_POINT('Ctrl Pts',(-5.74452516706089,-5.43915098207734,
76.8907929593604));
#60610=CARTESIAN_POINT('Ctrl Pts',(-5.74688649138818,-5.43665599941061,
76.8906536496043));
#60611=CARTESIAN_POINT('Ctrl Pts',(-5.75362505611544,-5.42952671515151,
76.8902554642953));
#60612=CARTESIAN_POINT('Ctrl Pts',(-5.75799830528626,-5.42488867653322,
76.8899962826315));
#60613=CARTESIAN_POINT('Ctrl Pts',(-5.77684082401892,-5.40485683653253,
76.8888762970128));
#60614=CARTESIAN_POINT('Ctrl Pts',(-5.79125388712421,-5.38941051771656,
76.8880112357019));
#60615=CARTESIAN_POINT('Ctrl Pts',(-5.82285143963137,-5.35527466293965,
76.8860966855741));
#60616=CARTESIAN_POINT('Ctrl Pts',(-5.84000813221957,-5.33655980878101,
76.885045215306));
#60617=CARTESIAN_POINT('Ctrl Pts',(-6.35941796636103,-4.76447300534346,
76.8528573462661));
#60618=CARTESIAN_POINT('Ctrl Pts',(-6.78082511369048,-4.14280706541201,
76.8169543520969));
#60619=CARTESIAN_POINT('Ctrl Pts',(-7.24517762208962,-3.19186364733059,
76.7691194268557));
#60620=CARTESIAN_POINT('Ctrl Pts',(-7.36502395956801,-2.9046583762339,76.7554152809114));
#60621=CARTESIAN_POINT('Ctrl Pts',(-7.50479702961425,-2.50491551185445,
76.737497419901));
#60622=CARTESIAN_POINT('Ctrl Pts',(-7.53966424528285,-2.39792506559273,
76.7328086081913));
#60623=CARTESIAN_POINT('Ctrl Pts',(-7.58974309522077,-2.2323478306801,76.7257146790602));
#60624=CARTESIAN_POINT('Ctrl Pts',(-7.6065839303791,-2.17427188089323,76.7232567440478));
#60625=CARTESIAN_POINT('Ctrl Pts',(-7.62617507491286,-2.10369626548633,
76.7203057239821));
#60626=CARTESIAN_POINT('Ctrl Pts',(-7.62956279183548,-2.09137654622007,
76.7197919115497));
#60627=CARTESIAN_POINT('Ctrl Pts',(-7.63478654515992,-2.0721983057618,76.7189940956143));
#60628=CARTESIAN_POINT('Ctrl Pts',(-7.63664321282725,-2.06534545509644,
76.7187094215359));
#60629=CARTESIAN_POINT('Ctrl Pts',(-7.63989995854664,-2.05326056738466,
76.7182081150941));
#60630=CARTESIAN_POINT('Ctrl Pts',(-7.64130389225151,-2.04802958000643,
76.7179913575842));
#60631=CARTESIAN_POINT('Ctrl Pts',(-7.64449574742573,-2.03608791492415,
76.7174970628489));
#60632=CARTESIAN_POINT('Ctrl Pts',(-7.64628020763725,-2.02937631215187,
76.7172196381558));
#60633=CARTESIAN_POINT('Ctrl Pts',(-7.65106375511801,-2.01128884536766,
76.7164730247647));
#60634=CARTESIAN_POINT('Ctrl Pts',(-7.6540463135995,-1.99990860671062,76.7160043726224));
#60635=CARTESIAN_POINT('Ctrl Pts',(-7.66764989366914,-1.94752664947359,
76.7138522527632));
#60636=CARTESIAN_POINT('Ctrl Pts',(-7.67796700602383,-1.90644634533213,
76.7121786412781));
#60637=CARTESIAN_POINT('Ctrl Pts',(-7.83608378484873,-1.25475255301284,
76.6858475950965));
#60638=CARTESIAN_POINT('Ctrl Pts',(-7.91096433687506,-0.628760618091075,
76.663847643362));
#60639=CARTESIAN_POINT('Ctrl Pts',(-7.91103092760329,0.544851669213203,
76.6235237229675));
#60640=CARTESIAN_POINT('Ctrl Pts',(-7.85468120141728,1.08863886011775,76.6051102215045));
#60641=CARTESIAN_POINT('Ctrl Pts',(-7.72786842137306,1.69391043821135,76.5811806430569));
#60642=CARTESIAN_POINT('Ctrl Pts',(-7.71185886122117,1.76536546050135,76.5782986969197));
#60643=CARTESIAN_POINT('Ctrl Pts',(-7.69284672224997,1.84502182289784,76.5750120948878));
#60644=CARTESIAN_POINT('Ctrl Pts',(-7.69081939515854,1.85345440974454,76.5746632385904));
#60645=CARTESIAN_POINT('Ctrl Pts',(-7.68775477680314,1.86610996493545,76.5741382590911));
#60646=CARTESIAN_POINT('Ctrl Pts',(-7.68672785891327,1.87033545983041,76.5739627388454));
#60647=CARTESIAN_POINT('Ctrl Pts',(-7.68494785482,1.87763347761757,76.5736591770404));
#60648=CARTESIAN_POINT('Ctrl Pts',(-7.684196407808,1.88070640285607,76.5735312315643));
#60649=CARTESIAN_POINT('Ctrl Pts',(-7.68263403905664,1.88707889784916,76.5732656393601));
#60650=CARTESIAN_POINT('Ctrl Pts',(-7.68182283712073,1.89037838639041,76.5731279761796));
#60651=CARTESIAN_POINT('Ctrl Pts',(-7.67990511219554,1.89815693610578,76.5728030884181));
#60652=CARTESIAN_POINT('Ctrl Pts',(-7.67879679726187,1.90263554907473,76.5726157586643));
#60653=CARTESIAN_POINT('Ctrl Pts',(-7.67514910067372,1.91732050017351,76.5720006395713));
#60654=CARTESIAN_POINT('Ctrl Pts',(-7.6725932924125,1.92752270678593,76.5715718938665));
#60655=CARTESIAN_POINT('Ctrl Pts',(-7.58196658609709,2.28624764423388,76.55644811545));
#60656=CARTESIAN_POINT('Ctrl Pts',(-7.47027001484355,2.62833833941774,76.5404304359116));
#60657=CARTESIAN_POINT('Ctrl Pts',(-7.01311817776944,3.76067338391006,76.484672890547));
#60658=CARTESIAN_POINT('Ctrl Pts',(-6.56200708626946,4.50190991946419,76.4442261511919));
#60659=CARTESIAN_POINT('Ctrl Pts',(-5.9932570524005,5.16380703571983,76.4084796968031));
#60660=CARTESIAN_POINT('Ctrl Pts',(-5.98633762539382,5.17182704991676,76.4080464876772));
#60661=CARTESIAN_POINT('Ctrl Pts',(-5.94863734918117,5.21534681269649,76.405695277769));
#60662=CARTESIAN_POINT('Ctrl Pts',(-5.91755648903749,5.2505860614261,76.4037898234488));
#60663=CARTESIAN_POINT('Ctrl Pts',(-5.87802031141662,5.29461488268659,76.4014067367755));
#60664=CARTESIAN_POINT('Ctrl Pts',(-5.86985649332964,5.30366423209943,76.400916807445));
#60665=CARTESIAN_POINT('Ctrl Pts',(-5.85695893555927,5.31789453413708,76.4001461721181));
#60666=CARTESIAN_POINT('Ctrl Pts',(-5.85223917469671,5.32308809728988,76.3998648727266));
#60667=CARTESIAN_POINT('Ctrl Pts',(-5.84389012029176,5.33225076184958,76.3993685140027));
#60668=CARTESIAN_POINT('Ctrl Pts',(-5.84026368171439,5.33622245164899,76.3991533332963));
#60669=CARTESIAN_POINT('Ctrl Pts',(-5.83195031299158,5.34530866014916,76.398660992285));
#60670=CARTESIAN_POINT('Ctrl Pts',(-5.82726069680937,5.35042072151442,76.398383946943));
#60671=CARTESIAN_POINT('Ctrl Pts',(-5.8143349469063,5.36447368325589,76.3976222255312));
#60672=CARTESIAN_POINT('Ctrl Pts',(-5.80608490426132,5.37340179582522,76.3971381455345));
#60673=CARTESIAN_POINT('Ctrl Pts',(-5.76220351911996,5.42067073428612,76.3945744343269));
#60674=CARTESIAN_POINT('Ctrl Pts',(-5.72621251195026,5.45867667180154,76.3925103242929));
#60675=CARTESIAN_POINT('Ctrl Pts',(-5.28202823152216,5.9185005093116,76.3674949553914));
#60676=CARTESIAN_POINT('Ctrl Pts',(-4.82846832864452,6.29400039735428,76.3468243301362));
#60677=CARTESIAN_POINT('Ctrl Pts',(-4.26928906247498,6.66061181377203,76.3238096190381));
#60678=CARTESIAN_POINT('Ctrl Pts',(-4.2003635546563,6.70429152609681,76.3210078212627));
#60679=CARTESIAN_POINT('Ctrl Pts',(-3.71428837588567,7.00189010659934,76.3014260536155));
#60680=CARTESIAN_POINT('Ctrl Pts',(-3.27512396270644,7.21774716902434,76.284685054587));
#60681=CARTESIAN_POINT('Ctrl Pts',(-2.75310897012774,7.41682365016354,76.2630381751009));
#60682=CARTESIAN_POINT('Ctrl Pts',(-2.68696702781521,7.44104090217362,76.2602638890925));
#60683=CARTESIAN_POINT('Ctrl Pts',(-2.61153521098281,7.46752270597455,76.2570552456935));
#60684=CARTESIAN_POINT('Ctrl Pts',(-2.60255238830475,7.47065810937037,76.2566724280423));
#60685=CARTESIAN_POINT('Ctrl Pts',(-2.58942588361466,7.47521329321921,76.2561119477288));
#60686=CARTESIAN_POINT('Ctrl Pts',(-2.58528661520565,7.47664585913675,76.2559350521128));
#60687=CARTESIAN_POINT('Ctrl Pts',(-2.57795814105536,7.47917536880392,76.255621583945));
#60688=CARTESIAN_POINT('Ctrl Pts',(-2.57476942792706,7.4802737093875,76.2554850964492));
#60689=CARTESIAN_POINT('Ctrl Pts',(-2.56812103566069,7.48255896897828,76.2552003274779));
#60690=CARTESIAN_POINT('Ctrl Pts',(-2.56466125340506,7.48374552167812,76.2550520253291));
#60691=CARTESIAN_POINT('Ctrl Pts',(-2.55566773967461,7.48682293112151,76.2546662383284));
#60692=CARTESIAN_POINT('Ctrl Pts',(-2.5501327407928,7.4887100492387,76.2544285292496));
#60693=CARTESIAN_POINT('Ctrl Pts',(-2.52647354730777,7.49674720960121,76.2534112732783));
#60694=CARTESIAN_POINT('Ctrl Pts',(-2.50832929238517,7.50283756047676,76.2526281934953));
#60695=CARTESIAN_POINT('Ctrl Pts',(-2.38144177708253,7.54491725658579,76.2471322985383));
#60696=CARTESIAN_POINT('Ctrl Pts',(-2.2719545875228,7.5786055071434,76.2422897076891));
#60697=CARTESIAN_POINT('Ctrl Pts',(-1.99129955984922,7.65833244825229,76.2296939089449));
#60698=CARTESIAN_POINT('Ctrl Pts',(-1.81924749826317,7.7010169899037,76.221802413683));
#60699=CARTESIAN_POINT('Ctrl Pts',(-1.24858961316317,7.82240090960169,76.1953896018029));
#60700=CARTESIAN_POINT('Ctrl Pts',(-0.845346381885203,7.87618717279358,
76.1763808516215));
#60701=CARTESIAN_POINT('Ctrl Pts',(-0.0524279349411913,7.92033205965817,
76.1400141756224));
#60702=CARTESIAN_POINT('Ctrl Pts',(0.335988121549553,7.91337914540182,76.1226709526148));
#60703=CARTESIAN_POINT('Ctrl Pts',(0.730419857845168,7.87721228461404,76.1058418754191));
#60704=CARTESIAN_POINT('Ctrl Pts',(0.738480974833161,7.87646065162174,76.1054982529992));
#60705=CARTESIAN_POINT('Ctrl Pts',(0.747697171325159,7.87558704407975,76.1051057574976));
#60706=CARTESIAN_POINT('Ctrl Pts',(0.748853379456794,7.8754771896668,76.1050565239552));
#60707=CARTESIAN_POINT('Ctrl Pts',(0.751450851169223,7.87522981978477,76.1049459334155));
#60708=CARTESIAN_POINT('Ctrl Pts',(0.752892101442853,7.87509216325358,76.1048845806217));
#60709=CARTESIAN_POINT('Ctrl Pts',(0.756561700810109,7.87474065630967,76.1047283948918));
#60710=CARTESIAN_POINT('Ctrl Pts',(0.758789997768888,7.87452625562743,76.1046335783665));
#60711=CARTESIAN_POINT('Ctrl Pts',(0.768390624197728,7.87359839646967,76.1042251661423));
#60712=CARTESIAN_POINT('Ctrl Pts',(0.775762052464235,7.87287552921991,76.1039118515696));
#60713=CARTESIAN_POINT('Ctrl Pts',(0.783976663102461,7.87205832749158,76.1035629965723));
#60714=CARTESIAN_POINT('Ctrl Pts',(0.784820845080389,7.87197420986925,76.103527149679));
#60715=CARTESIAN_POINT('Ctrl Pts',(0.787937608118689,7.87166313696443,76.1033948140748));
#60716=CARTESIAN_POINT('Ctrl Pts',(0.790210105469669,7.87143533323863,76.1032983508473));
#60717=CARTESIAN_POINT('Ctrl Pts',(0.794601676099962,7.87099318464625,76.1031119861319));
#60718=CARTESIAN_POINT('Ctrl Pts',(0.796720761930482,7.87077896805181,76.1030220807951));
#60719=CARTESIAN_POINT('Ctrl Pts',(0.951891240965182,7.85502960749803,76.0964403657639));
#60720=CARTESIAN_POINT('Ctrl Pts',(1.10446199005023,7.8350337787864,76.090085412071));
#60721=CARTESIAN_POINT('Ctrl Pts',(1.27427718356294,7.80771849112803,76.0831379208332));
#60722=CARTESIAN_POINT('Ctrl Pts',(1.29218571475534,7.80477459389872,76.0824068040235));
#60723=CARTESIAN_POINT('Ctrl Pts',(1.3173499220342,7.80054898482547,76.0813816402843));
#60724=CARTESIAN_POINT('Ctrl Pts',(1.32461411284663,7.79931873525908,76.0810859587343));
#60725=CARTESIAN_POINT('Ctrl Pts',(1.33794107399107,7.79704255044026,76.0805439621214));
#60726=CARTESIAN_POINT('Ctrl Pts',(1.34400435967317,7.79599968780535,76.0802975495607));
#60727=CARTESIAN_POINT('Ctrl Pts',(1.35629231726226,7.79387144329037,76.0797985215067));
#60728=CARTESIAN_POINT('Ctrl Pts',(1.36251691813998,7.7927856747394,76.0795459185151));
#60729=CARTESIAN_POINT('Ctrl Pts',(1.37784156025916,7.79009364676491,76.0789244770313));
#60730=CARTESIAN_POINT('Ctrl Pts',(1.38694011108493,7.78847889639276,76.078555908932));
#60731=CARTESIAN_POINT('Ctrl Pts',(1.42011563729916,7.78253114678753,76.0772134479337));
#60732=CARTESIAN_POINT('Ctrl Pts',(1.44417542353122,7.77810239286138,76.0762426040216));
#60733=CARTESIAN_POINT('Ctrl Pts',(1.79330018745065,7.71216222189318,76.062193984688));
#60734=CARTESIAN_POINT('Ctrl Pts',(2.11422722910587,7.63042869234352,76.0497924107294));
#60735=CARTESIAN_POINT('Ctrl Pts',(2.77367472250375,7.41766322184181,76.0248025824101));
#60736=CARTESIAN_POINT('Ctrl Pts',(3.11020133460932,7.28297033385233,76.0123388024757));
#60737=CARTESIAN_POINT('Ctrl Pts',(3.70035690335582,6.99837174232747,75.9897670428475));
#60738=CARTESIAN_POINT('Ctrl Pts',(3.95710285748966,6.85646953993599,75.9796717739896));
#60739=CARTESIAN_POINT('Ctrl Pts',(4.42447690235314,6.56314261721425,75.9598278449249));
#60740=CARTESIAN_POINT('Ctrl Pts',(4.63668852769994,6.41497747435768,75.9501865415141));
#60741=CARTESIAN_POINT('Ctrl Pts',(4.85386200813806,6.24693517836117,75.9392187924459));
#60742=CARTESIAN_POINT('Ctrl Pts',(4.86644981759778,6.23713409207241,75.9385789798622));
#60743=CARTESIAN_POINT('Ctrl Pts',(4.88348785604352,6.22378500200706,75.9377072701521));
#60744=CARTESIAN_POINT('Ctrl Pts',(4.88796410194713,6.22027011705225,75.9374777178803));
#60745=CARTESIAN_POINT('Ctrl Pts',(4.89503247860295,6.21470747066456,75.9371143805708));
#60746=CARTESIAN_POINT('Ctrl Pts',(4.89762713078323,6.2126629073401,75.9369808246781));
#60747=CARTESIAN_POINT('Ctrl Pts',(4.90265712096098,6.20869420953345,75.9367215606518));
#60748=CARTESIAN_POINT('Ctrl Pts',(4.9050926103238,6.20677026458069,75.9365958660512));
#60749=CARTESIAN_POINT('Ctrl Pts',(4.91082284929944,6.20223811224287,75.9362997539038));
#60750=CARTESIAN_POINT('Ctrl Pts',(4.91411665260809,6.1996287132856,75.9361292518156));
#60751=CARTESIAN_POINT('Ctrl Pts',(4.92378295818904,6.19195838185046,75.9356280216759));
#60752=CARTESIAN_POINT('Ctrl Pts',(4.93014971639758,6.18689025237377,75.9352967867975));
#60753=CARTESIAN_POINT('Ctrl Pts',(4.94458275210689,6.17536469943577,75.9345434280883));
#60754=CARTESIAN_POINT('Ctrl Pts',(4.95264420849895,6.16890128837062,75.9341208887497));
#60755=CARTESIAN_POINT('Ctrl Pts',(5.30872120493341,5.88226259233086,75.9153802750712));
#60756=CARTESIAN_POINT('Ctrl Pts',(5.63236209333266,5.57314642905344,75.895128047366));
#60757=CARTESIAN_POINT('Ctrl Pts',(5.97250322988178,5.18821857395531,75.8715688587952));
#60758=CARTESIAN_POINT('Ctrl Pts',(6.01621341142032,5.1374685356768,75.8684917593541));
#60759=CARTESIAN_POINT('Ctrl Pts',(6.22048375360702,4.89411646452558,75.8538912740486));
#60760=CARTESIAN_POINT('Ctrl Pts',(6.37247529847644,4.69450297824402,75.8423725990371));
#60761=CARTESIAN_POINT('Ctrl Pts',(6.77575330470779,4.10910957999597,75.8102870633667));
#60762=CARTESIAN_POINT('Ctrl Pts',(7.00324531293333,3.70813424096044,75.7903119644353));
#60763=CARTESIAN_POINT('Ctrl Pts',(7.20774183315733,3.26088579358375,75.7703369358526));
#60764=CARTESIAN_POINT('Ctrl Pts',(7.22070291602865,3.23208414503129,75.769059958138));
#60765=CARTESIAN_POINT('Ctrl Pts',(7.23782292867703,3.19342366424338,75.7673582637505));
#60766=CARTESIAN_POINT('Ctrl Pts',(7.24213475135818,3.18363309609588,75.7669283775652));
#60767=CARTESIAN_POINT('Ctrl Pts',(7.24884625958942,3.16830952977511,75.7662571965326));
#60768=CARTESIAN_POINT('Ctrl Pts',(7.25125949266104,3.1627824999397,75.7660154442922));
#60769=CARTESIAN_POINT('Ctrl Pts',(7.25586583459554,3.15219960688778,75.765553187832));
#60770=CARTESIAN_POINT('Ctrl Pts',(7.25805998465954,3.14714420237679,75.7653326485742));
#60771=CARTESIAN_POINT('Ctrl Pts',(7.26318054237733,3.13531240740026,75.764817143518));
#60772=CARTESIAN_POINT('Ctrl Pts',(7.26610275449806,3.1285342006477,75.7645223192532));
#60773=CARTESIAN_POINT('Ctrl Pts',(7.27445161075847,3.10909384558267,75.7636781677722));
#60774=CARTESIAN_POINT('Ctrl Pts',(7.27985468505086,3.09642157092452,75.7631296341863));
#60775=CARTESIAN_POINT('Ctrl Pts',(7.31459032204418,3.01435975243527,75.7595886132279));
#60776=CARTESIAN_POINT('Ctrl Pts',(7.34296399785464,2.94456727066848,75.7566284133959));
#60777=CARTESIAN_POINT('Ctrl Pts',(7.42336899314471,2.7383968500386,75.7480281542163));
#60778=CARTESIAN_POINT('Ctrl Pts',(7.47262896743741,2.60096970177034,75.7424794197113));
#60779=CARTESIAN_POINT('Ctrl Pts',(7.59788202095205,2.21853148042592,75.7274809045449));
#60780=CARTESIAN_POINT('Ctrl Pts',(7.66580767061685,1.97106452192522,75.7182715523887));
#60781=CARTESIAN_POINT('Ctrl Pts',(7.84571908143169,1.16372910922274,75.6892059852111));
#60782=CARTESIAN_POINT('Ctrl Pts',(7.90920345579479,0.59497934499948,75.6703152001558));
#60783=CARTESIAN_POINT('Ctrl Pts',(7.91135931281254,-0.104364926786781,
75.64489712916));
#60784=CARTESIAN_POINT('Ctrl Pts',(7.90861295650032,-0.233103098924084,
75.6401214088781));
#60785=CARTESIAN_POINT('Ctrl Pts',(7.89803930332656,-0.464117396627604,
75.6312935212535));
#60786=CARTESIAN_POINT('Ctrl Pts',(7.89136229312373,-0.566418023908654,
75.6272929952555));
#60787=CARTESIAN_POINT('Ctrl Pts',(7.88179749672174,-0.679193035796358,
75.6227551933064));
#60788=CARTESIAN_POINT('Ctrl Pts',(7.88087381629139,-0.689828129933893,
75.6223260057941));
#60789=CARTESIAN_POINT('Ctrl Pts',(7.87955566729525,-0.704656815517333,
75.6217257919629));
#60790=CARTESIAN_POINT('Ctrl Pts',(7.87917936787542,-0.708852051123079,
75.6215557834132));
#60791=CARTESIAN_POINT('Ctrl Pts',(7.87851545229675,-0.716187974345506,
75.621258148387));
#60792=CARTESIAN_POINT('Ctrl Pts',(7.87822930790469,-0.719328797345784,
75.6211306050201));
#60793=CARTESIAN_POINT('Ctrl Pts',(7.87762499826165,-0.725918302168633,
75.6208627779526));
#60794=CARTESIAN_POINT('Ctrl Pts',(7.87730644645747,-0.729366946869954,
75.6207224723322));
#60795=CARTESIAN_POINT('Ctrl Pts',(7.87655108453428,-0.737486283894132,
75.6203918176643));
#60796=CARTESIAN_POINT('Ctrl Pts',(7.87611238428003,-0.74215680039298,75.6202013604028));
#60797=CARTESIAN_POINT('Ctrl Pts',(7.87462355042127,-0.757857310206448,
75.6195602552951));
#60798=CARTESIAN_POINT('Ctrl Pts',(7.87355440395534,-0.768885432985613,
75.6191085148364));
#60799=CARTESIAN_POINT('Ctrl Pts',(7.8709542304535,-0.795131711828499,75.6180300704666));
#60800=CARTESIAN_POINT('Ctrl Pts',(7.86940223501198,-0.810347699760125,
75.6174021889463));
#60801=CARTESIAN_POINT('Ctrl Pts',(7.85120809196158,-0.983742928767514,
75.6102175097682));
#60802=CARTESIAN_POINT('Ctrl Pts',(7.82984422872752,-1.14138172175509,75.6034052790451));
#60803=CARTESIAN_POINT('Ctrl Pts',(7.75348784949516,-1.60035437304463,75.5829698854906));
#60804=CARTESIAN_POINT('Ctrl Pts',(7.68573296522575,-1.89926302227668,75.5689040332123));
#60805=CARTESIAN_POINT('Ctrl Pts',(7.39357992036319,-2.91163099549431,75.5202142548614));
#60806=CARTESIAN_POINT('Ctrl Pts',(7.08554873456032,-3.59694727208695,75.4858731925408));
#60807=CARTESIAN_POINT('Ctrl Pts',(6.65912607762144,-4.27111910674453,75.4532711949426));
#60808=CARTESIAN_POINT('Ctrl Pts',(6.63201142187113,-4.31310133950437,75.451243911244));
#60809=CARTESIAN_POINT('Ctrl Pts',(6.59831674744036,-4.36420248013499,75.4487795160396));
#60810=CARTESIAN_POINT('Ctrl Pts',(6.59211308495563,-4.37356745274508,75.4483280160249));
#60811=CARTESIAN_POINT('Ctrl Pts',(6.58183495229566,-4.3890116447487,75.4475836411606));
#60812=CARTESIAN_POINT('Ctrl Pts',(6.5777719660684,-4.39509846531191,75.4472903253074));
#60813=CARTESIAN_POINT('Ctrl Pts',(6.5704246709892,-4.40607254985559,75.4467615957527));
#60814=CARTESIAN_POINT('Ctrl Pts',(6.56714334333645,-4.4109617976134,75.4465260674801));
#60815=CARTESIAN_POINT('Ctrl Pts',(6.5601227918356,-4.42139736953882,75.4460234308395));
#60816=CARTESIAN_POINT('Ctrl Pts',(6.55638198478108,-4.42694262592752,75.4457563838443));
#60817=CARTESIAN_POINT('Ctrl Pts',(6.54626591208577,-4.44189743144858,75.4450363107336));
#60818=CARTESIAN_POINT('Ctrl Pts',(6.53987738272898,-4.45129801333657,75.4445837979134));
#60819=CARTESIAN_POINT('Ctrl Pts',(6.50849644328835,-4.49726099675213,75.4423718771911));
#60820=CARTESIAN_POINT('Ctrl Pts',(6.48321733072806,-4.53362719579732,75.4406236141858));
#60821=CARTESIAN_POINT('Ctrl Pts',(6.27526581947524,-4.82748704189991,75.4265084870423));
#60822=CARTESIAN_POINT('Ctrl Pts',(6.07762808678988,-5.07405683920033,75.4147565016945));
#60823=CARTESIAN_POINT('Ctrl Pts',(5.80368840844783,-5.37677241885671,75.4001206645649));
#60824=CARTESIAN_POINT('Ctrl Pts',(5.74041000221317,-5.44427903577735,75.3968409184733));
#60825=CARTESIAN_POINT('Ctrl Pts',(5.62629390718222,-5.56181820721542,75.3910844396402));
#60826=CARTESIAN_POINT('Ctrl Pts',(5.57593688839234,-5.61230192217494,75.3885962975681));
#60827=CARTESIAN_POINT('Ctrl Pts',(5.46668339485634,-5.71890816891238,75.3832972037355));
#60828=CARTESIAN_POINT('Ctrl Pts',(5.40758981018975,-5.77481693021322,75.3804904811321));
#60829=CARTESIAN_POINT('Ctrl Pts',(5.04923642458443,-6.10353229848063,75.3637708875067));
#60830=CARTESIAN_POINT('Ctrl Pts',(4.73026516454419,-6.3539327855739,75.3501501401085));
#60831=CARTESIAN_POINT('Ctrl Pts',(4.17396304345769,-6.72544968805596,75.3262309813327));
#60832=CARTESIAN_POINT('Ctrl Pts',(3.94719468742527,-6.86099648426533,75.3164302476946));
#60833=CARTESIAN_POINT('Ctrl Pts',(3.69953787795537,-6.99268277112885,75.305226755931));
#60834=CARTESIAN_POINT('Ctrl Pts',(3.68495606507433,-7.00037796397623,75.3045653103867));
#60835=CARTESIAN_POINT('Ctrl Pts',(3.66534051668494,-7.01065131641605,75.303672982764));
#60836=CARTESIAN_POINT('Ctrl Pts',(3.66032782689947,-7.01326979253774,75.3034447285799));
#60837=CARTESIAN_POINT('Ctrl Pts',(3.65246907561156,-7.01736424381077,75.303086522711));
#60838=CARTESIAN_POINT('Ctrl Pts',(3.64962490885851,-7.01884387226221,75.3029568112737));
#60839=CARTESIAN_POINT('Ctrl Pts',(3.64417083803523,-7.02167704661222,75.3027079310689));
#60840=CARTESIAN_POINT('Ctrl Pts',(3.64156107665035,-7.02303086770143,75.3025887805192));
#60841=CARTESIAN_POINT('Ctrl Pts',(3.6361888811896,-7.02581390972235,75.302343380466));
#60842=CARTESIAN_POINT('Ctrl Pts',(3.63342636521468,-7.02724295312075,75.30221711961));
#60843=CARTESIAN_POINT('Ctrl Pts',(3.62504065297781,-7.03157459675625,75.3018336391608));
#60844=CARTESIAN_POINT('Ctrl Pts',(3.61941482702038,-7.03447207365111,75.3015760809706));
#60845=CARTESIAN_POINT('Ctrl Pts',(3.59126332088931,-7.04892827109666,75.300285850591));
#60846=CARTESIAN_POINT('Ctrl Pts',(3.56868595416626,-7.06038543869717,75.2992465659487));
#60847=CARTESIAN_POINT('Ctrl Pts',(3.50642266352921,-7.09160677824048,75.2963688763414));
#60848=CARTESIAN_POINT('Ctrl Pts',(3.46662546119993,-7.11114578384441,75.2945166545636));
#60849=CARTESIAN_POINT('Ctrl Pts',(3.33122992056975,-7.17621348561152,75.2881772519894));
#60850=CARTESIAN_POINT('Ctrl Pts',(3.23488528060808,-7.2201556972113,75.2836028038682));
#60851=CARTESIAN_POINT('Ctrl Pts',(2.92015971360336,-7.35613634603328,75.2685262451957));
#60852=CARTESIAN_POINT('Ctrl Pts',(2.69852466385739,-7.44029759439141,75.2577073136242));
#60853=CARTESIAN_POINT('Ctrl Pts',(1.64646644903902,-7.78659670313505,75.2064485383649));
#60854=CARTESIAN_POINT('Ctrl Pts',(0.779935994600486,-7.92049991186082,
75.1653840525867));
#60855=CARTESIAN_POINT('Ctrl Pts',(-0.104235593133335,-7.91032427355923,
75.1291093696334));
#60856=CARTESIAN_POINT('Ctrl Pts',(-0.117431775338263,-7.91013937627933,
75.1285690169856));
#60857=CARTESIAN_POINT('Ctrl Pts',(-0.177726048414574,-7.90914365352843,
75.1261048536175));
#60858=CARTESIAN_POINT('Ctrl Pts',(-0.224817258285966,-7.9079451935394,
75.1241935245935));
#60859=CARTESIAN_POINT('Ctrl Pts',(-0.28398466931383,-7.9059104490268,75.1218083076549));
#60860=CARTESIAN_POINT('Ctrl Pts',(-0.29607288721056,-7.90546697973152,
75.1213218478521));
#60861=CARTESIAN_POINT('Ctrl Pts',(-0.315095389034554,-7.90472542644363,
75.120557667594));
#60862=CARTESIAN_POINT('Ctrl Pts',(-0.322030354513464,-7.90444594027644,
75.1202793518456));
#60863=CARTESIAN_POINT('Ctrl Pts',(-0.33426625666628,-7.90393669143006,
75.1197887872038));
#60864=CARTESIAN_POINT('Ctrl Pts',(-0.33956734171407,-7.90371072174731,
75.1195764170383));
#60865=CARTESIAN_POINT('Ctrl Pts',(-0.351690188410239,-7.90318174151913,
75.1190911254828));
#60866=CARTESIAN_POINT('Ctrl Pts',(-0.358511797594762,-7.90287523116757,
75.118818316255));
#60867=CARTESIAN_POINT('Ctrl Pts',(-0.377241562963671,-7.90200935963912,
75.118070008549));
#60868=CARTESIAN_POINT('Ctrl Pts',(-0.389148887442308,-7.90143191210849,
75.1175950889263));
#60869=CARTESIAN_POINT('Ctrl Pts',(-0.451672982941602,-7.89825811867552,
75.1151055641147));
#60870=CARTESIAN_POINT('Ctrl Pts',(-0.502265787237247,-7.89520227700313,
75.1131056716775));
#60871=CARTESIAN_POINT('Ctrl Pts',(-0.642360652955859,-7.88538835573283,
75.1076064626397));
#60872=CARTESIAN_POINT('Ctrl Pts',(-0.731783370383624,-7.8775929365302,
75.1041401301939));
#60873=CARTESIAN_POINT('Ctrl Pts',(-1.18932543569304,-7.82984835134208,
75.0866057585264));
#60874=CARTESIAN_POINT('Ctrl Pts',(-1.55445774395648,-7.76561068144842,
75.0733116577115));
#60875=CARTESIAN_POINT('Ctrl Pts',(-1.98298535629342,-7.6587713932111,75.0578931998984));
#60876=CARTESIAN_POINT('Ctrl Pts',(-2.05196868312361,-7.64057817223776,
75.0554159152606));
#60877=CARTESIAN_POINT('Ctrl Pts',(-2.17814629308361,-7.60546880220136,
75.0508834753753));
#60878=CARTESIAN_POINT('Ctrl Pts',(-2.23541330157723,-7.58883419133082,
75.0488259019974));
#60879=CARTESIAN_POINT('Ctrl Pts',(-2.34137885466724,-7.55675033467469,
75.0450114055189));
#60880=CARTESIAN_POINT('Ctrl Pts',(-2.39012632043474,-7.54147377792694,
75.0432537547265));
#60881=CARTESIAN_POINT('Ctrl Pts',(-2.48102910153206,-7.51201660025889,
75.0399665480035));
#60882=CARTESIAN_POINT('Ctrl Pts',(-2.52321939565732,-7.49795056559365,
75.038436970822));
#60883=CARTESIAN_POINT('Ctrl Pts',(-2.60234336095535,-7.47082755863067,
75.0355581140971));
#60884=CARTESIAN_POINT('Ctrl Pts',(-2.63930300812443,-7.45785056188197,
75.0342091171041));
#60885=CARTESIAN_POINT('Ctrl Pts',(-2.70894169459582,-7.43281703365264,
75.0316572351446));
#60886=CARTESIAN_POINT('Ctrl Pts',(-2.74164045856353,-7.42081813198745,
75.030454751985));
#60887=CARTESIAN_POINT('Ctrl Pts',(-2.80353748768815,-7.39763989381527,
75.0281689269075));
#60888=CARTESIAN_POINT('Ctrl Pts',(-2.83275080869563,-7.38650264271761,
75.0270860128218));
#60889=CARTESIAN_POINT('Ctrl Pts',(-3.13260035774982,-7.27014790305459,
75.0159227205949));
#60890=CARTESIAN_POINT('Ctrl Pts',(-3.39730119123685,-7.15028406115013,
75.0056691052768));
#60891=CARTESIAN_POINT('Ctrl Pts',(-3.68077168369177,-7.00262082970465,
74.9936781594259));
#60892=CARTESIAN_POINT('Ctrl Pts',(-3.70666949180692,-6.98894698226858,
74.9925730224812));
#60893=CARTESIAN_POINT('Ctrl Pts',(-3.74013292644046,-6.97104022530597,
74.9911317850525));
#60894=CARTESIAN_POINT('Ctrl Pts',(-3.74776855564842,-6.96693813541936,
74.9908020274796));
#60895=CARTESIAN_POINT('Ctrl Pts',(-3.8503748658589,-6.91159744346697,74.9863585123374));
#60896=CARTESIAN_POINT('Ctrl Pts',(-3.94428248660473,-6.85844012443397,
74.9821458431518));
#60897=CARTESIAN_POINT('Ctrl Pts',(-4.04775740123271,-6.79703870023905,
74.9773250776704));
#60898=CARTESIAN_POINT('Ctrl Pts',(-4.05841710340704,-6.79067932418798,
74.9768264024764));
#60899=CARTESIAN_POINT('Ctrl Pts',(-4.07393093269104,-6.78137449146389,
74.9760976950002));
#60900=CARTESIAN_POINT('Ctrl Pts',(-4.07879696111116,-6.77844883344216,
74.9758687063703));
#60901=CARTESIAN_POINT('Ctrl Pts',(-4.08738891322262,-6.77327039395603,
74.9754636365002));
#60902=CARTESIAN_POINT('Ctrl Pts',(-4.09111613864862,-6.77101976791924,
74.9752876675537));
#60903=CARTESIAN_POINT('Ctrl Pts',(-4.09828881182738,-6.76668057825193,
74.974948557979));
#60904=CARTESIAN_POINT('Ctrl Pts',(-4.10173452665601,-6.76459245675534,
74.9747854401871));
#60905=CARTESIAN_POINT('Ctrl Pts',(-4.1108183713586,-6.75907810617024,74.9743548624282));
#60906=CARTESIAN_POINT('Ctrl Pts',(-4.11645380526456,-6.75564745944821,
74.9740871764412));
#60907=CARTESIAN_POINT('Ctrl Pts',(-4.1370857341212,-6.74305209203146,74.9731050978656));
#60908=CARTESIAN_POINT('Ctrl Pts',(-4.15205589551518,-6.73384449781604,
74.9723885428181));
#60909=CARTESIAN_POINT('Ctrl Pts',(-4.18873808529172,-6.71111380758679,
74.9706231659168));
#60910=CARTESIAN_POINT('Ctrl Pts',(-4.21041536223115,-6.69753519902802,
74.9695716522344));
#60911=CARTESIAN_POINT('Ctrl Pts',(-4.29302091828066,-6.64523169352483,
74.9655339961701));
#60912=CARTESIAN_POINT('Ctrl Pts',(-4.35348291586055,-6.60577920840755,
74.9625146294311));
#60913=CARTESIAN_POINT('Ctrl Pts',(-4.56908180229136,-6.46085158897698,
74.9515367832989));
#60914=CARTESIAN_POINT('Ctrl Pts',(-4.72099179277314,-6.35069630305085,
74.9434031101507));
#60915=CARTESIAN_POINT('Ctrl Pts',(-5.55097487494354,-5.70259842359616,
74.8971918493891));
#60916=CARTESIAN_POINT('Ctrl Pts',(-6.14124528887608,-5.06147289441774,
74.8582868142302));
#60917=CARTESIAN_POINT('Ctrl Pts',(-6.64278342095406,-4.29648135388938,
74.8210643351798));
#60918=CARTESIAN_POINT('Ctrl Pts',(-6.66927693366555,-4.25524016472949,
74.819079406937));
#60919=CARTESIAN_POINT('Ctrl Pts',(-6.70411899956952,-4.19987836421536,
74.8164430323171));
#60920=CARTESIAN_POINT('Ctrl Pts',(-6.71280920198177,-4.18597449289266,
74.8157832659632));
#60921=CARTESIAN_POINT('Ctrl Pts',(-6.72631012120633,-4.16422356131286,
74.8147547644515));
#60922=CARTESIAN_POINT('Ctrl Pts',(-6.73115045926393,-4.15639497767591,
74.8143853165966));
#60923=CARTESIAN_POINT('Ctrl Pts',(-6.74080623654395,-4.14071697686919,
74.8136468879669));
#60924=CARTESIAN_POINT('Ctrl Pts',(-6.7456216577009,-4.13286755810954,74.8132779073677));
#60925=CARTESIAN_POINT('Ctrl Pts',(-6.75638826830701,-4.11524840460448,
74.8124512964852));
#60926=CARTESIAN_POINT('Ctrl Pts',(-6.76233199963502,-4.10547412503793,
74.8119938451033));
#60927=CARTESIAN_POINT('Ctrl Pts',(-6.77962761495663,-4.07689256413663,
74.8106594256318));
#60928=CARTESIAN_POINT('Ctrl Pts',(-6.79092241522967,-4.05805080474741,
74.809783827594));
#60929=CARTESIAN_POINT('Ctrl Pts',(-6.87311044619286,-3.91964230434996,
74.8033815789275));
#60930=CARTESIAN_POINT('Ctrl Pts',(-6.94092116008519,-3.79827040802802,
74.7979301556462));
#60931=CARTESIAN_POINT('Ctrl Pts',(-7.15243665818085,-3.39508606202152,
74.780317024785));
#60932=CARTESIAN_POINT('Ctrl Pts',(-7.28244750168348,-3.1064339610442,74.7684931771233));
#60933=CARTESIAN_POINT('Ctrl Pts',(-7.58368703654001,-2.31390287227634,
74.7374098427156));
#60934=CARTESIAN_POINT('Ctrl Pts',(-7.72197650334821,-1.79930232279479,
74.7187080685195));
#60935=CARTESIAN_POINT('Ctrl Pts',(-7.81209422176409,-1.24734752017167,
74.6977405539795));
#60936=CARTESIAN_POINT('Ctrl Pts',(-7.81642405686987,-1.21992086371801,
74.6966960964807));
#60937=CARTESIAN_POINT('Ctrl Pts',(-7.83194396905852,-1.11813637000325,
74.6928088706968));
#60938=CARTESIAN_POINT('Ctrl Pts',(-7.842217939224,-1.04364395560218,74.6899420640016));
#60939=CARTESIAN_POINT('Ctrl Pts',(-7.86412117576441,-0.866173827354949,
74.6830403611618));
#60940=CARTESIAN_POINT('Ctrl Pts',(-7.87479181495238,-0.763093431508333,
74.6789743761494));
#60941=CARTESIAN_POINT('Ctrl Pts',(-7.88449381396879,-0.647178220215648,
74.6743125158825));
#60942=CARTESIAN_POINT('Ctrl Pts',(-7.88552279664459,-0.634517590096962,
74.6738021341312));
#60943=CARTESIAN_POINT('Ctrl Pts',(-7.8869724488813,-0.616132724246009,
74.6730591926453));
#60944=CARTESIAN_POINT('Ctrl Pts',(-7.88741739167083,-0.610410380493285,
74.6728276966247));
#60945=CARTESIAN_POINT('Ctrl Pts',(-7.8881902706487,-0.600328549014301,
74.672419385478));
#60946=CARTESIAN_POINT('Ctrl Pts',(-7.88852082168823,-0.595969259606479,
74.6722426863553));
#60947=CARTESIAN_POINT('Ctrl Pts',(-7.88914847521694,-0.587599783764911,
74.6719031488454));
#60948=CARTESIAN_POINT('Ctrl Pts',(-7.88944613408017,-0.583589639435366,
74.6717403354051));
#60949=CARTESIAN_POINT('Ctrl Pts',(-7.89007359526751,-0.575048088177602,
74.6713932702122));
#60950=CARTESIAN_POINT('Ctrl Pts',(-7.89040255158785,-0.570516622210531,
74.6712089803689));
#60951=CARTESIAN_POINT('Ctrl Pts',(-7.89117955925274,-0.559683902082172,
74.6707680268791));
#60952=CARTESIAN_POINT('Ctrl Pts',(-7.89162396655545,-0.553382396496017,
74.6705111974594));
#60953=CARTESIAN_POINT('Ctrl Pts',(-7.89278970467752,-0.53656571560085,
74.6698249290095));
#60954=CARTESIAN_POINT('Ctrl Pts',(-7.89349756814213,-0.52604964544283,
74.6693948694301));
#60955=CARTESIAN_POINT('Ctrl Pts',(-7.90537857213335,-0.34411953389681,
74.6619385649561));
#60956=CARTESIAN_POINT('Ctrl Pts',(-7.91098514682664,-0.172414955914368,
74.6546275518882));
#60957=CARTESIAN_POINT('Ctrl Pts',(-7.91099997052785,-0.000682867722154,
74.6471121226888));
#60958=CARTESIAN_POINT('',(-7.91099996455606,-0.000133956286235481,72.642331508237));
#60959=CARTESIAN_POINT('Ctrl Pts',(-7.91099994932565,-0.00089541584189321,
74.6422459153707));
#60960=CARTESIAN_POINT('Ctrl Pts',(-7.91102194644307,0.193449140794186,
74.6343900678167));
#60961=CARTESIAN_POINT('Ctrl Pts',(-7.90387815483653,0.388049300595132,
74.6265342202626));
#60962=CARTESIAN_POINT('Ctrl Pts',(-7.88953808641908,0.582331334330231,
74.6186783727085));
#60963=CARTESIAN_POINT('Ctrl Pts',(-7.87521209893698,0.776422596816661,
74.6108302390425));
#60964=CARTESIAN_POINT('Ctrl Pts',(-7.8537039329886,0.970196009224877,74.6029821053764));
#60965=CARTESIAN_POINT('Ctrl Pts',(-7.82503509210339,1.16307644088875,74.5951339717104));
#60966=CARTESIAN_POINT('Ctrl Pts',(-7.79638889121586,1.35580455343575,74.5872920357741));
#60967=CARTESIAN_POINT('Ctrl Pts',(-7.76059332992449,1.54764074561036,74.5794500998377));
#60968=CARTESIAN_POINT('Ctrl Pts',(-7.71772184260884,1.73801339468901,74.5716081639014));
#60969=CARTESIAN_POINT('Ctrl Pts',(-7.67487597314194,1.92827228662892,74.5637709139124));
#60970=CARTESIAN_POINT('Ctrl Pts',(-7.6249626772959,2.11706903739895,74.5559336639233));
#60971=CARTESIAN_POINT('Ctrl Pts',(-7.56810678752856,2.3038404138664,74.5480964139343));
#60972=CARTESIAN_POINT('Ctrl Pts',(-7.51127394917922,2.49053606651551,74.5402623414476));
#60973=CARTESIAN_POINT('Ctrl Pts',(-7.44750422697393,2.67520764683579,74.532428268961));
#60974=CARTESIAN_POINT('Ctrl Pts',(-7.37697285163034,2.8573051195679,74.5245941964743));
#60975=CARTESIAN_POINT('Ctrl Pts',(-7.30644453438772,3.03939469691365,74.5167604636575));
#60976=CARTESIAN_POINT('Ctrl Pts',(-7.22915526570112,3.21891005951464,74.5089267308408));
#60977=CARTESIAN_POINT('Ctrl Pts',(-7.1453293354841,3.39531879025673,74.501092998024));
#60978=CARTESIAN_POINT('Ctrl Pts',(-7.06150186723957,3.57173075772376,74.4932591214749));
#60979=CARTESIAN_POINT('Ctrl Pts',(-6.9711376478802,3.74503566313881,74.4854252449258));
#60980=CARTESIAN_POINT('Ctrl Pts',(-6.87450807130635,3.91472346118392,74.4775913683767));
#60981=CARTESIAN_POINT('Ctrl Pts',(-6.7778599042609,4.08444390530183,74.4697559846756));
#60982=CARTESIAN_POINT('Ctrl Pts',(-6.67494415161497,4.25054555136554,74.4619206009745));
#60983=CARTESIAN_POINT('Ctrl Pts',(-6.56607697610846,4.41254508688788,74.4540852172734));
#60984=CARTESIAN_POINT('Ctrl Pts',(-6.45716990750051,4.57460398524273,74.4462469623877));
#60985=CARTESIAN_POINT('Ctrl Pts',(-6.34230726650615,4.73255748814937,74.438408707502));
#60986=CARTESIAN_POINT('Ctrl Pts',(-6.22184723591979,4.88595312839545,74.4305704526164));
#60987=CARTESIAN_POINT('Ctrl Pts',(-6.10125341770897,5.03951913584309,74.422723492258));
#60988=CARTESIAN_POINT('Ctrl Pts',(-5.97505000736939,5.18851689268872,74.4148765318997));
#60989=CARTESIAN_POINT('Ctrl Pts',(-5.84363476146546,5.33252789721652,74.4070295715414));
#60990=CARTESIAN_POINT('Ctrl Pts',(-5.71214195379757,5.47662389757161,74.399177979878));
#60991=CARTESIAN_POINT('Ctrl Pts',(-5.57543142418788,5.61572703025123,74.3913263882147));
#60992=CARTESIAN_POINT('Ctrl Pts',(-5.43393623575889,5.74945719052734,74.3834747965513));
#60993=CARTESIAN_POINT('Ctrl Pts',(-5.29223343387657,5.88338357076468,74.3756116843827));
#60994=CARTESIAN_POINT('Ctrl Pts',(-5.14573220875179,6.01192099649521,74.3677485722141));
#60995=CARTESIAN_POINT('Ctrl Pts',(-4.99489806692352,6.13473017345047,74.3598854600455));
#60996=CARTESIAN_POINT('Ctrl Pts',(-4.8744750196751,6.23277863343284,74.3536077041163));
#60997=CARTESIAN_POINT('Ctrl Pts',(-4.75129077201187,6.32717663391295,74.347329948187));
#60998=CARTESIAN_POINT('Ctrl Pts',(-4.62559424657141,6.41777211079401,74.3410521922577));
#60999=CARTESIAN_POINT('Ctrl Pts',(-4.46854943026035,6.53096179503982,74.3332087851047));
#61000=CARTESIAN_POINT('Ctrl Pts',(-4.30710127573518,6.63856101387509,74.3253653779516));
#61001=CARTESIAN_POINT('Ctrl Pts',(-4.14168797058622,6.74020339116717,74.3175219707985));
#61002=CARTESIAN_POINT('Ctrl Pts',(-3.97646886206965,6.84172643944058,74.3096877718724));
#61003=CARTESIAN_POINT('Ctrl Pts',(-3.80729416822044,6.93730638928325,74.3018535729463));
#61004=CARTESIAN_POINT('Ctrl Pts',(-3.63463451777544,7.02661745950321,74.2940193740201));
#61005=CARTESIAN_POINT('Ctrl Pts',(-3.462143997643,7.11584104426155,74.286192849154));
#61006=CARTESIAN_POINT('Ctrl Pts',(-3.28617562885373,7.19880781798418,74.2783663242879));
#61007=CARTESIAN_POINT('Ctrl Pts',(-3.10722851531469,7.27523552564556,74.2705397994217));
#61008=CARTESIAN_POINT('Ctrl Pts',(-2.92842191524121,7.3516032204805,74.2627194201262));
#61009=CARTESIAN_POINT('Ctrl Pts',(-2.74664155057281,7.42144193847331,74.2548990408307));
#61010=CARTESIAN_POINT('Ctrl Pts',(-2.56241076835612,7.48451548560177,74.2470786615353));
#61011=CARTESIAN_POINT('Ctrl Pts',(-2.37828886025944,7.54755175841125,74.2392629038177));
#61012=CARTESIAN_POINT('Ctrl Pts',(-2.19171975084654,7.60383071078097,74.2314471461001));
#61013=CARTESIAN_POINT('Ctrl Pts',(-2.00324657220252,7.65316432405308,74.2236313883826));
#61014=CARTESIAN_POINT('Ctrl Pts',(-1.81484817241031,7.70247836365968,74.2158187316547));
#61015=CARTESIAN_POINT('Ctrl Pts',(-1.62454754815614,7.74485246558273,74.2080060749269));
#61016=CARTESIAN_POINT('Ctrl Pts',(-1.43290297449505,7.78014846038835,74.200193418199));
#61017=CARTESIAN_POINT('Ctrl Pts',(-1.24126560417739,7.81544312852363,74.1923810551254));
#61018=CARTESIAN_POINT('Ctrl Pts',(-1.04828472912884,7.84366014701759,74.1845686920519));
#61019=CARTESIAN_POINT('Ctrl Pts',(-0.854529267370442,7.86471237434703,
74.1767563289783));
#61020=CARTESIAN_POINT('Ctrl Pts',(-0.660768106299891,7.88576522092723,
74.1689437361043));
#61021=CARTESIAN_POINT('Ctrl Pts',(-0.466232662795107,7.89965281774444,
74.1611311432302));
#61022=CARTESIAN_POINT('Ctrl Pts',(-0.27149740643086,7.90633987116044,74.1533185503562));
#61023=CARTESIAN_POINT('Ctrl Pts',(-0.076722163289667,7.91302829769048,
74.1455043532507));
#61024=CARTESIAN_POINT('Ctrl Pts',(0.118252622912289,7.91251322335745,74.1376901561453));
#61025=CARTESIAN_POINT('Ctrl Pts',(0.312851893044608,7.90481149003684,74.1298759590399));
#61026=CARTESIAN_POINT('Ctrl Pts',(0.507525359154526,7.89710682023227,74.1220587825708));
#61027=CARTESIAN_POINT('Ctrl Pts',(0.70182267285472,7.88221004719473,74.1142416061017));
#61028=CARTESIAN_POINT('Ctrl Pts',(0.89517315124006,7.86018994867802,74.1064244296327));
#61029=CARTESIAN_POINT('Ctrl Pts',(1.08873337038756,7.83814596342317,74.0985987733265));
#61030=CARTESIAN_POINT('Ctrl Pts',(1.28134435330082,7.80896325924617,74.0907731170204));
#61031=CARTESIAN_POINT('Ctrl Pts',(1.47244382938962,7.77276206822854,74.0829474607143));
#61032=CARTESIAN_POINT('Ctrl Pts',(1.66365945679525,7.7365388739271,74.075117047931));
#61033=CARTESIAN_POINT('Ctrl Pts',(1.85336140466193,7.6932887691761,74.0672866351478));
#61034=CARTESIAN_POINT('Ctrl Pts',(2.04100176571583,7.6431821116826,74.0594562223645));
#61035=CARTESIAN_POINT('Ctrl Pts',(2.22889857301095,7.5930069739117,74.0516151078329));
#61036=CARTESIAN_POINT('Ctrl Pts',(2.41472783098999,7.53595666990954,74.0437739933013));
#61037=CARTESIAN_POINT('Ctrl Pts',(2.59795976063738,7.4722504027976,74.0359328787697));
#61038=CARTESIAN_POINT('Ctrl Pts',(2.69675872130326,7.43789987780628,74.0317049367966));
#61039=CARTESIAN_POINT('Ctrl Pts',(2.7948029183207,7.40161502359304,74.0274769948233));
#61040=CARTESIAN_POINT('Ctrl Pts',(2.89201224625962,7.3634357583593,74.0232490528502));
#61041=CARTESIAN_POINT('Ctrl Pts',(3.07390617094678,7.29199635493702,74.0153379091857));
#61042=CARTESIAN_POINT('Ctrl Pts',(3.25339594683619,7.21371711665667,74.0074267655212));
#61043=CARTESIAN_POINT('Ctrl Pts',(3.42993046795433,7.12877955789058,73.9995156218567));
#61044=CARTESIAN_POINT('Ctrl Pts',(3.60627360478942,7.04393408147578,73.9916130548069));
#61045=CARTESIAN_POINT('Ctrl Pts',(3.77966756050509,6.95244481072383,73.983710487757));
#61046=CARTESIAN_POINT('Ctrl Pts',(3.94957870478955,6.85454222064996,73.9758079207072));
#61047=CARTESIAN_POINT('Ctrl Pts',(4.1193371863076,6.75672759467228,73.9679124540024));
#61048=CARTESIAN_POINT('Ctrl Pts',(4.28561879324678,6.65251129941072,73.9600169872976));
#61049=CARTESIAN_POINT('Ctrl Pts',(4.44791186724698,6.54217097156621,73.9521215205928));
#61050=CARTESIAN_POINT('Ctrl Pts',(4.61008924068536,6.43190930658517,73.9442316826551));
#61051=CARTESIAN_POINT('Ctrl Pts',(4.76828346234788,6.315532500463,73.9363418447176));
#61052=CARTESIAN_POINT('Ctrl Pts',(4.92200915181058,6.19336313399214,73.9284520067799));
#61053=CARTESIAN_POINT('Ctrl Pts',(5.07565376969686,6.07125819698108,73.9205663297708));
#61054=CARTESIAN_POINT('Ctrl Pts',(5.2248342819248,5.94336700090116,73.9126806527617));
#61055=CARTESIAN_POINT('Ctrl Pts',(5.36909566265947,5.81005445458227,73.9047949757526));
#61056=CARTESIAN_POINT('Ctrl Pts',(5.51330772398102,5.67678748453967,73.8969119946622));
#61057=CARTESIAN_POINT('Ctrl Pts',(5.65260375261238,5.53810309195948,73.8890290135718));
#61058=CARTESIAN_POINT('Ctrl Pts',(5.78656288774104,5.39440552296711,73.8811460324815));
#61059=CARTESIAN_POINT('Ctrl Pts',(5.92052402967655,5.25070580127895,73.8732629332982));
#61060=CARTESIAN_POINT('Ctrl Pts',(6.04914787705711,5.10199299955927,73.8653798341149));
#61061=CARTESIAN_POINT('Ctrl Pts',(6.17205105019653,4.9487075922677,73.8574967349317));
#61062=CARTESIAN_POINT('Ctrl Pts',(6.29496182703056,4.79541270161295,73.8496131480419));
#61063=CARTESIAN_POINT('Ctrl Pts',(6.41215100808309,4.6375449105039,73.8417295611521));
#61064=CARTESIAN_POINT('Ctrl Pts',(6.52327606147301,4.4755771053366,73.8338459742624));
#61065=CARTESIAN_POINT('Ctrl Pts',(6.63442666983935,4.31357205309211,73.8259605744162));
#61066=CARTESIAN_POINT('Ctrl Pts',(6.73951017654278,4.1474653924283,73.81807517457));
#61067=CARTESIAN_POINT('Ctrl Pts',(6.83822774164264,3.97775845840707,73.8101897747239));
#61068=CARTESIAN_POINT('Ctrl Pts',(6.9369846029145,3.80798396971245,73.8023012359629));
#61069=CARTESIAN_POINT('Ctrl Pts',(7.02937029991796,3.63460664989781,73.7944126972019));
#61070=CARTESIAN_POINT('Ctrl Pts',(7.11513213477735,3.45815206499928,73.7865241584409));
#61071=CARTESIAN_POINT('Ctrl Pts',(7.2009852462306,3.28150967892427,73.7786272238829));
#61072=CARTESIAN_POINT('Ctrl Pts',(7.28020026341932,3.10178379628958,73.770730289325));
#61073=CARTESIAN_POINT('Ctrl Pts',(7.35257237048228,2.91952060051313,73.7628333547671));
#61074=CARTESIAN_POINT('Ctrl Pts',(7.42498861809563,2.73714624039307,73.7549316037813));
#61075=CARTESIAN_POINT('Ctrl Pts',(7.4905535200444,2.55223180610671,73.7470298527954));
#61076=CARTESIAN_POINT('Ctrl Pts',(7.54911218770278,2.36533849109959,73.7391281018096));
#61077=CARTESIAN_POINT('Ctrl Pts',(7.6077465975999,2.17820344043406,73.7312161303673));
#61078=CARTESIAN_POINT('Ctrl Pts',(7.65935658192268,1.98908472824269,73.7233041589251));
#61079=CARTESIAN_POINT('Ctrl Pts',(7.70383813669256,1.79855468742024,73.7153921874828));
#61080=CARTESIAN_POINT('Ctrl Pts',(7.72247764336563,1.71871516774285,73.7120767628027));
#61081=CARTESIAN_POINT('Ctrl Pts',(7.73986606790911,1.63862790595284,73.7087613381226));
#61082=CARTESIAN_POINT('Ctrl Pts',(7.75599846688739,1.5583352597052,73.7054459134424));
#61083=CARTESIAN_POINT('Ctrl Pts',(7.79449283298146,1.36674475146895,73.6975348041545));
#61084=CARTESIAN_POINT('Ctrl Pts',(7.82593565520974,1.17346951254426,73.6896236948665));
#61085=CARTESIAN_POINT('Ctrl Pts',(7.85018093930971,0.979071100634962,73.6817125855785));
#61086=CARTESIAN_POINT('Ctrl Pts',(7.87439993954777,0.784883432431188,73.6738100525771));
#61087=CARTESIAN_POINT('Ctrl Pts',(7.89143690121566,0.589575355637895,73.6659075195756));
#61088=CARTESIAN_POINT('Ctrl Pts',(7.90119645078819,0.393720263705267,73.6580049865742));
#61089=CARTESIAN_POINT('Ctrl Pts',(7.91094723194043,0.198041136836178,73.6501095535655));
#61090=CARTESIAN_POINT('Ctrl Pts',(7.9134336089223,0.00181631610688981,
73.6422141205568));
#61091=CARTESIAN_POINT('Ctrl Pts',(7.90861175274931,-0.194373723212607,
73.634318687548));
#61092=CARTESIAN_POINT('Ctrl Pts',(7.9037933339166,-0.390423905203012,73.6264288829299));
#61093=CARTESIAN_POINT('Ctrl Pts',(7.8916770700637,-0.586439011857354,73.6185390783117));
#61094=CARTESIAN_POINT('Ctrl Pts',(7.87227114556442,-0.781836306853166,
73.6106492736936));
#61095=CARTESIAN_POINT('Ctrl Pts',(7.85287545438328,-0.977130563074305,
73.6027636296029));
#61096=CARTESIAN_POINT('Ctrl Pts',(7.82619779635584,-1.17180731448945,73.5948779855122));
#61097=CARTESIAN_POINT('Ctrl Pts',(7.79229837886304,-1.36528640759678,73.5869923414214));
#61098=CARTESIAN_POINT('Ctrl Pts',(7.75841054896432,-1.55869936513715,73.5791093928237));
#61099=CARTESIAN_POINT('Ctrl Pts',(7.71730593897962,-1.75091514104126,73.571226444226));
#61100=CARTESIAN_POINT('Ctrl Pts',(7.66909632977393,-1.94136098772175,73.5633434956283));
#61101=CARTESIAN_POINT('Ctrl Pts',(7.62088599392436,-2.13180970491528,73.555460428214));
#61102=CARTESIAN_POINT('Ctrl Pts',(7.56557052129184,-2.3204881032442,73.5475773607998));
#61103=CARTESIAN_POINT('Ctrl Pts',(7.50331244954073,-2.50683531261373,73.5396942933856));
#61104=CARTESIAN_POINT('Ctrl Pts',(7.44105052245668,-2.69319406153968,73.5318107378122));
#61105=CARTESIAN_POINT('Ctrl Pts',(7.37184524835379,-2.87722100640294,73.5239271822388));
#61106=CARTESIAN_POINT('Ctrl Pts',(7.29590853774536,-3.05837205206535,73.5160436266654));
#61107=CARTESIAN_POINT('Ctrl Pts',(7.21995435962968,-3.2395647673916,73.50815825766));
#61108=CARTESIAN_POINT('Ctrl Pts',(7.13726579291068,-3.41787994716892,73.5002728886546));
#61109=CARTESIAN_POINT('Ctrl Pts',(7.04810233046337,-3.59279480896374,73.4923875196491));
#61110=CARTESIAN_POINT('Ctrl Pts',(6.9589033692351,-3.76777930987076,73.4844990112301));
#61111=CARTESIAN_POINT('Ctrl Pts',(6.86322453218225,-3.9393604882114,73.476610502811));
#61112=CARTESIAN_POINT('Ctrl Pts',(6.76137067674087,-4.10704121865226,73.468721994392));
#61113=CARTESIAN_POINT('Ctrl Pts',(6.6594084060418,-4.27490043177816,73.4608250892886));
#61114=CARTESIAN_POINT('Ctrl Pts',(6.55125816750903,-4.43885060946561,73.4529281841853));
#61115=CARTESIAN_POINT('Ctrl Pts',(6.43726808841204,-4.59842370360888,73.4450312790819));
#61116=CARTESIAN_POINT('Ctrl Pts',(6.32320847851897,-4.7580941329269,73.4371295570848));
#61117=CARTESIAN_POINT('Ctrl Pts',(6.20330213666765,-4.91338188362191,73.4292278350876));
#61118=CARTESIAN_POINT('Ctrl Pts',(6.0779368546735,-5.06385274179667,73.4213261130905));
#61119=CARTESIAN_POINT('Ctrl Pts',(5.9524094045112,-5.21451824383967,73.4134141697007));
#61120=CARTESIAN_POINT('Ctrl Pts',(5.82140913931665,-5.36035415185085,73.4055022263108));
#61121=CARTESIAN_POINT('Ctrl Pts',(5.68536078078645,-5.50096298772272,73.397590282921));
#61122=CARTESIAN_POINT('Ctrl Pts',(5.62834393133281,-5.55989109911908,73.3942744466256));
#61123=CARTESIAN_POINT('Ctrl Pts',(5.57044084668786,-5.61790161832553,73.3909586103302));
#61124=CARTESIAN_POINT('Ctrl Pts',(5.51168446450331,-5.67496743283633,73.3876427740348));
#61125=CARTESIAN_POINT('Ctrl Pts',(5.37275346019076,-5.80990104561383,73.3798023922834));
#61126=CARTESIAN_POINT('Ctrl Pts',(5.22865548944522,-5.93993266925251,73.371962010532));
#61127=CARTESIAN_POINT('Ctrl Pts',(5.07977286725619,-6.06463755034774,73.3641216287806));
#61128=CARTESIAN_POINT('Ctrl Pts',(4.93105669264826,-6.18920301405829,73.3562900124081));
#61129=CARTESIAN_POINT('Ctrl Pts',(4.77756678462485,-6.30845336992658,73.3484583960355));
#61130=CARTESIAN_POINT('Ctrl Pts',(4.61972327526206,-6.42199952195592,73.3406267796629));
#61131=CARTESIAN_POINT('Ctrl Pts',(4.46202554069436,-6.53544080957168,73.3328023961013));
#61132=CARTESIAN_POINT('Ctrl Pts',(4.2999824952884,-6.64318818069257,73.3249780125397));
#61133=CARTESIAN_POINT('Ctrl Pts',(4.13404857025015,-6.74489165360072,73.3171536289781));
#61134=CARTESIAN_POINT('Ctrl Pts',(3.9682356448381,-6.84652096396374,73.3093349509857));
#61135=CARTESIAN_POINT('Ctrl Pts',(3.79853778921688,-6.94211497125855,73.3015162729933));
#61136=CARTESIAN_POINT('Ctrl Pts',(3.62543989696728,-7.03136590951416,73.2936975950009));
#61137=CARTESIAN_POINT('Ctrl Pts',(3.45243460117617,-7.12056910414509,73.2858830995082));
#61138=CARTESIAN_POINT('Ctrl Pts',(3.27603320358031,-7.20343582829939,73.2780686040155));
#61139=CARTESIAN_POINT('Ctrl Pts',(3.096746940803,-7.27970324839051,73.2702541085229));
#61140=CARTESIAN_POINT('Ctrl Pts',(2.91752176390836,-7.35594468287289,73.2624422755619));
#61141=CARTESIAN_POINT('Ctrl Pts',(2.73541400341827,-7.4255911558716,73.2546304426009));
#61142=CARTESIAN_POINT('Ctrl Pts',(2.55095687597675,-7.4884270722834,73.2468186096399));
#61143=CARTESIAN_POINT('Ctrl Pts',(2.36649110968891,-7.55126593154611,73.2390064108204));
#61144=CARTESIAN_POINT('Ctrl Pts',(2.17967608651558,-7.60729347493693,73.2311942120008));
#61145=CARTESIAN_POINT('Ctrl Pts',(1.99106275853056,-7.65634312786416,73.2233820131813));
#61146=CARTESIAN_POINT('Ctrl Pts',(1.80243400734703,-7.70539679165605,73.2155691755463));
#61147=CARTESIAN_POINT('Ctrl Pts',(1.61200699876838,-7.74747133899127,73.2077563379113));
#61148=CARTESIAN_POINT('Ctrl Pts',(1.42034544108779,-7.78245075975307,73.1999435002764));
#61149=CARTESIAN_POINT('Ctrl Pts',(1.22863448724491,-7.81743919562028,73.1921286490702));
#61150=CARTESIAN_POINT('Ctrl Pts',(1.03568869647809,-7.84532879890732,73.1843137978641));
#61151=CARTESIAN_POINT('Ctrl Pts',(0.842079659009908,-7.86605510074025,
73.1764989466579));
#61152=CARTESIAN_POINT('Ctrl Pts',(0.648386654184466,-7.88679039147584,
73.1686807061864));
#61153=CARTESIAN_POINT('Ctrl Pts',(0.454030179016691,-7.90035615466375,
73.160862465715));
#61154=CARTESIAN_POINT('Ctrl Pts',(0.259584759797906,-7.90673995730735,
73.1530442252434));
#61155=CARTESIAN_POINT('Ctrl Pts',(0.0649130088055798,-7.91313119060877,
73.1452168844484));
#61156=CARTESIAN_POINT('Ctrl Pts',(-0.129847541460096,-7.91232375521652,
73.1373895436533));
#61157=CARTESIAN_POINT('Ctrl Pts',(-0.32412344744981,-7.90435734204959,
73.1295622028582));
#61158=CARTESIAN_POINT('Ctrl Pts',(-0.518526178365934,-7.89638572834192,
73.12172975231));
#61159=CARTESIAN_POINT('Ctrl Pts',(-0.712443285170314,-7.8812458507839,
73.1138973017618));
#61160=CARTESIAN_POINT('Ctrl Pts',(-0.905308544782102,-7.85902903918445,
73.1060648512135));
#61161=CARTESIAN_POINT('Ctrl Pts',(-1.09845058537667,-7.83678034423307,
73.0982211603136));
#61162=CARTESIAN_POINT('Ctrl Pts',(-1.29053741764301,-7.80743448352382,
73.0903774694136));
#61163=CARTESIAN_POINT('Ctrl Pts',(-1.48101390737776,-7.77113368860385,
73.0825337785136));
#61164=CARTESIAN_POINT('Ctrl Pts',(-1.58376893255215,-7.75155075161753,
73.0783023972181));
#61165=CARTESIAN_POINT('Ctrl Pts',(-1.68605557863687,-7.72994464739893,
73.0740710159226));
#61166=CARTESIAN_POINT('Ctrl Pts',(-1.78778884638401,-7.7063436233239,73.0698396346272));
#61167=CARTESIAN_POINT('Ctrl Pts',(-1.97815190839978,-7.66218144010575,
73.061921883455));
#61168=CARTESIAN_POINT('Ctrl Pts',(-2.1671452454434,-7.61089943386916,73.0540041322827));
#61169=CARTESIAN_POINT('Ctrl Pts',(-2.35419659870376,-7.55259421488085,
73.0460863811105));
#61170=CARTESIAN_POINT('Ctrl Pts',(-2.54103304357766,-7.4943559843442,73.0381777268579));
#61171=CARTESIAN_POINT('Ctrl Pts',(-2.72593162325107,-7.42911071492126,
73.0302690726053));
#61172=CARTESIAN_POINT('Ctrl Pts',(-2.90832993989894,-7.35700604598687,
73.0223604183527));
#61173=CARTESIAN_POINT('Ctrl Pts',(-3.09055245868333,-7.28497087246768,
73.0144593865637));
#61174=CARTESIAN_POINT('Ctrl Pts',(-3.27027919682617,-7.20608959507233,
73.0065583547746));
#61175=CARTESIAN_POINT('Ctrl Pts',(-3.44696232993268,-7.12055978810831,
72.9986573229856));
#61176=CARTESIAN_POINT('Ctrl Pts',(-3.62350786865408,-7.03509658864096,
72.9907624442322));
#61177=CARTESIAN_POINT('Ctrl Pts',(-3.79701421605697,-6.94299532447365,
72.9828675654788));
#61178=CARTESIAN_POINT('Ctrl Pts',(-3.96695270934947,-6.84450196886413,
72.9749726867254));
#61179=CARTESIAN_POINT('Ctrl Pts',(-4.13679029977623,-6.7460670947772,72.9670824956438));
#61180=CARTESIAN_POINT('Ctrl Pts',(-4.30306396017696,-6.64124786415838,
72.9591923045622));
#61181=CARTESIAN_POINT('Ctrl Pts',(-4.46526861175117,-6.53033668541751,
72.9513021134806));
#61182=CARTESIAN_POINT('Ctrl Pts',(-4.62740695520858,-6.41947084638376,
72.9434151478535));
#61183=CARTESIAN_POINT('Ctrl Pts',(-4.78547932102437,-6.30251821654022,
72.9355281822263));
#61184=CARTESIAN_POINT('Ctrl Pts',(-4.93900843104948,-6.17981526568733,
72.9276412165992));
#61185=CARTESIAN_POINT('Ctrl Pts',(-5.09252420868523,-6.05712297029592,
72.9197549358721));
#61186=CARTESIAN_POINT('Ctrl Pts',(-5.24149724359643,-5.92868155869958,
72.911868655145));
#61187=CARTESIAN_POINT('Ctrl Pts',(-5.38548185032401,-5.79486895795157,
72.9039823744179));
#61188=CARTESIAN_POINT('Ctrl Pts',(-5.52946620431588,-5.66105659208437,
72.8960961075336));
#61189=CARTESIAN_POINT('Ctrl Pts',(-5.66846189478627,-5.52187329002544,
72.8882098406493));
#61190=CARTESIAN_POINT('Ctrl Pts',(-5.80205867807116,-5.37773521998054,
72.8803235737649));
#61191=CARTESIAN_POINT('Ctrl Pts',(-5.93567761840211,-5.23357324461563,
72.8724359989421));
#61192=CARTESIAN_POINT('Ctrl Pts',(-6.06389563317599,-5.08445511660056,
72.8645484241192));
#61193=CARTESIAN_POINT('Ctrl Pts',(-6.18634133258751,-4.93083176722949,
72.8566608492964));
#61194=CARTESIAN_POINT('Ctrl Pts',(-6.30882786228494,-4.77715719118971,
72.8487706443123));
#61195=CARTESIAN_POINT('Ctrl Pts',(-6.42553802684242,-4.61897466976535,
72.8408804393282));
#61196=CARTESIAN_POINT('Ctrl Pts',(-6.53614235278993,-4.45676610829711,
72.8329902343441));
#61197=CARTESIAN_POINT('Ctrl Pts',(-6.64685348565564,-4.29440090741709,
72.8250924100515));
#61198=CARTESIAN_POINT('Ctrl Pts',(-6.75144680858466,-4.12800218571056,
72.8171945857589));
#61199=CARTESIAN_POINT('Ctrl Pts',(-6.84963706251331,-3.95807947265389,
72.8092967614663));
#61200=CARTESIAN_POINT('Ctrl Pts',(-6.9478816865164,-3.78806266970347,72.8013945639771));
#61201=CARTESIAN_POINT('Ctrl Pts',(-7.03971601159217,-3.61451828871069,
72.7934923664878));
#61202=CARTESIAN_POINT('Ctrl Pts',(-7.1249018280747,-3.43797832167363,72.7855901689985));
#61203=CARTESIAN_POINT('Ctrl Pts',(-7.21019047081311,-3.26122525644048,
72.7776784329098));
#61204=CARTESIAN_POINT('Ctrl Pts',(-7.28881443710697,-3.08146969736468,
72.7697666968211));
#61205=CARTESIAN_POINT('Ctrl Pts',(-7.36058412422407,-2.8992623803686,72.7618549607323));
#61206=CARTESIAN_POINT('Ctrl Pts',(-7.39027285456639,-2.82388927902195,
72.7585821388947));
#61207=CARTESIAN_POINT('Ctrl Pts',(-7.41878927289718,-2.74809680284435,
72.755309317057));
#61208=CARTESIAN_POINT('Ctrl Pts',(-7.44612248664829,-2.6719245711342,72.7520364952194));
#61209=CARTESIAN_POINT('Ctrl Pts',(-7.52247326301973,-2.45915013919315,
72.7428944129709));
#61210=CARTESIAN_POINT('Ctrl Pts',(-7.58973959628872,-2.24298999729443,
72.7337523307223));
#61211=CARTESIAN_POINT('Ctrl Pts',(-7.64765336366459,-2.02418354632915,
72.7246102484738));
#61212=CARTESIAN_POINT('Ctrl Pts',(-7.70439061686576,-1.80982213326664,
72.7156538869932));
#61213=CARTESIAN_POINT('Ctrl Pts',(-7.75215150291776,-1.59292105319892,
72.7066975255126));
#61214=CARTESIAN_POINT('Ctrl Pts',(-7.79073219648633,-1.37419534369438,
72.697741164032));
#61215=CARTESIAN_POINT('Ctrl Pts',(-7.83051291464963,-1.14866632904863,
72.6885062213995));
#61216=CARTESIAN_POINT('Ctrl Pts',(-7.8605330812214,-0.921197480203638,
72.679271278767));
#61217=CARTESIAN_POINT('Ctrl Pts',(-7.88062417100901,-0.692591997722056,
72.6700363361345));
#61218=CARTESIAN_POINT('Ctrl Pts',(-7.90071526079662,-0.463986515240399,
72.660801393502));
#61219=CARTESIAN_POINT('Ctrl Pts',(-7.91087714858086,-0.234244582106221,
72.6515664508695));
#61220=CARTESIAN_POINT('Ctrl Pts',(-7.9109988923078,-0.00418639519816283,
72.642331508237));
#61221=CARTESIAN_POINT('',(-7.90354147324386,0.00220337357936208,70.6423315082369));
#61222=CARTESIAN_POINT('Ctrl Pts',(-7.911,1.85740312019789E-12,72.642331508237));
#61223=CARTESIAN_POINT('Ctrl Pts',(-7.91099999999948,2.20167589666843,72.5537440725042));
#61224=CARTESIAN_POINT('Ctrl Pts',(-6.94214576672286,4.38610418338808,72.4651566367715));
#61225=CARTESIAN_POINT('Ctrl Pts',(-3.67820201488183,7.34180684107678,72.2879817653061));
#61226=CARTESIAN_POINT('Ctrl Pts',(-1.40868175871654,8.08992666571347,72.1993943295734));
#61227=CARTESIAN_POINT('Ctrl Pts',(2.97309270521321,7.65454228025233,72.0222194581079));
#61228=CARTESIAN_POINT('Ctrl Pts',(5.05102072675622,6.47444880834203,71.9336320223752));
#61229=CARTESIAN_POINT('Ctrl Pts',(7.66951518847864,2.93425195367713,71.7564571509098));
#61230=CARTESIAN_POINT('Ctrl Pts',(8.18956872247064,0.601881960099487,71.6678697151771));
#61231=CARTESIAN_POINT('Ctrl Pts',(7.3230668976137,-3.71537198232385,71.4906948437116));
#61232=CARTESIAN_POINT('Ctrl Pts',(5.94329958850262,-5.66643518936439,71.4021074079789));
#61233=CARTESIAN_POINT('Ctrl Pts',(2.16154501637973,-7.92205913232958,71.2249325365135));
#61234=CARTESIAN_POINT('Ctrl Pts',(-0.210816529298817,-8.20894963713001,
71.1363451007807));
#61235=CARTESIAN_POINT('Ctrl Pts',(-4.42123908576272,-6.91982244717931,
70.9591702293153));
#61236=CARTESIAN_POINT('Ctrl Pts',(-6.22631625634043,-5.35390358803681,
70.8705827935826));
#61237=CARTESIAN_POINT('Ctrl Pts',(-7.65317280859478,-2.31334857514619,
70.7354407413122));
#61238=CARTESIAN_POINT('Ctrl Pts',(-7.91100000000025,-1.15702837836482,
70.6888861247746));
#61239=CARTESIAN_POINT('Ctrl Pts',(-7.911,1.68642877440561E-12,70.642331508237));
#61240=CARTESIAN_POINT('',(-7.92318561732542,0.00259301387528471,68.6424391999658));
#61241=CARTESIAN_POINT('Ctrl Pts',(-7.89823755503975,0.00377023974625967,
70.6423315082369));
#61242=CARTESIAN_POINT('Ctrl Pts',(-7.90350964776257,0.958128817974856,
70.6040258452798));
#61243=CARTESIAN_POINT('Ctrl Pts',(-7.52228863784238,3.22866395001779,70.5127529924218));
#61244=CARTESIAN_POINT('Ctrl Pts',(-5.36383164184186,6.23324328561409,70.3685129496619));
#61245=CARTESIAN_POINT('Ctrl Pts',(-0.5271358810351,8.71026298249118,70.1566441900566));
#61246=CARTESIAN_POINT('Ctrl Pts',(6.62174075612686,6.61018822700539,69.8918082405504));
#61247=CARTESIAN_POINT('Ctrl Pts',(9.14004810553684,-1.99688238525928,69.5740051011428));
#61248=CARTESIAN_POINT('Ctrl Pts',(3.27357265470031,-8.75711389441476,69.256201961735));
#61249=CARTESIAN_POINT('Ctrl Pts',(-5.3858310801681,-7.53156686276361,68.945679994676));
#61250=CARTESIAN_POINT('Ctrl Pts',(-7.91004429377716,-2.43849120782205,
68.7410924074197));
#61251=CARTESIAN_POINT('Ctrl Pts',(-7.92318561732542,0.00259301387528471,
68.6424391999658));
#61252=CARTESIAN_POINT('',(-7.91099653591344,4.8067954642318E-5,64.635061427433));
#61253=CARTESIAN_POINT('Ctrl Pts',(-7.91099947655417,0.00287783939459638,
68.6494532539836));
#61254=CARTESIAN_POINT('Ctrl Pts',(-7.91094092592253,0.163829842891923,
68.6434681772393));
#61255=CARTESIAN_POINT('Ctrl Pts',(-7.90597044551911,0.324735313140411,
68.6372897700822));
#61256=CARTESIAN_POINT('Ctrl Pts',(-7.89567872179959,0.492163448253284,
68.6305561724352));
#61257=CARTESIAN_POINT('Ctrl Pts',(-7.89525230816442,0.498957240198783,
68.6302824165131));
#61258=CARTESIAN_POINT('Ctrl Pts',(-7.89454362150085,0.510019912661784,
68.6298357800155));
#61259=CARTESIAN_POINT('Ctrl Pts',(-7.89426665256145,0.514289141639768,
68.6296632071228));
#61260=CARTESIAN_POINT('Ctrl Pts',(-7.8937735402111,0.521795767861521,68.629359397902));
#61261=CARTESIAN_POINT('Ctrl Pts',(-7.89355886777265,0.525033264128524,
68.6292282476011));
#61262=CARTESIAN_POINT('Ctrl Pts',(-7.89313532577422,0.531361766581175,
68.6289716414006));
#61263=CARTESIAN_POINT('Ctrl Pts',(-7.89292663206871,0.534452784346573,
68.6288461958661));
#61264=CARTESIAN_POINT('Ctrl Pts',(-7.89250850430255,0.540592125052581,
68.6285968138893));
#61265=CARTESIAN_POINT('Ctrl Pts',(-7.89229912056636,0.543640439625881,
68.6284728806887));
#61266=CARTESIAN_POINT('Ctrl Pts',(-7.89180048221448,0.550838865707491,
68.6281799603841));
#61267=CARTESIAN_POINT('Ctrl Pts',(-7.89150972073084,0.554988859827049,
68.6280108846847));
#61268=CARTESIAN_POINT('Ctrl Pts',(-7.89048718821528,0.569420030229027,
68.6274222403401));
#61269=CARTESIAN_POINT('Ctrl Pts',(-7.88973860067586,0.57969996486082,68.6270016860655));
#61270=CARTESIAN_POINT('Ctrl Pts',(-7.8808503797559,0.698549930152759,68.6221254326864));
#61271=CARTESIAN_POINT('Ctrl Pts',(-7.87049072626236,0.806937635924736,
68.617542643153));
#61272=CARTESIAN_POINT('Ctrl Pts',(-7.85348961277053,0.952929441680667,
68.6112187738668));
#61273=CARTESIAN_POINT('Ctrl Pts',(-7.8488075570822,0.99075399211787,68.6095665836419));
#61274=CARTESIAN_POINT('Ctrl Pts',(-7.84124407009167,1.0484345092539,68.6070275917584));
#61275=CARTESIAN_POINT('Ctrl Pts',(-7.83856007311695,1.06831617814717,68.6061488957539));
#61276=CARTESIAN_POINT('Ctrl Pts',(-7.74238415395425,1.76085809806045,68.5754226798741));
#61277=CARTESIAN_POINT('Ctrl Pts',(-7.56274349562382,2.4187002454741,68.5426153192326));
#61278=CARTESIAN_POINT('Ctrl Pts',(-7.1907306448635,3.31055477745236,68.4986216735679));
#61279=CARTESIAN_POINT('Ctrl Pts',(-7.06582890206217,3.56937856281599,68.4858752252229));
#61280=CARTESIAN_POINT('Ctrl Pts',(-6.86690645513325,3.93002029751216,68.4682765040594));
#61281=CARTESIAN_POINT('Ctrl Pts',(-6.80411917675493,4.03775035884632,68.4630395629916));
#61282=CARTESIAN_POINT('Ctrl Pts',(-6.69853392034159,4.20945081593222,68.4547244392056));
#61283=CARTESIAN_POINT('Ctrl Pts',(-6.65730457636518,4.27435715415497,68.4515885722328));
#61284=CARTESIAN_POINT('Ctrl Pts',(-6.607713072547,4.34996920439848,68.4479429023018));
#61285=CARTESIAN_POINT('Ctrl Pts',(-6.60026236071995,4.3612659745087,68.447398419022));
#61286=CARTESIAN_POINT('Ctrl Pts',(-6.58881091488455,4.37853210160864,68.4465665106012));
#61287=CARTESIAN_POINT('Ctrl Pts',(-6.58483099114974,4.38451519044823,68.4462782891154));
#61288=CARTESIAN_POINT('Ctrl Pts',(-6.57788085544039,4.39493264306798,68.4457765422278));
#61289=CARTESIAN_POINT('Ctrl Pts',(-6.57491430095284,4.39936943444712,68.4455628767698));
#61290=CARTESIAN_POINT('Ctrl Pts',(-6.5687073268532,4.40863231007383,68.445116856689));
#61291=CARTESIAN_POINT('Ctrl Pts',(-6.56546607255558,4.41345783276506,68.4448845343044));
#61292=CARTESIAN_POINT('Ctrl Pts',(-6.55650168684509,4.42677212465107,68.4442436136742));
#61293=CARTESIAN_POINT('Ctrl Pts',(-6.55076738198565,4.43525337735473,68.443835445305));
#61294=CARTESIAN_POINT('Ctrl Pts',(-6.52830970369499,4.46833056536898,68.4422439493382));
#61295=CARTESIAN_POINT('Ctrl Pts',(-6.51146403846622,4.49284339028041,68.441065337577));
#61296=CARTESIAN_POINT('Ctrl Pts',(-6.24337421164096,4.87827699777393,68.4225441216345));
#61297=CARTESIAN_POINT('Ctrl Pts',(-5.96259051514637,5.21774623364937,68.4064461721521));
#61298=CARTESIAN_POINT('Ctrl Pts',(-5.27195462574641,5.92372307891987,68.3717041088256));
#61299=CARTESIAN_POINT('Ctrl Pts',(-4.84927165961036,6.27443315496323,68.3535185018485));
#61300=CARTESIAN_POINT('Ctrl Pts',(-4.31040847135696,6.63433116497635,68.3301794111759));
#61301=CARTESIAN_POINT('Ctrl Pts',(-4.22599274790826,6.68841951200458,68.3265158864006));
#61302=CARTESIAN_POINT('Ctrl Pts',(-4.01605792533861,6.81737146994626,68.3173340019242));
#61303=CARTESIAN_POINT('Ctrl Pts',(-3.88944820503646,6.89038953698008,68.3117333619421));
#61304=CARTESIAN_POINT('Ctrl Pts',(-3.7386136246717,6.97189573185971,68.3049167503924));
#61305=CARTESIAN_POINT('Ctrl Pts',(-3.71628338822199,6.98382414483279,68.3039043536631));
#61306=CARTESIAN_POINT('Ctrl Pts',(-3.68715147319466,6.99920661171946,68.302579742826));
#61307=CARTESIAN_POINT('Ctrl Pts',(-3.68040133394519,7.00275839939544,68.3022725505751));
#61308=CARTESIAN_POINT('Ctrl Pts',(-3.67005198614956,7.00818492106894,68.3018011637879));
#61309=CARTESIAN_POINT('Ctrl Pts',(-3.66645644142063,7.01006666387812,68.3016373222652));
#61310=CARTESIAN_POINT('Ctrl Pts',(-3.65937162888443,7.01376758712125,68.3013143395282));
#61311=CARTESIAN_POINT('Ctrl Pts',(-3.65588244830939,7.01558693257347,68.3011552066138));
#61312=CARTESIAN_POINT('Ctrl Pts',(-3.64798373953,7.01969802286378,68.300794814471));
#61313=CARTESIAN_POINT('Ctrl Pts',(-3.6435734089288,7.02198821628573,68.3005934788109));
#61314=CARTESIAN_POINT('Ctrl Pts',(-3.63145270505106,7.02826775356491,68.3000398699717));
#61315=CARTESIAN_POINT('Ctrl Pts',(-3.62373793315425,7.03224855617166,68.2996871812363));
#61316=CARTESIAN_POINT('Ctrl Pts',(-3.58613112125047,7.05157525755354,68.2979664460232));
#61317=CARTESIAN_POINT('Ctrl Pts',(-3.5561483611739,7.066743154887,68.2965899441491));
#61318=CARTESIAN_POINT('Ctrl Pts',(-3.392672769792,7.14813954724615,68.2890631914091));
#61319=CARTESIAN_POINT('Ctrl Pts',(-3.257429899254,7.21077490044745,68.2827587768466));
#61320=CARTESIAN_POINT('Ctrl Pts',(-3.08340777210517,7.28547508743618,68.2746137800077));
#61321=CARTESIAN_POINT('Ctrl Pts',(-3.04619000394575,7.30111478814185,68.272869916936));
#61322=CARTESIAN_POINT('Ctrl Pts',(-2.8310518646966,7.38958907319875,68.2627838571465));
#61323=CARTESIAN_POINT('Ctrl Pts',(-2.65064613646246,7.45620235622921,68.2543057865524));
#61324=CARTESIAN_POINT('Ctrl Pts',(-1.77928398254101,7.742321154766,68.2136785728615));
#61325=CARTESIAN_POINT('Ctrl Pts',(-1.06265114629847,7.87276354414527,68.1816371486636));
#61326=CARTESIAN_POINT('Ctrl Pts',(-0.270300186127443,7.90667344668757,
68.14923013952));
#61327=CARTESIAN_POINT('Ctrl Pts',(-0.20231096037545,7.90870518227394,68.1464694220199));
#61328=CARTESIAN_POINT('Ctrl Pts',(-0.116476910722555,7.91016257725009,
68.1430077333634));
#61329=CARTESIAN_POINT('Ctrl Pts',(-0.0986495706354486,7.91040499184555,
68.1422900397425));
#61330=CARTESIAN_POINT('Ctrl Pts',(-0.0702371149717731,7.91069527847364,
68.1411482101363));
#61331=CARTESIAN_POINT('Ctrl Pts',(-0.0596524929844704,7.91078217510751,
68.1407232813959));
#61332=CARTESIAN_POINT('Ctrl Pts',(-0.0397079781150411,7.91090588266893,
68.1399234132388));
#61333=CARTESIAN_POINT('Ctrl Pts',(-0.0303481306473132,7.91094732629901,
68.1395483800319));
#61334=CARTESIAN_POINT('Ctrl Pts',(-0.00939958587563894,7.9110029038809,
68.1387097647156));
#61335=CARTESIAN_POINT('Ctrl Pts',(0.00218912402489875,7.91100818518859,
68.1382463629129));
#61336=CARTESIAN_POINT('Ctrl Pts',(0.0314747774394929,7.91095718111787,
68.1370766141461));
#61337=CARTESIAN_POINT('Ctrl Pts',(0.0491716247692127,7.91086697763484,
68.1363709599773));
#61338=CARTESIAN_POINT('Ctrl Pts',(0.14487613256771,7.9100580022514,68.1325612589977));
#61339=CARTESIAN_POINT('Ctrl Pts',(0.222871048765295,7.9082447787756,68.1294798470457));
#61340=CARTESIAN_POINT('Ctrl Pts',(1.01103895469475,7.87825184796659,68.098564582206));
#61341=CARTESIAN_POINT('Ctrl Pts',(1.71434228040871,7.75564970723329,68.0732099874292));
#61342=CARTESIAN_POINT('Ctrl Pts',(2.58816134928532,7.47848717820106,68.0399228065226));
#61343=CARTESIAN_POINT('Ctrl Pts',(2.78199194130245,7.40856709915989,68.0323879451451));
#61344=CARTESIAN_POINT('Ctrl Pts',(3.14351509859778,7.26196550146311,68.0177501349705));
#61345=CARTESIAN_POINT('Ctrl Pts',(3.31168733223126,7.18683179006791,68.0106899685778));
#61346=CARTESIAN_POINT('Ctrl Pts',(3.50203226266947,7.09369176927395,68.0022628779281));
#61347=CARTESIAN_POINT('Ctrl Pts',(3.52692294393694,7.08134926455154,68.0011521103001));
#61348=CARTESIAN_POINT('Ctrl Pts',(3.55879786564547,7.06533375018621,67.999717781326));
#61349=CARTESIAN_POINT('Ctrl Pts',(3.56584253903808,7.06178095356809,67.9994000319825));
#61350=CARTESIAN_POINT('Ctrl Pts',(3.57653255425188,7.05636964953916,67.9989167069012));
#61351=CARTESIAN_POINT('Ctrl Pts',(3.58018180196981,7.05451883598822,67.9987515099943));
#61352=CARTESIAN_POINT('Ctrl Pts',(3.5875888710558,7.05075491514986,67.9984157831869));
#61353=CARTESIAN_POINT('Ctrl Pts',(3.5913466016845,7.04884163304157,67.998245244622));
#61354=CARTESIAN_POINT('Ctrl Pts',(3.59955010369944,7.04465648397866,67.9978724605965));
#61355=CARTESIAN_POINT('Ctrl Pts',(3.60399525556892,7.04238341216738,67.9976701547008));
#61356=CARTESIAN_POINT('Ctrl Pts',(3.61625134649596,7.03610149732554,67.997111500546));
#61357=CARTESIAN_POINT('Ctrl Pts',(3.62405775201769,7.03208386545488,67.9967547062395));
#61358=CARTESIAN_POINT('Ctrl Pts',(3.66252085681063,7.0122074490791,67.9949919068444));
#61359=CARTESIAN_POINT('Ctrl Pts',(3.69307986320553,6.99616133308654,67.993576206816));
#61360=CARTESIAN_POINT('Ctrl Pts',(4.14022183771854,6.7576272763702,67.97262566497));
#61361=CARTESIAN_POINT('Ctrl Pts',(4.53611858641511,6.49849833620121,67.9510108263184));
#61362=CARTESIAN_POINT('Ctrl Pts',(4.92750917515386,6.18904613259168,67.9280224711265));
#61363=CARTESIAN_POINT('Ctrl Pts',(4.94843960648932,6.17232404868004,67.926787684642));
#61364=CARTESIAN_POINT('Ctrl Pts',(4.99136920263822,6.13766731506257,67.924244324779));
#61365=CARTESIAN_POINT('Ctrl Pts',(5.01335761670537,6.11971992777455,67.9229357473975));
#61366=CARTESIAN_POINT('Ctrl Pts',(5.05855151511288,6.08242471110209,67.9202345565047));
#61367=CARTESIAN_POINT('Ctrl Pts',(5.08174372550052,6.06306147979911,67.9188419850648));
#61368=CARTESIAN_POINT('Ctrl Pts',(5.12963562442472,6.02260858448557,67.9159536586792));
#61369=CARTESIAN_POINT('Ctrl Pts',(5.15431753289776,6.00149869424389,67.9144580219927));
#61370=CARTESIAN_POINT('Ctrl Pts',(5.20686400143601,5.95599360007591,67.9112594598269));
#61371=CARTESIAN_POINT('Ctrl Pts',(5.23468870592389,5.93155347768586,67.9095569259487));
#61372=CARTESIAN_POINT('Ctrl Pts',(5.29446382939873,5.87830116751628,67.9058814038093));
#61373=CARTESIAN_POINT('Ctrl Pts',(5.32635296647424,5.84942184848483,67.9039092549819));
#61374=CARTESIAN_POINT('Ctrl Pts',(5.45704000537359,5.72911468680025,67.8957832267198));
#61375=CARTESIAN_POINT('Ctrl Pts',(5.55373361440389,5.63543121791988,67.8896666623384));
#61376=CARTESIAN_POINT('Ctrl Pts',(5.86952825081222,5.31344151356259,67.8693987595086));
#61377=CARTESIAN_POINT('Ctrl Pts',(6.0773280810714,5.07445904661621,67.8555830484987));
#61378=CARTESIAN_POINT('Ctrl Pts',(6.34452287154075,4.72713235174881,67.8372646471534));
#61379=CARTESIAN_POINT('Ctrl Pts',(6.41653884601722,4.62890718712765,67.8322613868703));
#61380=CARTESIAN_POINT('Ctrl Pts',(6.49493251040166,4.51663615140824,67.8267363506803));
#61381=CARTESIAN_POINT('Ctrl Pts',(6.503568665259,4.50419194290465,67.8261265667568));
#61382=CARTESIAN_POINT('Ctrl Pts',(6.51643972383408,4.4855312841497,67.8252160611097));
#61383=CARTESIAN_POINT('Ctrl Pts',(6.52070156495297,4.47933350808965,67.8249142944688));
#61384=CARTESIAN_POINT('Ctrl Pts',(6.52799683755423,4.46869189338354,67.8243972545249));
#61385=CARTESIAN_POINT('Ctrl Pts',(6.53103458229434,4.46425102722952,67.8241818142289));
#61386=CARTESIAN_POINT('Ctrl Pts',(6.53726325389339,4.45512539421982,67.823739769952));
#61387=CARTESIAN_POINT('Ctrl Pts',(6.54045368154829,4.4504402893004,67.8235131853382));
#61388=CARTESIAN_POINT('Ctrl Pts',(6.54898239257343,4.43788700026679,67.8229070384149));
#61389=CARTESIAN_POINT('Ctrl Pts',(6.5543115385856,4.43001260284519,67.8225278292217));
#61390=CARTESIAN_POINT('Ctrl Pts',(6.57353409713771,4.40149855097581,67.8211583215554));
#61391=CARTESIAN_POINT('Ctrl Pts',(6.58734438804481,4.38080288857381,67.8201712276785));
#61392=CARTESIAN_POINT('Ctrl Pts',(6.62019746402077,4.33106368670392,67.8178152375516));
#61393=CARTESIAN_POINT('Ctrl Pts',(6.6391471491737,4.3019591225542,67.8164499059574));
#61394=CARTESIAN_POINT('Ctrl Pts',(7.07985123176592,3.61523998330174,67.7845411723833));
#61395=CARTESIAN_POINT('Ctrl Pts',(7.40205778277287,2.89893642478682,67.7584110984444));
#61396=CARTESIAN_POINT('Ctrl Pts',(7.66813724775287,1.95531463424542,67.7250073861231));
#61397=CARTESIAN_POINT('Ctrl Pts',(7.71492825677698,1.7616646867055,67.718167678931));
#61398=CARTESIAN_POINT('Ctrl Pts',(7.78818608759195,1.39902066469634,67.7050928322685));
#61399=CARTESIAN_POINT('Ctrl Pts',(7.81657720664827,1.23053536838248,67.6989130312334));
#61400=CARTESIAN_POINT('Ctrl Pts',(7.85564106579971,0.941974937944957,67.6879655591328));
#61401=CARTESIAN_POINT('Ctrl Pts',(7.86906490094676,0.822331064325059,67.6833208780761));
#61402=CARTESIAN_POINT('Ctrl Pts',(7.88090175287269,0.689547614685502,67.6780060991761));
#61403=CARTESIAN_POINT('Ctrl Pts',(7.88201878972633,0.676659549575808,67.6774885771304));
#61404=CARTESIAN_POINT('Ctrl Pts',(7.88366781144431,0.657075307923078,67.6766995653631));
#61405=CARTESIAN_POINT('Ctrl Pts',(7.88422289231788,0.650381046159154,67.6764294043016));
#61406=CARTESIAN_POINT('Ctrl Pts',(7.88511372540038,0.639468874199588,67.6759882564822));
#61407=CARTESIAN_POINT('Ctrl Pts',(7.88545462185806,0.635251375480635,67.6758175691101));
#61408=CARTESIAN_POINT('Ctrl Pts',(7.88610414603498,0.627134513656483,67.6754887085127));
#61409=CARTESIAN_POINT('Ctrl Pts',(7.88641326574405,0.623235190050995,67.6753305641751));
#61410=CARTESIAN_POINT('Ctrl Pts',(7.88696889193816,0.616159756937043,67.6750433133565));
#61411=CARTESIAN_POINT('Ctrl Pts',(7.88721637215501,0.612983725060461,67.6749142644107));
#61412=CARTESIAN_POINT('Ctrl Pts',(7.88771278116616,0.606562999094773,67.6746531609388));
#61413=CARTESIAN_POINT('Ctrl Pts',(7.88796162657585,0.603318297128218,67.6745211014534));
#61414=CARTESIAN_POINT('Ctrl Pts',(7.88865743512677,0.594171611950547,67.6741485191722));
#61415=CARTESIAN_POINT('Ctrl Pts',(7.88909977595405,0.588269290292336,67.6739077272334));
#61416=CARTESIAN_POINT('Ctrl Pts',(7.89089870740357,0.563898496850559,67.6729119990488));
#61417=CARTESIAN_POINT('Ctrl Pts',(7.89219706296108,0.545425919393756,67.6721537153381));
#61418=CARTESIAN_POINT('Ctrl Pts',(7.91204488063971,0.248115668916403,67.6598944346911));
#61419=CARTESIAN_POINT('Ctrl Pts',(7.91586998213839,-0.0314863387240819,
67.6475929125248));
#61420=CARTESIAN_POINT('Ctrl Pts',(7.88580753096586,-0.796397804043023,
67.6129341639281));
#61421=CARTESIAN_POINT('Ctrl Pts',(7.82199184228816,-1.27932658237856,67.5900057008226));
#61422=CARTESIAN_POINT('Ctrl Pts',(7.70473192668626,-1.79523577118004,67.5659425830425));
#61423=CARTESIAN_POINT('Ctrl Pts',(7.69487217659428,-1.83703777119662,67.5639953181844));
#61424=CARTESIAN_POINT('Ctrl Pts',(7.67308528544332,-1.92615257412625,67.5598506312191));
#61425=CARTESIAN_POINT('Ctrl Pts',(7.66105982218207,-1.97343964210881,67.5576553014596));
#61426=CARTESIAN_POINT('Ctrl Pts',(7.63404754080314,-2.07568885271387,67.552918584164));
#61427=CARTESIAN_POINT('Ctrl Pts',(7.61890289850263,-2.13060668341339,67.5503809778475));
#61428=CARTESIAN_POINT('Ctrl Pts',(7.58390209904289,-2.25237942939429,67.5447708382287));
#61429=CARTESIAN_POINT('Ctrl Pts',(7.56375231647056,-2.31914538870215,67.5417061621037));
#61430=CARTESIAN_POINT('Ctrl Pts',(7.46759581862002,-2.62316551521308,67.5278090480241));
#61431=CARTESIAN_POINT('Ctrl Pts',(7.38128796122879,-2.85702431425384,67.5172879759508));
#61432=CARTESIAN_POINT('Ctrl Pts',(7.26879472569624,-3.12251170775818,67.505551997522));
#61433=CARTESIAN_POINT('Ctrl Pts',(7.25324062684075,-3.15847377668298,67.5039666414827));
#61434=CARTESIAN_POINT('Ctrl Pts',(7.23303085979246,-3.20426336802984,67.501953435656));
#61435=CARTESIAN_POINT('Ctrl Pts',(7.22862136846004,-3.21419854133358,67.5015169467027));
#61436=CARTESIAN_POINT('Ctrl Pts',(7.22151536459081,-3.23012073358205,67.5008179416756));
#61437=CARTESIAN_POINT('Ctrl Pts',(7.21883185799487,-3.23611352100214,67.5005549679327));
#61438=CARTESIAN_POINT('Ctrl Pts',(7.21372808772702,-3.24747328522235,67.5000567031605));
#61439=CARTESIAN_POINT('Ctrl Pts',(7.21130928872717,-3.25284091286537,67.4998213607178));
#61440=CARTESIAN_POINT('Ctrl Pts',(7.20581143745926,-3.26500508439965,67.499288236394));
#61441=CARTESIAN_POINT('Ctrl Pts',(7.20272875509302,-3.27179998690852,67.4989905829124));
#61442=CARTESIAN_POINT('Ctrl Pts',(7.19477524597916,-3.28926553305072,67.4982258786636));
#61443=CARTESIAN_POINT('Ctrl Pts',(7.18989028386523,-3.29992974086019,67.4977593278664));
#61444=CARTESIAN_POINT('Ctrl Pts',(7.16128061824754,-3.36202149829367,67.4950449636154));
#61445=CARTESIAN_POINT('Ctrl Pts',(7.13702762745633,-3.41320457427152,67.4928159100865));
#61446=CARTESIAN_POINT('Ctrl Pts',(6.72876861081588,-4.25140526080209,67.4564375544603));
#61447=CARTESIAN_POINT('Ctrl Pts',(6.21733959113934,-4.96943763013283,67.4280391085575));
#61448=CARTESIAN_POINT('Ctrl Pts',(5.43485615499623,-5.75326456697196,67.3892094787069));
#61449=CARTESIAN_POINT('Ctrl Pts',(5.26386324736674,-5.91011395545199,67.3808774830197));
#61450=CARTESIAN_POINT('Ctrl Pts',(5.00540980646068,-6.12706539534449,67.3680950536652));
#61451=CARTESIAN_POINT('Ctrl Pts',(4.92323511246187,-6.19328765606045,67.3640046901931));
#61452=CARTESIAN_POINT('Ctrl Pts',(4.83028269945863,-6.26517627037266,67.3593187354782));
#61453=CARTESIAN_POINT('Ctrl Pts',(4.8207850884402,-6.27248720872898,67.3588392634721));
#61454=CARTESIAN_POINT('Ctrl Pts',(4.80621128289297,-6.28365297669245,67.3581024345928));
#61455=CARTESIAN_POINT('Ctrl Pts',(4.80114694836999,-6.28752332854597,67.3578461882604));
#61456=CARTESIAN_POINT('Ctrl Pts',(4.79173898605905,-6.29469524735209,67.3573697772519));
#61457=CARTESIAN_POINT('Ctrl Pts',(4.78739663434703,-6.29799843066742,67.3571497316832));
#61458=CARTESIAN_POINT('Ctrl Pts',(4.78023993206646,-6.30343078375762,67.356786819352));
#61459=CARTESIAN_POINT('Ctrl Pts',(4.77742758846653,-6.30556255148006,67.3566441434874));
#61460=CARTESIAN_POINT('Ctrl Pts',(4.77189906032785,-6.30974737614529,67.3563635470208));
#61461=CARTESIAN_POINT('Ctrl Pts',(4.76918297458713,-6.31180056303822,67.3562256357615));
#61462=CARTESIAN_POINT('Ctrl Pts',(4.76290964748358,-6.31653643547735,67.3559069701905));
#61463=CARTESIAN_POINT('Ctrl Pts',(4.75935146644038,-6.31921786849791,67.3557261272015));
#61464=CARTESIAN_POINT('Ctrl Pts',(4.74796071436577,-6.32778682218729,67.3551468879168));
#61465=CARTESIAN_POINT('Ctrl Pts',(4.7401194953676,-6.33366277758992,67.3547476811499));
#61466=CARTESIAN_POINT('Ctrl Pts',(4.67105454749812,-6.3852177201588,67.3512275456467));
#61467=CARTESIAN_POINT('Ctrl Pts',(4.60918491314709,-6.43002096771147,67.3480469189616));
#61468=CARTESIAN_POINT('Ctrl Pts',(4.52461019155802,-6.48941837247957,67.3436738738866));
#61469=CARTESIAN_POINT('Ctrl Pts',(4.50246333112469,-6.50480377274657,67.3425264436965));
#61470=CARTESIAN_POINT('Ctrl Pts',(4.44617049445471,-6.54348512428783,67.3396050177943));
#61471=CARTESIAN_POINT('Ctrl Pts',(4.41192003930784,-6.56662707253893,67.3378230043631));
#61472=CARTESIAN_POINT('Ctrl Pts',(3.70830047627113,-7.03405072634773,67.3011485962119));
#61473=CARTESIAN_POINT('Ctrl Pts',(2.97527940937981,-7.37409894589128,67.2623019455133));
#61474=CARTESIAN_POINT('Ctrl Pts',(2.13123365980928,-7.61888637607336,67.223575162696));
#61475=CARTESIAN_POINT('Ctrl Pts',(2.05864615567481,-7.63881947014498,67.2202849282014));
#61476=CARTESIAN_POINT('Ctrl Pts',(1.76022682084135,-7.71620501250749,67.2069282617555));
#61477=CARTESIAN_POINT('Ctrl Pts',(1.53218528114985,-7.76470466796158,67.1971226213925));
#61478=CARTESIAN_POINT('Ctrl Pts',(1.26463299644139,-7.80935876665833,67.1860809016005));
#61479=CARTESIAN_POINT('Ctrl Pts',(1.22689943862315,-7.81537579279685,67.1845341286885));
#61480=CARTESIAN_POINT('Ctrl Pts',(1.17820120134105,-7.82277987557015,67.1825511676504));
#61481=CARTESIAN_POINT('Ctrl Pts',(1.1672754894649,-7.82441761317952,67.1821071392955));
#61482=CARTESIAN_POINT('Ctrl Pts',(1.14964662436026,-7.82702239075837,67.1813920691294));
#61483=CARTESIAN_POINT('Ctrl Pts',(1.14294561559971,-7.82800371655567,67.1811205808547));
#61484=CARTESIAN_POINT('Ctrl Pts',(1.13016997693378,-7.82985788414935,67.1806035916863));
#61485=CARTESIAN_POINT('Ctrl Pts',(1.12409557731458,-7.83073226435541,67.1803580428891));
#61486=CARTESIAN_POINT('Ctrl Pts',(1.11023200305203,-7.8327113945868,67.1797982254109));
#61487=CARTESIAN_POINT('Ctrl Pts',(1.10244218013375,-7.83381159662447,67.1794840989437));
#61488=CARTESIAN_POINT('Ctrl Pts',(1.07918307475748,-7.83706123551461,67.1785474482309));
#61489=CARTESIAN_POINT('Ctrl Pts',(1.06370901392733,-7.83917649088735,67.1779259907163));
#61490=CARTESIAN_POINT('Ctrl Pts',(0.955453308429607,-7.85364826518484,
67.1735899930467));
#61491=CARTESIAN_POINT('Ctrl Pts',(0.862463304555911,-7.86440333918357,
67.1699255647607));
#61492=CARTESIAN_POINT('Ctrl Pts',(0.719489402636579,-7.87837299262084,
67.1643769300196));
#61493=CARTESIAN_POINT('Ctrl Pts',(0.669630958021547,-7.88276731213581,
67.162457857266));
#61494=CARTESIAN_POINT('Ctrl Pts',(0.563476439129206,-7.89110890281257,
67.1584038618069));
#61495=CARTESIAN_POINT('Ctrl Pts',(0.507172964847898,-7.89492755762467,
67.156272727584));
#61496=CARTESIAN_POINT('Ctrl Pts',(0.399609179556531,-7.90106739068111,
67.1522350412394));
#61497=CARTESIAN_POINT('Ctrl Pts',(0.348357864035457,-7.90349291811474,
67.1503257662165));
#61498=CARTESIAN_POINT('Ctrl Pts',(-0.383391119345756,-7.9309920828275,
67.1232564823845));
#61499=CARTESIAN_POINT('Ctrl Pts',(-1.06426157097136,-7.86860256756077,
67.1007311374372));
#61500=CARTESIAN_POINT('Ctrl Pts',(-1.9080332944433,-7.67965476527742,67.069961695459));
#61501=CARTESIAN_POINT('Ctrl Pts',(-2.0858910055835,-7.6332654696956,67.063287981003));
#61502=CARTESIAN_POINT('Ctrl Pts',(-2.37897639460787,-7.54581361684718,
67.05175294653));
#61503=CARTESIAN_POINT('Ctrl Pts',(-2.49515957289562,-7.50819605923408,
67.0470359396797));
#61504=CARTESIAN_POINT('Ctrl Pts',(-2.62939890116315,-7.46127245208345,
67.0413688874191));
#61505=CARTESIAN_POINT('Ctrl Pts',(-2.64835171619549,-7.45456627576543,
67.0405636820065));
#61506=CARTESIAN_POINT('Ctrl Pts',(-2.67298954034492,-7.44574272420475,
67.0395100726196));
#61507=CARTESIAN_POINT('Ctrl Pts',(-2.67869810482986,-7.44369090308348,
67.0392654704491));
#61508=CARTESIAN_POINT('Ctrl Pts',(-2.68795649606905,-7.44035114328275,
67.0388679742034));
#61509=CARTESIAN_POINT('Ctrl Pts',(-2.69150777934348,-7.43906722202124,
67.0387153159681));
#61510=CARTESIAN_POINT('Ctrl Pts',(-2.6983244821171,-7.43659720967967,67.038421922945));
#61511=CARTESIAN_POINT('Ctrl Pts',(-2.70159003394883,-7.43541151235972,
67.0382812114222));
#61512=CARTESIAN_POINT('Ctrl Pts',(-2.70908376487301,-7.43268500654611,
67.0379579404018));
#61513=CARTESIAN_POINT('Ctrl Pts',(-2.71331140991337,-7.4311427414865,67.0377752951474));
#61514=CARTESIAN_POINT('Ctrl Pts',(-2.72455117517701,-7.42703155124166,
67.0372889958287));
#61515=CARTESIAN_POINT('Ctrl Pts',(-2.73156096208925,-7.42445630864336,
67.0369849728667));
#61516=CARTESIAN_POINT('Ctrl Pts',(-2.77828163959225,-7.40721702946232,
67.0349537707147));
#61517=CARTESIAN_POINT('Ctrl Pts',(-2.81787727934781,-7.39224461898516,
67.0332088572557));
#61518=CARTESIAN_POINT('Ctrl Pts',(-3.58184127039359,-7.09633492288994,
66.9991141327769));
#61519=CARTESIAN_POINT('Ctrl Pts',(-4.26104161191115,-6.71052669220169,
66.961774082844));
#61520=CARTESIAN_POINT('Ctrl Pts',(-5.12736918834453,-6.03308995772376,
66.9124971469583));
#61521=CARTESIAN_POINT('Ctrl Pts',(-5.36922694756987,-5.81889345126023,
66.8984474872653));
#61522=CARTESIAN_POINT('Ctrl Pts',(-5.67762462484864,-5.51011858376345,
66.880263990129));
#61523=CARTESIAN_POINT('Ctrl Pts',(-5.75617084761759,-5.42801315025172,
66.8756046517084));
#61524=CARTESIAN_POINT('Ctrl Pts',(-5.84324540770193,-5.33297642586478,
66.8704044451791));
#61525=CARTESIAN_POINT('Ctrl Pts',(-5.85353457242243,-5.32168088730323,
66.8697893870546));
#61526=CARTESIAN_POINT('Ctrl Pts',(-5.86895261327634,-5.30465600680504,
66.8688668556361));
#61527=CARTESIAN_POINT('Ctrl Pts',(-5.87410593765565,-5.29894891096811,
66.8685583595507));
#61528=CARTESIAN_POINT('Ctrl Pts',(-5.88295845250713,-5.28911632972766,
66.8680281573179));
#61529=CARTESIAN_POINT('Ctrl Pts',(-5.88666163967655,-5.28499446011311,
66.86780628445));
#61530=CARTESIAN_POINT('Ctrl Pts',(-5.89428234049941,-5.27649421561489,
66.8673495345632));
#61531=CARTESIAN_POINT('Ctrl Pts',(-5.89819931372861,-5.27211536033217,
66.8671146800983));
#61532=CARTESIAN_POINT('Ctrl Pts',(-5.90762172562808,-5.26155823189152,
66.8665495134014));
#61533=CARTESIAN_POINT('Ctrl Pts',(-5.91312236067572,-5.25537566962838,
66.8662194008167));
#61534=CARTESIAN_POINT('Ctrl Pts',(-5.93322814389547,-5.23270579463592,
66.8650121200683));
#61535=CARTESIAN_POINT('Ctrl Pts',(-5.9477741817461,-5.21616606652942,66.8641374004957));
#61536=CARTESIAN_POINT('Ctrl Pts',(-6.18469580862659,-4.94449218256167,
66.8498684916393));
#61537=CARTESIAN_POINT('Ctrl Pts',(-6.3905521852358,-4.67539698622458,66.8371780757865));
#61538=CARTESIAN_POINT('Ctrl Pts',(-6.80283504860003,-4.05812943447416,
66.8104316711447));
#61539=CARTESIAN_POINT('Ctrl Pts',(-7.00108142342318,-3.70565090907486,
66.7966332241711));
#61540=CARTESIAN_POINT('Ctrl Pts',(-7.38973486476031,-2.8710402448608,66.7649668980283));
#61541=CARTESIAN_POINT('Ctrl Pts',(-7.56145389410808,-2.38229830374398,
66.7471165660588));
#61542=CARTESIAN_POINT('Ctrl Pts',(-7.68964230681711,-1.85844878422692,
66.7256628567245));
#61543=CARTESIAN_POINT('Ctrl Pts',(-7.69491456177336,-1.83649681686598,
66.7247596143042));
#61544=CARTESIAN_POINT('Ctrl Pts',(-7.70152331106617,-1.80845198727906,
66.723599957476));
#61545=CARTESIAN_POINT('Ctrl Pts',(-7.70294670845239,-1.80237951262106,
66.7233485184985));
#61546=CARTESIAN_POINT('Ctrl Pts',(-7.70521690975511,-1.79264260766185,
66.7229447928263));
#61547=CARTESIAN_POINT('Ctrl Pts',(-7.70606828674644,-1.78897923551097,
66.7227927706842));
#61548=CARTESIAN_POINT('Ctrl Pts',(-7.70767704262457,-1.78203449675327,
66.7225043375755));
#61549=CARTESIAN_POINT('Ctrl Pts',(-7.70843493955274,-1.77875324978937,
66.7223679568046));
#61550=CARTESIAN_POINT('Ctrl Pts',(-7.71014712446851,-1.77131885283397,
66.7220587226871));
#61551=CARTESIAN_POINT('Ctrl Pts',(-7.71110015168522,-1.76716541667691,
66.7218857955945));
#61552=CARTESIAN_POINT('Ctrl Pts',(-7.71355383413197,-1.75643212067998,
66.7214384879769));
#61553=CARTESIAN_POINT('Ctrl Pts',(-7.71504942081288,-1.74985113086354,
66.721163808711));
#61554=CARTESIAN_POINT('Ctrl Pts',(-7.72414175752318,-1.7096041130958,66.7194814480187));
#61555=CARTESIAN_POINT('Ctrl Pts',(-7.73152644974159,-1.67589104674753,
66.7180614423544));
#61556=CARTESIAN_POINT('Ctrl Pts',(-7.85334861415972,-1.10179321287086,
66.6937110512951));
#61557=CARTESIAN_POINT('Ctrl Pts',(-7.91109258458655,-0.550968866681914,
66.6679033779296));
#61558=CARTESIAN_POINT('Ctrl Pts',(-7.91089005426597,0.655736935955637,
66.6120946576746));
#61559=CARTESIAN_POINT('Ctrl Pts',(-7.82958133489435,1.30770847290239,66.5825653318638));
#61560=CARTESIAN_POINT('Ctrl Pts',(-7.65798626123248,1.98522778643018,66.5540587658793));
#61561=CARTESIAN_POINT('Ctrl Pts',(-7.64675081407073,2.02807421328028,66.5522641190122));
#61562=CARTESIAN_POINT('Ctrl Pts',(-7.63207438100254,2.08218640665378,66.5500076188406));
#61563=CARTESIAN_POINT('Ctrl Pts',(-7.62896741199729,2.09354145349253,66.5495346687731));
#61564=CARTESIAN_POINT('Ctrl Pts',(-7.62401570662342,2.1114810591777,66.5487883424342));
#61565=CARTESIAN_POINT('Ctrl Pts',(-7.62218776572446,2.11807021188144,66.5485144068926));
#61566=CARTESIAN_POINT('Ctrl Pts',(-7.61879302936558,2.13024586357164,66.5480085645146));
#61567=CARTESIAN_POINT('Ctrl Pts',(-7.61722862772925,2.13583302171916,66.5477765780554));
#61568=CARTESIAN_POINT('Ctrl Pts',(-7.61374842710794,2.1482098730685,66.547262970415));
#61569=CARTESIAN_POINT('Ctrl Pts',(-7.6118296885436,2.15499873851126,66.5469814475543));
#61570=CARTESIAN_POINT('Ctrl Pts',(-7.6063264186957,2.17437131382389,66.5461786602874));
#61571=CARTESIAN_POINT('Ctrl Pts',(-7.60271973838712,2.18694873735875,66.5456581360065));
#61572=CARTESIAN_POINT('Ctrl Pts',(-7.579714404026,2.26642955223683,66.5423730000273));
#61573=CARTESIAN_POINT('Ctrl Pts',(-7.55946372008898,2.33308421321055,66.539636993923));
#61574=CARTESIAN_POINT('Ctrl Pts',(-7.49733577381843,2.52827001211136,66.5316765246582));
#61575=CARTESIAN_POINT('Ctrl Pts',(-7.45304096448978,2.6560074304315,66.5265334227416));
#61576=CARTESIAN_POINT('Ctrl Pts',(-7.33980074703697,2.95738542198601,66.5145183578765));
#61577=CARTESIAN_POINT('Ctrl Pts',(-7.26793571848666,3.12984317430211,66.5077404830479));
#61578=CARTESIAN_POINT('Ctrl Pts',(-7.01715963707973,3.67629946893593,66.486366981675));
#61579=CARTESIAN_POINT('Ctrl Pts',(-6.81494828728814,4.03883532749926,66.4723817100936));
#61580=CARTESIAN_POINT('Ctrl Pts',(-6.33613707954847,4.75808855139636,66.4426852165574));
#61581=CARTESIAN_POINT('Ctrl Pts',(-6.05558270157148,5.11036893659748,66.4269680597869));
#61582=CARTESIAN_POINT('Ctrl Pts',(-5.72661530530558,5.45808117848825,66.4080035600071));
#61583=CARTESIAN_POINT('Ctrl Pts',(-5.70643796006051,5.47917318322084,66.4068383239828));
#61584=CARTESIAN_POINT('Ctrl Pts',(-5.68173905485941,5.50470730057592,66.4054087861052));
#61585=CARTESIAN_POINT('Ctrl Pts',(-5.67732804936663,5.50925651716915,66.4051533607586));
#61586=CARTESIAN_POINT('Ctrl Pts',(-5.6700654376369,5.51672870534834,66.4047325980703));
#61587=CARTESIAN_POINT('Ctrl Pts',(-5.66721701904365,5.51965478398972,66.4045675203916));
#61588=CARTESIAN_POINT('Ctrl Pts',(-5.66209247050693,5.52491090111962,66.4042704329761));
#61589=CARTESIAN_POINT('Ctrl Pts',(-5.65981716280006,5.52724174371747,66.4041384908344));
#61590=CARTESIAN_POINT('Ctrl Pts',(-5.65496254460128,5.53220871092019,66.4038569018087));
#61591=CARTESIAN_POINT('Ctrl Pts',(-5.65238283594739,5.53484443121317,66.4037072215481));
#61592=CARTESIAN_POINT('Ctrl Pts',(-5.64538557486457,5.54198362567672,66.4033011032379));
#61593=CARTESIAN_POINT('Ctrl Pts',(-5.64096448309388,5.54648361542504,66.4030443731792));
#61594=CARTESIAN_POINT('Ctrl Pts',(-5.6189437067743,5.56884380788051,66.4017650100703));
#61595=CARTESIAN_POINT('Ctrl Pts',(-5.60126474090482,5.58662536876952,66.4007358983747));
#61596=CARTESIAN_POINT('Ctrl Pts',(-5.45079467668902,5.73653642085184,66.3919625437275));
#61597=CARTESIAN_POINT('Ctrl Pts',(-5.31344183571156,5.86398662616408,66.3838607627234));
#61598=CARTESIAN_POINT('Ctrl Pts',(-5.01696805963021,6.12011161225012,66.366435329072));
#61599=CARTESIAN_POINT('Ctrl Pts',(-4.857111369941,6.24773536539808,66.3570747924512));
#61600=CARTESIAN_POINT('Ctrl Pts',(-4.55102381369818,6.47325132871581,66.339471771655));
#61601=CARTESIAN_POINT('Ctrl Pts',(-4.40611723015186,6.57274148427782,66.3312615985282));
#61602=CARTESIAN_POINT('Ctrl Pts',(-3.80684380750867,6.95546147392947,66.2980877482013));
#61603=CARTESIAN_POINT('Ctrl Pts',(-3.32753611475839,7.19709205084432,66.2734288323677));
#61604=CARTESIAN_POINT('Ctrl Pts',(-2.63674050532818,7.46144874001913,66.2417255529085));
#61605=CARTESIAN_POINT('Ctrl Pts',(-2.44326791912679,7.5270225287051,66.2332162504104));
#61606=CARTESIAN_POINT('Ctrl Pts',(-2.22926265058221,7.59043275440089,66.2241927791821));
#61607=CARTESIAN_POINT('Ctrl Pts',(-2.21104212489442,7.59576027090131,66.2234275277023));
#61608=CARTESIAN_POINT('Ctrl Pts',(-2.18547415538237,7.60313631934836,66.2223578727714));
#61609=CARTESIAN_POINT('Ctrl Pts',(-2.17814273001472,7.60523986620684,66.2220516385642));
#61610=CARTESIAN_POINT('Ctrl Pts',(-2.16543288040593,7.6088667150911,66.2215215782053));
#61611=CARTESIAN_POINT('Ctrl Pts',(-2.16005586860403,7.61039492354056,66.2212975890711));
#61612=CARTESIAN_POINT('Ctrl Pts',(-2.14888239489348,7.61355775729978,66.2208326712037));
#61613=CARTESIAN_POINT('Ctrl Pts',(-2.1430856757498,7.61519146557947,66.2205917730263));
#61614=CARTESIAN_POINT('Ctrl Pts',(-2.12946442220123,7.6190136032769,66.2200264029842));
#61615=CARTESIAN_POINT('Ctrl Pts',(-2.12163836407965,7.62119660321936,66.2197021113083));
#61616=CARTESIAN_POINT('Ctrl Pts',(-2.096188811041,7.62825326058703,66.2186492958385));
#61617=CARTESIAN_POINT('Ctrl Pts',(-2.07855171896932,7.63307789142871,66.2179223951527));
#61618=CARTESIAN_POINT('Ctrl Pts',(-1.56914799898355,7.77052891315829,66.1970054069954));
#61619=CARTESIAN_POINT('Ctrl Pts',(-1.06570584867169,7.85542426181188,66.1785325924315));
#61620=CARTESIAN_POINT('Ctrl Pts',(0.159150779709888,7.94196668774283,66.1356988099988));
#61621=CARTESIAN_POINT('Ctrl Pts',(0.879317484782621,7.89472518917485,66.1122960571025));
#61622=CARTESIAN_POINT('Ctrl Pts',(1.62666303722671,7.74208407100822,66.0822990366393));
#61623=CARTESIAN_POINT('Ctrl Pts',(1.67015494030046,7.73281842086246,66.0805314033459));
#61624=CARTESIAN_POINT('Ctrl Pts',(1.72218932271921,7.72127340314833,66.0783920044124));
#61625=CARTESIAN_POINT('Ctrl Pts',(1.73080980152335,7.71934559787622,66.0780367618677));
#61626=CARTESIAN_POINT('Ctrl Pts',(1.74484411557498,7.71618240117225,66.0774571177898));
#61627=CARTESIAN_POINT('Ctrl Pts',(1.75025992691864,7.71495573699591,66.0772331183432));
#61628=CARTESIAN_POINT('Ctrl Pts',(1.75990338118739,7.71276084805908,66.0768337044654));
#61629=CARTESIAN_POINT('Ctrl Pts',(1.76413153199991,7.71179484608876,66.0766583911976));
#61630=CARTESIAN_POINT('Ctrl Pts',(1.77302913844042,7.70975431727278,66.076289067136));
#61631=CARTESIAN_POINT('Ctrl Pts',(1.77769841529951,7.70867902448658,66.0760950218924));
#61632=CARTESIAN_POINT('Ctrl Pts',(1.78999339410308,7.70583583564691,66.0755834629921));
#61633=CARTESIAN_POINT('Ctrl Pts',(1.79761744174322,7.70406086485422,66.0752656342688));
#61634=CARTESIAN_POINT('Ctrl Pts',(1.83170418218451,7.69607170444554,66.0738419265431));
#61635=CARTESIAN_POINT('Ctrl Pts',(1.85813716877952,7.68973251338095,66.0727305828458));
#61636=CARTESIAN_POINT('Ctrl Pts',(2.05696284217316,7.64096487874032,66.0643185323845));
#61637=CARTESIAN_POINT('Ctrl Pts',(2.22790946943088,7.59288182224325,66.0567883031286));
#61638=CARTESIAN_POINT('Ctrl Pts',(2.83381579837784,7.40023137470824,66.029327806374));
#61639=CARTESIAN_POINT('Ctrl Pts',(3.2576505771805,7.22368672858054,66.0087263139449));
#61640=CARTESIAN_POINT('Ctrl Pts',(4.12640949275155,6.76971866602819,65.9655569451721));
#61641=CARTESIAN_POINT('Ctrl Pts',(4.56397830033079,6.48278791626769,65.9432578712934));
#61642=CARTESIAN_POINT('Ctrl Pts',(4.99569295035043,6.13417094442863,65.9207741625339));
#61643=CARTESIAN_POINT('Ctrl Pts',(5.02113481454038,6.11336293919424,65.9194467149308));
#61644=CARTESIAN_POINT('Ctrl Pts',(5.05696115562571,6.08368731010578,65.917573751928));
#61645=CARTESIAN_POINT('Ctrl Pts',(5.06745336739912,6.0749505172856,65.9170247768184));
#61646=CARTESIAN_POINT('Ctrl Pts',(5.08527653798075,6.0600309817093,65.9160914343758));
#61647=CARTESIAN_POINT('Ctrl Pts',(5.0926189567968,6.05386200110572,65.9157067042587));
#61648=CARTESIAN_POINT('Ctrl Pts',(5.10732085843323,6.04146402874386,65.9149358762265));
#61649=CARTESIAN_POINT('Ctrl Pts',(5.11468020910902,6.03523490186752,65.9145497825033));
#61650=CARTESIAN_POINT('Ctrl Pts',(5.13228823731932,6.02027571606978,65.9136254353891));
#61651=CARTESIAN_POINT('Ctrl Pts',(5.14252606429163,6.01153290999979,65.9130875226745));
#61652=CARTESIAN_POINT('Ctrl Pts',(5.17735099927239,5.98163936605093,65.9112561443866));
#61653=CARTESIAN_POINT('Ctrl Pts',(5.20183043415213,5.96036349819083,65.9099660587199));
#61654=CARTESIAN_POINT('Ctrl Pts',(5.56223936653641,5.6432088938309,65.8909302454142));
#61655=CARTESIAN_POINT('Ctrl Pts',(5.87260253269959,5.31948245807064,65.8740605656661));
#61656=CARTESIAN_POINT('Ctrl Pts',(6.55426582120358,4.47564338644807,65.8343161857849));
#61657=CARTESIAN_POINT('Ctrl Pts',(6.89323408049747,3.93357050236585,65.8121469050521));
#61658=CARTESIAN_POINT('Ctrl Pts',(7.20358061721953,3.27127866018645,65.783826096306));
#61659=CARTESIAN_POINT('Ctrl Pts',(7.24211326519641,3.18506393607554,65.7801131023004));
#61660=CARTESIAN_POINT('Ctrl Pts',(7.28394685596344,3.08677709767737,65.7758312406306));
#61661=CARTESIAN_POINT('Ctrl Pts',(7.28877451360614,3.07536026158793,65.7753331258333));
#61662=CARTESIAN_POINT('Ctrl Pts',(7.2957785875294,3.05868732704689,65.7746045508147));
#61663=CARTESIAN_POINT('Ctrl Pts',(7.29797621400613,3.05344011607293,65.7743750937799));
#61664=CARTESIAN_POINT('Ctrl Pts',(7.30185194375157,3.04415805890376,65.7739688988962));
#61665=CARTESIAN_POINT('Ctrl Pts',(7.30353236902722,3.04012418011427,65.7737922721432));
#61666=CARTESIAN_POINT('Ctrl Pts',(7.30700637991229,3.03176527566995,65.7734260619754));
#61667=CARTESIAN_POINT('Ctrl Pts',(7.3087994695217,3.02744004680772,65.773236454759));
#61668=CARTESIAN_POINT('Ctrl Pts',(7.31339302995311,3.01633175266325,65.7727491929033));
#61669=CARTESIAN_POINT('Ctrl Pts',(7.31618790003867,3.00954638832292,65.7724512661382));
#61670=CARTESIAN_POINT('Ctrl Pts',(7.32763941219574,2.98163427042889,65.7712245006141));
#61671=CARTESIAN_POINT('Ctrl Pts',(7.33621395232553,2.96047413537408,65.7702916187018));
#61672=CARTESIAN_POINT('Ctrl Pts',(7.3905962671344,2.82458304382312,65.7642806379654));
#61673=CARTESIAN_POINT('Ctrl Pts',(7.43379768561378,2.70884272530146,65.7590603389057));
#61674=CARTESIAN_POINT('Ctrl Pts',(7.52030217422378,2.45941321864593,65.7476522567079));
#61675=CARTESIAN_POINT('Ctrl Pts',(7.56278976212658,2.3254819431823,65.7414353092094));
#61676=CARTESIAN_POINT('Ctrl Pts',(7.68937808901607,1.88618192752425,65.7209018695115));
#61677=CARTESIAN_POINT('Ctrl Pts',(7.75871444421833,1.57688309699188,65.7062362304532));
#61678=CARTESIAN_POINT('Ctrl Pts',(7.90835065262444,0.65258773733756,65.6631082614545));
#61679=CARTESIAN_POINT('Ctrl Pts',(7.93518243310435,0.0313038399315663,
65.6352078284755));
#61680=CARTESIAN_POINT('Ctrl Pts',(7.88471613501784,-0.647175869606253,
65.6072831967041));
#61681=CARTESIAN_POINT('Ctrl Pts',(7.87953331836288,-0.707488542760406,
65.6048207161513));
#61682=CARTESIAN_POINT('Ctrl Pts',(7.87248723459751,-0.779750892207637,
65.6018937001239));
#61683=CARTESIAN_POINT('Ctrl Pts',(7.87128826838524,-0.791762407855548,
65.601407942929));
#61684=CARTESIAN_POINT('Ctrl Pts',(7.86928982409767,-0.811330017020597,
65.6006178645159));
#61685=CARTESIAN_POINT('Ctrl Pts',(7.86850694620996,-0.818887764005264,
65.6003130115811));
#61686=CARTESIAN_POINT('Ctrl Pts',(7.86709215416323,-0.832356520317786,
65.5997702710113));
#61687=CARTESIAN_POINT('Ctrl Pts',(7.86646446399809,-0.838267961854198,
65.5995322480565));
#61688=CARTESIAN_POINT('Ctrl Pts',(7.86514231737033,-0.850587368597784,
65.5990365962943));
#61689=CARTESIAN_POINT('Ctrl Pts',(7.86444669143068,-0.85699520536097,65.5987790052243));
#61690=CARTESIAN_POINT('Ctrl Pts',(7.86260600020357,-0.87375995679363,65.5981056411469));
#61691=CARTESIAN_POINT('Ctrl Pts',(7.86144830055577,-0.884115487543032,
65.5976902743716));
#61692=CARTESIAN_POINT('Ctrl Pts',(7.85887777857409,-0.906704312140545,
65.5967854541167));
#61693=CARTESIAN_POINT('Ctrl Pts',(7.85745684398556,-0.918936665346535,
65.5962962622859));
#61694=CARTESIAN_POINT('Ctrl Pts',(7.85322258853049,-0.95465999839684,65.5948699130692));
#61695=CARTESIAN_POINT('Ctrl Pts',(7.85033243329407,-0.978141828640588,
65.5939352272318));
#61696=CARTESIAN_POINT('Ctrl Pts',(7.7744338475608,-1.57278594691258,65.5703375843208));
#61697=CARTESIAN_POINT('Ctrl Pts',(7.63939349205951,-2.13430009453654,65.5499193941914));
#61698=CARTESIAN_POINT('Ctrl Pts',(7.21837545121001,-3.30546001013523,65.507372771856));
#61699=CARTESIAN_POINT('Ctrl Pts',(6.91334759674717,-3.90338366838295,65.4856411473921));
#61700=CARTESIAN_POINT('Ctrl Pts',(6.50150692742712,-4.50757851728124,65.4572120729399));
#61701=CARTESIAN_POINT('Ctrl Pts',(6.46555920906736,-4.55899113076703,65.4547351512214));
#61702=CARTESIAN_POINT('Ctrl Pts',(6.42427971641129,-4.61655898623468,65.4518895875639));
#61703=CARTESIAN_POINT('Ctrl Pts',(6.41954453482423,-4.62314121702876,65.4515631537998));
#61704=CARTESIAN_POINT('Ctrl Pts',(6.41237754463379,-4.63307158900949,65.4510690302293));
#61705=CARTESIAN_POINT('Ctrl Pts',(6.40995320392804,-4.63642513657832,65.4509018777105));
#61706=CARTESIAN_POINT('Ctrl Pts',(6.40573740872022,-4.64224714477417,65.4506111921949));
#61707=CARTESIAN_POINT('Ctrl Pts',(6.40394716042954,-4.64471646809879,65.450487746564));
#61708=CARTESIAN_POINT('Ctrl Pts',(6.40019871686216,-4.64988048023665,65.4502292632825));
#61709=CARTESIAN_POINT('Ctrl Pts',(6.3982402551412,-4.65257495729345,65.4500942064135));
#61710=CARTESIAN_POINT('Ctrl Pts',(6.3935827714855,-4.65897428140715,65.4497730100365));
#61711=CARTESIAN_POINT('Ctrl Pts',(6.39088223283296,-4.66267801767797,65.4495867610095));
#61712=CARTESIAN_POINT('Ctrl Pts',(6.38186200845938,-4.6750265213773,65.4489646315706));
#61713=CARTESIAN_POINT('Ctrl Pts',(6.375528013643,-4.68366077077349,65.4485277264112));
#61714=CARTESIAN_POINT('Ctrl Pts',(6.18880852938391,-4.93710873807688,65.4356475814128));
#61715=CARTESIAN_POINT('Ctrl Pts',(5.99448912529731,-5.17131124723761,65.4222327115985));
#61716=CARTESIAN_POINT('Ctrl Pts',(5.74316731692485,-5.44096685953509,65.4054992728906));
#61717=CARTESIAN_POINT('Ctrl Pts',(5.69856228120195,-5.48766607509887,65.4025505532815));
#61718=CARTESIAN_POINT('Ctrl Pts',(5.5677386741146,-5.62131658754398,65.3939752088805));
#61719=CARTESIAN_POINT('Ctrl Pts',(5.48006713143088,-5.70681853381715,65.3883182276661));
#61720=CARTESIAN_POINT('Ctrl Pts',(5.33823003196128,-5.83886212341088,65.3793474398773));
#61721=CARTESIAN_POINT('Ctrl Pts',(5.28535748264227,-5.88676541437934,65.3760413591992));
#61722=CARTESIAN_POINT('Ctrl Pts',(5.21068701387108,-5.95260089724688,65.3714310969771));
#61723=CARTESIAN_POINT('Ctrl Pts',(5.18943013167645,-5.97114155832867,65.3701251721931));
#61724=CARTESIAN_POINT('Ctrl Pts',(5.14793064829591,-6.00694921883984,65.3675887389204));
#61725=CARTESIAN_POINT('Ctrl Pts',(5.1276991866357,-6.02422857571521,65.3663581711255));
#61726=CARTESIAN_POINT('Ctrl Pts',(5.08815054670785,-6.05766284306286,65.3639646379976));
#61727=CARTESIAN_POINT('Ctrl Pts',(5.06884263369266,-6.07382823804599,65.3628015940133));
#61728=CARTESIAN_POINT('Ctrl Pts',(4.77458884005739,-6.31780955657994,65.3451624517865));
#61729=CARTESIAN_POINT('Ctrl Pts',(4.484588708145,-6.5268609883565,65.3289373829094));
#61730=CARTESIAN_POINT('Ctrl Pts',(3.95414389393391,-6.85713921173142,65.3017365025117));
#61731=CARTESIAN_POINT('Ctrl Pts',(3.71980025115205,-6.9870392305715,65.2904739226519));
#61732=CARTESIAN_POINT('Ctrl Pts',(3.46113863895642,-7.11370855157737,65.2788343496852));
#61733=CARTESIAN_POINT('Ctrl Pts',(3.44294092627836,-7.12253380624951,65.2780195049568));
#61734=CARTESIAN_POINT('Ctrl Pts',(3.41767737679023,-7.13466629936368,65.2768938229362));
#61735=CARTESIAN_POINT('Ctrl Pts',(3.41064027064769,-7.13803297833426,65.2765808616145));
#61736=CARTESIAN_POINT('Ctrl Pts',(3.39853738267738,-7.14380123519055,65.2760436288176));
#61737=CARTESIAN_POINT('Ctrl Pts',(3.39347401288705,-7.14620784426314,65.2758191778843));
#61738=CARTESIAN_POINT('Ctrl Pts',(3.38315054362597,-7.15110112158841,65.2753621774131));
#61739=CARTESIAN_POINT('Ctrl Pts',(3.37789024985902,-7.15358737362752,65.2751296427917));
#61740=CARTESIAN_POINT('Ctrl Pts',(3.36574600419395,-7.15931090984744,65.2745935550495));
#61741=CARTESIAN_POINT('Ctrl Pts',(3.35886011099411,-7.16254407482488,65.2742901486567));
#61742=CARTESIAN_POINT('Ctrl Pts',(3.34438858056131,-7.16931350052565,65.2736536757385));
#61743=CARTESIAN_POINT('Ctrl Pts',(3.33680197100886,-7.1728476669622,65.2733206838029));
#61744=CARTESIAN_POINT('Ctrl Pts',(3.31667107998892,-7.18218664483193,65.2724388800504));
#61745=CARTESIAN_POINT('Ctrl Pts',(3.3041171434833,-7.18797064258925,65.2718908058595));
#61746=CARTESIAN_POINT('Ctrl Pts',(3.26629029106942,-7.20527863805732,65.2702448533724));
#61747=CARTESIAN_POINT('Ctrl Pts',(3.24097165838254,-7.21670251898742,65.2691505075324));
#61748=CARTESIAN_POINT('Ctrl Pts',(3.15086644352229,-7.25678857354164,65.2652815453654));
#61749=CARTESIAN_POINT('Ctrl Pts',(3.08575481346521,-7.28471394799858,65.2625326866272));
#61750=CARTESIAN_POINT('Ctrl Pts',(2.72633876021872,-7.43317825486152,65.2476041381684));
#61751=CARTESIAN_POINT('Ctrl Pts',(2.42533573231901,-7.53676521957365,65.2360135070626));
#61752=CARTESIAN_POINT('Ctrl Pts',(1.36251957969407,-7.83222711536702,65.1970980564306));
#61753=CARTESIAN_POINT('Ctrl Pts',(0.579198370295354,-7.92870708804797,
65.1722442929536));
#61754=CARTESIAN_POINT('Ctrl Pts',(-0.273564968773696,-7.90656299248594,
65.139186186722));
#61755=CARTESIAN_POINT('Ctrl Pts',(-0.341743006582916,-7.90390962495232,
65.1364986228612));
#61756=CARTESIAN_POINT('Ctrl Pts',(-0.419168056529104,-7.89989276568388,
65.1333874507478));
#61757=CARTESIAN_POINT('Ctrl Pts',(-0.428458909871383,-7.89939431413478,
65.1330131483934));
#61758=CARTESIAN_POINT('Ctrl Pts',(-0.442072842881279,-7.8986398421575,
65.1324632353069));
#61759=CARTESIAN_POINT('Ctrl Pts',(-0.446396652284255,-7.89839665901994,
65.1322883681955));
#61760=CARTESIAN_POINT('Ctrl Pts',(-0.454100171094432,-7.89795704569675,
65.1319764379677));
#61761=CARTESIAN_POINT('Ctrl Pts',(-0.457479961458077,-7.8977619960249,
65.1318394540992));
#61762=CARTESIAN_POINT('Ctrl Pts',(-0.464539172974304,-7.89735005821463,
65.1315530728924));
#61763=CARTESIAN_POINT('Ctrl Pts',(-0.468218568974029,-7.89713276808683,
65.1314036526732));
#61764=CARTESIAN_POINT('Ctrl Pts',(-0.477788768900233,-7.89656087924876,
65.1310146118375));
#61765=CARTESIAN_POINT('Ctrl Pts',(-0.483679321172297,-7.89620226066201,
65.1307747639001));
#61766=CARTESIAN_POINT('Ctrl Pts',(-0.508920606365858,-7.89463721289469,
65.1297453521007));
#61767=CARTESIAN_POINT('Ctrl Pts',(-0.528267126489259,-7.89336624878868,
65.1289521834084));
#61768=CARTESIAN_POINT('Ctrl Pts',(-0.663818456408564,-7.88396066731016,
65.1233666373127));
#61769=CARTESIAN_POINT('Ctrl Pts',(-0.779831116300489,-7.87333168455961,
65.1184409503652));
#61770=CARTESIAN_POINT('Ctrl Pts',(-1.17246918751565,-7.82859567815469,
65.1013755944532));
#61771=CARTESIAN_POINT('Ctrl Pts',(-1.44750189101963,-7.78243633116659,
65.0887596766703));
#61772=CARTESIAN_POINT('Ctrl Pts',(-1.89984988559776,-7.6817073234516,65.0674905476054));
#61773=CARTESIAN_POINT('Ctrl Pts',(-2.07872891234743,-7.63524344915277,
65.0589395686552));
#61774=CARTESIAN_POINT('Ctrl Pts',(-2.47380800169171,-7.51770718545703,
65.0399191989619));
#61775=CARTESIAN_POINT('Ctrl Pts',(-2.68890722311049,-7.44348242729305,
65.029473221703));
#61776=CARTESIAN_POINT('Ctrl Pts',(-3.03351346715425,-7.30767767287447,
65.0127617540415));
#61777=CARTESIAN_POINT('Ctrl Pts',(-3.16507080476889,-7.25166780482523,
65.0063868193198));
#61778=CARTESIAN_POINT('Ctrl Pts',(-3.57928239931427,-7.06189842947632,
64.9863800906994));
#61779=CARTESIAN_POINT('Ctrl Pts',(-3.8555697467116,-6.91493188095261,64.9731473074963));
#61780=CARTESIAN_POINT('Ctrl Pts',(-4.14090003389964,-6.74072213798318,
64.9596202169897));
#61781=CARTESIAN_POINT('Ctrl Pts',(-4.15929868149795,-6.72938500309702,
64.9587485252625));
#61782=CARTESIAN_POINT('Ctrl Pts',(-4.18462115509304,-6.71363792322352,
64.9575495294879));
#61783=CARTESIAN_POINT('Ctrl Pts',(-4.19158483518406,-6.70929243257123,
64.9572198824613));
#61784=CARTESIAN_POINT('Ctrl Pts',(-4.20350583180728,-6.70182766314031,
64.9566556942475));
#61785=CARTESIAN_POINT('Ctrl Pts',(-4.2084664642725,-6.69871370665778,64.956420959278));
#61786=CARTESIAN_POINT('Ctrl Pts',(-4.21853670316011,-6.69237667650353,
64.9559445161954));
#61787=CARTESIAN_POINT('Ctrl Pts',(-4.22364608556527,-6.68915325285777,
64.95570282108));
#61788=CARTESIAN_POINT('Ctrl Pts',(-4.23537692500638,-6.68173366383357,
64.9551479934072));
#61789=CARTESIAN_POINT('Ctrl Pts',(-4.24199585220415,-6.67753349984981,
64.9548350073082));
#61790=CARTESIAN_POINT('Ctrl Pts',(-4.25586587566238,-6.66870307223613,
64.9541792767325));
#61791=CARTESIAN_POINT('Ctrl Pts',(-4.26311568601348,-6.66407080286021,
64.9538366061956));
#61792=CARTESIAN_POINT('Ctrl Pts',(-4.28225469898228,-6.65179790917247,
64.9529321770542));
#61793=CARTESIAN_POINT('Ctrl Pts',(-4.2941310323446,-6.64413722097158,64.9523711540824));
#61794=CARTESIAN_POINT('Ctrl Pts',(-4.32967017335749,-6.62107802603943,
64.950692902182));
#61795=CARTESIAN_POINT('Ctrl Pts',(-4.35327125492157,-6.60558456448919,
64.9495791607741));
#61796=CARTESIAN_POINT('Ctrl Pts',(-4.43635414165144,-6.5504042609527,64.9456607916105));
#61797=CARTESIAN_POINT('Ctrl Pts',(-4.49538100309093,-6.51003717433462,
64.9428812497779));
#61798=CARTESIAN_POINT('Ctrl Pts',(-4.8223070819249,-6.27989305886382,64.9274989605675));
#61799=CARTESIAN_POINT('Ctrl Pts',(-5.07874741751383,-6.07437642427691,
64.9154991433005));
#61800=CARTESIAN_POINT('Ctrl Pts',(-5.89656955768259,-5.33085736647997,
64.8762930818178));
#61801=CARTESIAN_POINT('Ctrl Pts',(-6.39122418823901,-4.72646437585342,
64.8512485770037));
#61802=CARTESIAN_POINT('Ctrl Pts',(-6.81167331635576,-4.02328720890917,
64.8190194679026));
#61803=CARTESIAN_POINT('Ctrl Pts',(-6.83322482880398,-3.98657392411261,
64.8173277527226));
#61804=CARTESIAN_POINT('Ctrl Pts',(-6.85821413568586,-3.94320629057885,
64.8153168083088));
#61805=CARTESIAN_POINT('Ctrl Pts',(-6.86194045197115,-3.93671820351944,
64.815015628031));
#61806=CARTESIAN_POINT('Ctrl Pts',(-6.86789534632451,-3.92631567775764,
64.814532194738));
#61807=CARTESIAN_POINT('Ctrl Pts',(-6.87012980160444,-3.92240459391802,
64.8143503134739));
#61808=CARTESIAN_POINT('Ctrl Pts',(-6.87408205203401,-3.91547302584095,
64.8140277465171));
#61809=CARTESIAN_POINT('Ctrl Pts',(-6.87580120185589,-3.91245331048732,
64.8138871470073));
#61810=CARTESIAN_POINT('Ctrl Pts',(-6.87938353052511,-3.90615123685815,
64.813593562851));
#61811=CARTESIAN_POINT('Ctrl Pts',(-6.88124634581206,-3.90286868513731,
64.8134405560029));
#61812=CARTESIAN_POINT('Ctrl Pts',(-6.88609266291181,-3.89431451337888,
64.8130416007666));
#61813=CARTESIAN_POINT('Ctrl Pts',(-6.88907245585836,-3.88904080576171,
64.8127954179079));
#61814=CARTESIAN_POINT('Ctrl Pts',(-6.901877448275,-3.86631733285549,64.8117337132005));
#61815=CARTESIAN_POINT('Ctrl Pts',(-6.91164235389926,-3.84883384778569,
64.8109144350583));
#61816=CARTESIAN_POINT('Ctrl Pts',(-6.98010767235342,-3.72514995203476,
64.8051027533573));
#61817=CARTESIAN_POINT('Ctrl Pts',(-7.0364217919288,-3.61765270278702,64.7999695735854));
#61818=CARTESIAN_POINT('Ctrl Pts',(-7.16446578323156,-3.35892192035464,
64.7874999820108));
#61819=CARTESIAN_POINT('Ctrl Pts',(-7.23391204766382,-3.20662414353978,
64.7800697395181));
#61820=CARTESIAN_POINT('Ctrl Pts',(-7.64464833544654,-2.22447909682973,
64.7320922283271));
#61821=CARTESIAN_POINT('Ctrl Pts',(-7.84758214064166,-1.34354495997937,
64.6897923431192));
#61822=CARTESIAN_POINT('Ctrl Pts',(-7.90045102068861,-0.410105426828256,
64.6514788716379));
#61823=CARTESIAN_POINT('Ctrl Pts',(-7.90229716424221,-0.372843625238695,
64.6499581785528));
#61824=CARTESIAN_POINT('Ctrl Pts',(-7.90500619706137,-0.309036130821233,
64.6473689126054));
#61825=CARTESIAN_POINT('Ctrl Pts',(-7.90599910803566,-0.28249677385192,
64.6462963373018));
#61826=CARTESIAN_POINT('Ctrl Pts',(-7.90718029755614,-0.246007624109232,
64.6448275929709));
#61827=CARTESIAN_POINT('Ctrl Pts',(-7.90748346825854,-0.2360618760573,64.6444278684035));
#61828=CARTESIAN_POINT('Ctrl Pts',(-7.90793582102612,-0.220242085950251,
64.6437930241016));
#61829=CARTESIAN_POINT('Ctrl Pts',(-7.90809722415668,-0.214368419699298,
64.643557525978));
#61830=CARTESIAN_POINT('Ctrl Pts',(-7.90840775836396,-0.202589778265901,
64.6430856956073));
#61831=CARTESIAN_POINT('Ctrl Pts',(-7.90855682021521,-0.196684804787421,
64.6428493656472));
#61832=CARTESIAN_POINT('Ctrl Pts',(-7.90884298812438,-0.184821821521475,
64.6423750081454));
#61833=CARTESIAN_POINT('Ctrl Pts',(-7.90897997552525,-0.17886381258873,
64.6421369844309));
#61834=CARTESIAN_POINT('Ctrl Pts',(-7.9092775596066,-0.165251617995553,
64.6415936647936));
#61835=CARTESIAN_POINT('Ctrl Pts',(-7.90943377820633,-0.157597337334214,
64.6412885046623));
#61836=CARTESIAN_POINT('Ctrl Pts',(-7.90997103444742,-0.12925673130627,
64.6401599298155));
#61837=CARTESIAN_POINT('Ctrl Pts',(-7.91028203238736,-0.108569078050581,
64.6393386854051));
#61838=CARTESIAN_POINT('Ctrl Pts',(-7.91083749197123,-0.0585696182767007,
64.6373599847449));
#61839=CARTESIAN_POINT('Ctrl Pts',(-7.91100020597333,-0.0292571747042206,
64.6362050642762));
#61840=CARTESIAN_POINT('Ctrl Pts',(-7.91099999980433,5.56412939415241E-5,
64.6350551235107));
#61841=CARTESIAN_POINT('',(-7.91099918378876,-0.00359361845736577,60.642331508237));
#61842=CARTESIAN_POINT('Ctrl Pts',(-7.91099999985539,4.78326250410999E-5,
64.6350554298447));
#61843=CARTESIAN_POINT('Ctrl Pts',(-7.91099386948979,1.01394414802377,64.5952802815208));
#61844=CARTESIAN_POINT('Ctrl Pts',(-7.7161184369875,2.01823940527957,64.5634430191512));
#61845=CARTESIAN_POINT('Ctrl Pts',(-7.25761683982437,3.15530437559156,64.5189314313957));
#61846=CARTESIAN_POINT('Ctrl Pts',(-7.17038029084581,3.34881812174155,64.5109668091539));
#61847=CARTESIAN_POINT('Ctrl Pts',(-7.06342309757213,3.56268177758636,64.5014792860627));
#61848=CARTESIAN_POINT('Ctrl Pts',(-7.05124543716367,3.5867234429763,64.5004027211427));
#61849=CARTESIAN_POINT('Ctrl Pts',(-7.03591889424989,3.61660203525023,64.4990517188644));
#61850=CARTESIAN_POINT('Ctrl Pts',(-7.03288507577004,3.62249809915078,64.4987844836784));
#61851=CARTESIAN_POINT('Ctrl Pts',(-7.02807848656479,3.63181065060439,64.4983613815403));
#61852=CARTESIAN_POINT('Ctrl Pts',(-7.02631062344652,3.63522968158852,64.4982058259261));
#61853=CARTESIAN_POINT('Ctrl Pts',(-7.02315352268604,3.64132457864591,64.4979281371314));
#61854=CARTESIAN_POINT('Ctrl Pts',(-7.02176524848077,3.64400094476363,64.4978060655629));
#61855=CARTESIAN_POINT('Ctrl Pts',(-7.01878532974652,3.64973771583157,64.4975441173107));
#61856=CARTESIAN_POINT('Ctrl Pts',(-7.01719321307264,3.65279787420183,64.4974042102566));
#61857=CARTESIAN_POINT('Ctrl Pts',(-7.01262510613737,3.66156408333416,64.4970029207348));
#61858=CARTESIAN_POINT('Ctrl Pts',(-7.0096441787391,3.66726749803442,64.4967412172963));
#61859=CARTESIAN_POINT('Ctrl Pts',(-6.99580720391803,3.69366330284882,64.4955271808382));
#61860=CARTESIAN_POINT('Ctrl Pts',(-6.98486657172159,3.71431097007132,64.4945693983454));
#61861=CARTESIAN_POINT('Ctrl Pts',(-6.97076287027303,3.7406454445837,64.4933377328772));
#61862=CARTESIAN_POINT('Ctrl Pts',(-6.96768394019634,3.74637742956143,64.493069034115));
#61863=CARTESIAN_POINT('Ctrl Pts',(-6.95902591614555,3.76244831430947,64.4923139709411));
#61864=CARTESIAN_POINT('Ctrl Pts',(-6.95343087665174,3.77277855967851,64.491826637168));
#61865=CARTESIAN_POINT('Ctrl Pts',(-6.6382015856957,4.3517102018188,64.4644055592839));
#61866=CARTESIAN_POINT('Ctrl Pts',(-6.259974352022,4.88014042433532,64.4336344177656));
#61867=CARTESIAN_POINT('Ctrl Pts',(-5.60018827487086,5.5972097939344,64.3888481638421));
#61868=CARTESIAN_POINT('Ctrl Pts',(-5.36403780128666,5.82391548487136,64.3740785313534));
#61869=CARTESIAN_POINT('Ctrl Pts',(-4.9814295865403,6.14814703894353,64.3523077657414));
#61870=CARTESIAN_POINT('Ctrl Pts',(-4.8446437454756,6.25649941217763,64.3448995196463));
#61871=CARTESIAN_POINT('Ctrl Pts',(-4.65535150571118,6.39651017091543,64.3351476978341));
#61872=CARTESIAN_POINT('Ctrl Pts',(-4.60590376953269,6.43220729606451,64.3326442639539));
#61873=CARTESIAN_POINT('Ctrl Pts',(-4.53574987897492,6.4816286910602,64.3291534043964));
#61874=CARTESIAN_POINT('Ctrl Pts',(-4.51538499854268,6.4958321855982,64.3281471566339));
#61875=CARTESIAN_POINT('Ctrl Pts',(-4.48448030128063,6.51717112009017,64.3266307881946));
#61876=CARTESIAN_POINT('Ctrl Pts',(-4.47398967261001,6.52437731837421,64.326117901354));
#61877=CARTESIAN_POINT('Ctrl Pts',(-4.45695009307533,6.53602168387213,64.3252878150125));
#61878=CARTESIAN_POINT('Ctrl Pts',(-4.45041181553591,6.54047538462121,64.3249700101159));
#61879=CARTESIAN_POINT('Ctrl Pts',(-4.43784598216374,6.54900732948644,64.3243605808945));
#61880=CARTESIAN_POINT('Ctrl Pts',(-4.43181945982286,6.55308707701844,64.3240688982204));
#61881=CARTESIAN_POINT('Ctrl Pts',(-4.42100270444228,6.56038790077899,64.3235464365189));
#61882=CARTESIAN_POINT('Ctrl Pts',(-4.41621456346552,6.5636120582339,64.3233155379782));
#61883=CARTESIAN_POINT('Ctrl Pts',(-4.40666604234861,6.57002650148381,64.3228558233716));
#61884=CARTESIAN_POINT('Ctrl Pts',(-4.40190571616421,6.57321686126165,64.3226270045019));
#61885=CARTESIAN_POINT('Ctrl Pts',(-4.3888457062231,6.5819491006779,64.3220002424179));
#61886=CARTESIAN_POINT('Ctrl Pts',(-4.38053898250101,6.58748046074524,64.3216027061369));
#61887=CARTESIAN_POINT('Ctrl Pts',(-4.34865491658069,6.60862474867806,64.3200810652362));
#61888=CARTESIAN_POINT('Ctrl Pts',(-4.32500425530015,6.62412702668795,64.3189612272794));
#61889=CARTESIAN_POINT('Ctrl Pts',(-3.95800998285834,6.86187704030903,64.3017196204905));
#61890=CARTESIAN_POINT('Ctrl Pts',(-3.59800988637363,7.05730621796375,64.2866786028816));
#61891=CARTESIAN_POINT('Ctrl Pts',(-3.0306461341968,7.31055131590422,64.2647779435393));
#61892=CARTESIAN_POINT('Ctrl Pts',(-2.83340924322063,7.38923347269942,64.2574628252671));
#61893=CARTESIAN_POINT('Ctrl Pts',(-2.2403075253277,7.59859069643404,64.2359111276538));
#61894=CARTESIAN_POINT('Ctrl Pts',(-1.83704719089428,7.70602235390341,64.221852051876));
#61895=CARTESIAN_POINT('Ctrl Pts',(-1.21199585755554,7.82066944486034,64.1987407775701));
#61896=CARTESIAN_POINT('Ctrl Pts',(-0.995232906795697,7.85119750111191,
64.1904832831767));
#61897=CARTESIAN_POINT('Ctrl Pts',(-0.767004874880943,7.87373708962187,
64.1812821128865));
#61898=CARTESIAN_POINT('Ctrl Pts',(-0.756507140700339,7.87475264237463,
64.1808577688203));
#61899=CARTESIAN_POINT('Ctrl Pts',(-0.741472438960316,7.8761767611683,64.1802483854263));
#61900=CARTESIAN_POINT('Ctrl Pts',(-0.736937061144705,7.87660240958293,
64.1800643442921));
#61901=CARTESIAN_POINT('Ctrl Pts',(-0.729089730281855,7.87733205004603,
64.1797455330635));
#61902=CARTESIAN_POINT('Ctrl Pts',(-0.725777944227535,7.87763787166503,
64.1796108707708));
#61903=CARTESIAN_POINT('Ctrl Pts',(-0.719422389391531,7.87822072342102,
64.1793522212239));
#61904=CARTESIAN_POINT('Ctrl Pts',(-0.716378661517996,7.87849807733375,
64.1792282535316));
#61905=CARTESIAN_POINT('Ctrl Pts',(-0.709188186183988,7.87914909439321,
64.1789351613605));
#61906=CARTESIAN_POINT('Ctrl Pts',(-0.705041314906496,7.87952124682976,
64.1787659480275));
#61907=CARTESIAN_POINT('Ctrl Pts',(-0.690608202694697,7.88080503174254,
64.178176375359));
#61908=CARTESIAN_POINT('Ctrl Pts',(-0.680320511570052,7.88169979366968,
64.1777550262929));
#61909=CARTESIAN_POINT('Ctrl Pts',(-0.560797236933118,7.89185945884062,
64.1728470945995));
#61910=CARTESIAN_POINT('Ctrl Pts',(-0.451386860279121,7.89887251617531,
64.168231657301));
#61911=CARTESIAN_POINT('Ctrl Pts',(-0.335740740402612,7.90387479707518,
64.1632496920286));
#61912=CARTESIAN_POINT('Ctrl Pts',(-0.329610007988939,7.90413283636504,
64.1629852767757));
#61913=CARTESIAN_POINT('Ctrl Pts',(-0.285202427143589,7.90595017217556,
64.1610678083962));
#61914=CARTESIAN_POINT('Ctrl Pts',(-0.246915485981296,7.90723853279353,
64.1594028240778));
#61915=CARTESIAN_POINT('Ctrl Pts',(0.530469085518871,7.9277460963672,64.1253779099398));
#61916=CARTESIAN_POINT('Ctrl Pts',(1.26865250408552,7.84354558166536,64.0894448731624));
#61917=CARTESIAN_POINT('Ctrl Pts',(2.21460367329774,7.59841963969145,64.0453188475074));
#61918=CARTESIAN_POINT('Ctrl Pts',(2.44196588209815,7.52843046875656,64.0348285139961));
#61919=CARTESIAN_POINT('Ctrl Pts',(2.78341406173769,7.40622176143864,64.019322518065));
#61920=CARTESIAN_POINT('Ctrl Pts',(2.89997527433777,7.36136264321405,64.0140736570269));
#61921=CARTESIAN_POINT('Ctrl Pts',(3.0632417961441,7.29404862251231,64.0067839341006));
#61922=CARTESIAN_POINT('Ctrl Pts',(3.11086022325393,7.27386722576488,64.0046653782119));
#61923=CARTESIAN_POINT('Ctrl Pts',(3.17845399733532,7.24443479096087,64.0016685019175));
#61924=CARTESIAN_POINT('Ctrl Pts',(3.19859339992578,7.235565321805,64.0007769128658));
#61925=CARTESIAN_POINT('Ctrl Pts',(3.23397108687755,7.21980828259798,63.9992129871672));
#61926=CARTESIAN_POINT('Ctrl Pts',(3.24922498244686,7.21295623487672,63.9985394128938));
#61927=CARTESIAN_POINT('Ctrl Pts',(3.27157105676704,7.20283311030566,63.9975537406742));
#61928=CARTESIAN_POINT('Ctrl Pts',(3.27868025021575,7.19959983691455,63.9972403183809));
#61929=CARTESIAN_POINT('Ctrl Pts',(3.29091426047964,7.1940139093937,63.996701231573));
#61930=CARTESIAN_POINT('Ctrl Pts',(3.29604136447162,7.19166629664088,63.9964753904016));
#61931=CARTESIAN_POINT('Ctrl Pts',(3.30622575751362,7.18698985944788,63.9960269462288));
#61932=CARTESIAN_POINT('Ctrl Pts',(3.31128310630907,7.18466117429932,63.9958043385356));
#61933=CARTESIAN_POINT('Ctrl Pts',(3.32318366999913,7.17916625729532,63.9952807019857));
#61934=CARTESIAN_POINT('Ctrl Pts',(3.33002483079712,7.17599557421387,63.9949798296979));
#61935=CARTESIAN_POINT('Ctrl Pts',(3.35361728734951,7.16502014018583,63.9939427367428));
#61936=CARTESIAN_POINT('Ctrl Pts',(3.37034582186741,7.1571664481374,63.9932082376562));
#61937=CARTESIAN_POINT('Ctrl Pts',(3.55477904334699,7.06978894979585,63.985119598948));
#61938=CARTESIAN_POINT('Ctrl Pts',(3.71966841235432,6.98444287871347,63.9779748539739));
#61939=CARTESIAN_POINT('Ctrl Pts',(4.28072169493017,6.66853389689715,63.9538265410862));
#61940=CARTESIAN_POINT('Ctrl Pts',(4.65975669480649,6.40941670241914,63.9378595921906));
#61941=CARTESIAN_POINT('Ctrl Pts',(5.28939977977875,5.89344817366404,63.9098137064711));
#61942=CARTESIAN_POINT('Ctrl Pts',(5.54903177527296,5.6496646169731,63.89767430744));
#61943=CARTESIAN_POINT('Ctrl Pts',(5.90859553882458,5.26327202000188,63.8786808015062));
#61944=CARTESIAN_POINT('Ctrl Pts',(6.02167792494257,5.13350984659474,63.8723354901088));
#61945=CARTESIAN_POINT('Ctrl Pts',(6.17076104171189,4.95072722260881,63.863290463233));
#61946=CARTESIAN_POINT('Ctrl Pts',(6.21048817200704,4.9007987631877,63.860809073322));
#61947=CARTESIAN_POINT('Ctrl Pts',(6.27218267299865,4.8213070086398,63.8568335614568));
#61948=CARTESIAN_POINT('Ctrl Pts',(6.29455447052026,4.7920622597193,63.8553661385901));
#61949=CARTESIAN_POINT('Ctrl Pts',(6.32195478545519,4.75572121436434,63.8535377267592));
#61950=CARTESIAN_POINT('Ctrl Pts',(6.32717711541763,4.74877103336481,63.8531878246028));
#61951=CARTESIAN_POINT('Ctrl Pts',(6.33537587813,4.73782210851243,63.8526362789881));
#61952=CARTESIAN_POINT('Ctrl Pts',(6.33836001645364,4.73382912141493,63.8524350658728));
#61953=CARTESIAN_POINT('Ctrl Pts',(6.3436580537528,4.72672598362314,63.852077008739));
#61954=CARTESIAN_POINT('Ctrl Pts',(6.34597344650699,4.72361694502721,63.8519202471015));
#61955=CARTESIAN_POINT('Ctrl Pts',(6.35131405905895,4.71643471979036,63.8515580195688));
#61956=CARTESIAN_POINT('Ctrl Pts',(6.35433764538506,4.71236032483842,63.8513524647364));
#61957=CARTESIAN_POINT('Ctrl Pts',(6.36262652433077,4.70116826931233,63.850787642565));
#61958=CARTESIAN_POINT('Ctrl Pts',(6.36788378119336,4.69404468798553,63.8504279435061));
#61959=CARTESIAN_POINT('Ctrl Pts',(6.39365515127953,4.65900151748875,63.8486575540353));
#61960=CARTESIAN_POINT('Ctrl Pts',(6.4139974556738,4.63095647999794,63.8472378647344));
#61961=CARTESIAN_POINT('Ctrl Pts',(6.86841664702163,3.99573081911279,63.8150330203316));
#61962=CARTESIAN_POINT('Ctrl Pts',(7.21459132249159,3.33027937341748,63.7807128586842));
#61963=CARTESIAN_POINT('Ctrl Pts',(7.59689770166168,2.24393909209498,63.7306458109734));
#61964=CARTESIAN_POINT('Ctrl Pts',(7.70185451943391,1.85191714279034,63.7135659762062));
#61965=CARTESIAN_POINT('Ctrl Pts',(7.78212536859619,1.42247849583244,63.6958736931847));
#61966=CARTESIAN_POINT('Ctrl Pts',(7.7877474341483,1.39136991685154,63.6945974400299));
#61967=CARTESIAN_POINT('Ctrl Pts',(7.79547377165128,1.34710325910973,63.6927887913858));
#61968=CARTESIAN_POINT('Ctrl Pts',(7.7977314736105,1.33397240681414,63.6922532171616));
#61969=CARTESIAN_POINT('Ctrl Pts',(7.80156138916666,1.31135553735924,63.6913323059691));
#61970=CARTESIAN_POINT('Ctrl Pts',(7.80314949768616,1.30187225624173,63.690946642583));
#61971=CARTESIAN_POINT('Ctrl Pts',(7.80629371567735,1.28288432205146,63.6901753893163));
#61972=CARTESIAN_POINT('Ctrl Pts',(7.80784976573041,1.27337967453623,63.6897898014468));
#61973=CARTESIAN_POINT('Ctrl Pts',(7.8113066844272,1.25201958680365,63.6889243169866));
#61974=CARTESIAN_POINT('Ctrl Pts',(7.81319792899082,1.24016260522442,63.6884446191057));
#61975=CARTESIAN_POINT('Ctrl Pts',(7.81967402108194,1.19895849624785,63.686780159549));
#61976=CARTESIAN_POINT('Ctrl Pts',(7.82412059200975,1.16958977833616,63.685598261645));
#61977=CARTESIAN_POINT('Ctrl Pts',(7.87937518285511,0.790220869603066,63.6703881259816));
#61978=CARTESIAN_POINT('Ctrl Pts',(7.9068244351229,0.437210266177055,63.6568858817682));
#61979=CARTESIAN_POINT('Ctrl Pts',(7.91624864564317,-0.455304595667546,
63.62374615972));
#61980=CARTESIAN_POINT('Ctrl Pts',(7.86687042817707,-0.993287822590111,
63.6047467466212));
#61981=CARTESIAN_POINT('Ctrl Pts',(7.70774213273537,-1.8049134457731,63.5742555361342));
#61982=CARTESIAN_POINT('Ctrl Pts',(7.63687206082662,-2.08450597952448,63.5633783022865));
#61983=CARTESIAN_POINT('Ctrl Pts',(7.54700868196269,-2.37207761037149,63.5513062634907));
#61984=CARTESIAN_POINT('Ctrl Pts',(7.54307469003259,-2.38455791561117,63.5507805668073));
#61985=CARTESIAN_POINT('Ctrl Pts',(7.53732814477398,-2.40263189271311,63.5500165994312));
#61986=CARTESIAN_POINT('Ctrl Pts',(7.53554027822042,-2.40823343738295,63.549779458266));
#61987=CARTESIAN_POINT('Ctrl Pts',(7.53240825660417,-2.41800870192283,63.549364969387));
#61988=CARTESIAN_POINT('Ctrl Pts',(7.53106687187501,-2.42218331221409,63.549187750132));
#61989=CARTESIAN_POINT('Ctrl Pts',(7.52846819721708,-2.4302477888818,63.5488449936077));
#61990=CARTESIAN_POINT('Ctrl Pts',(7.52721136117553,-2.43413780135328,63.5486794776092));
#61991=CARTESIAN_POINT('Ctrl Pts',(7.52422388434788,-2.44335985151692,63.5482866523986));
#61992=CARTESIAN_POINT('Ctrl Pts',(7.52249059184378,-2.44869102198768,63.5480592180016));
#61993=CARTESIAN_POINT('Ctrl Pts',(7.51729972731645,-2.46459928580051,63.5473795066422));
#61994=CARTESIAN_POINT('Ctrl Pts',(7.51382551381067,-2.47517089831649,63.5469264341903));
#61995=CARTESIAN_POINT('Ctrl Pts',(7.47739818319091,-2.58523139427013,63.5421948355159));
#61996=CARTESIAN_POINT('Ctrl Pts',(7.44249770121712,-2.6840510691432,63.5378148009425));
#61997=CARTESIAN_POINT('Ctrl Pts',(7.40096487679848,-2.79460497503083,63.5327724174956));
#61998=CARTESIAN_POINT('Ctrl Pts',(7.39625368563849,-2.80704996201716,63.532202813432));
#61999=CARTESIAN_POINT('Ctrl Pts',(7.3825742744057,-2.84291168628154,63.5305558186826));
#62000=CARTESIAN_POINT('Ctrl Pts',(7.3735261457789,-2.86629759954752,63.5294748755323));
#62001=CARTESIAN_POINT('Ctrl Pts',(7.10216940202607,-3.55786150962325,63.4973124365846));
#62002=CARTESIAN_POINT('Ctrl Pts',(6.75024813504183,-4.18729509146563,63.4629170636766));
#62003=CARTESIAN_POINT('Ctrl Pts',(6.07543787764888,-5.0828894855077,63.4127532224534));
#62004=CARTESIAN_POINT('Ctrl Pts',(5.80832422935133,-5.38610652872779,63.3954243789023));
#62005=CARTESIAN_POINT('Ctrl Pts',(5.50913175319859,-5.67746300934643,63.3785323732826));
#62006=CARTESIAN_POINT('Ctrl Pts',(5.49902717940968,-5.6872505641499,63.3779645582292));
#62007=CARTESIAN_POINT('Ctrl Pts',(5.48278067953501,-5.70290357136074,63.3770558740115));
#62008=CARTESIAN_POINT('Ctrl Pts',(5.47665534457708,-5.70878615481774,63.3767142451668));
#62009=CARTESIAN_POINT('Ctrl Pts',(5.46495112424964,-5.71999035423805,63.3760633050793));
#62010=CARTESIAN_POINT('Ctrl Pts',(5.45937391111856,-5.72531369813512,63.3757539174831));
#62011=CARTESIAN_POINT('Ctrl Pts',(5.44984044537626,-5.73438661330298,63.3752264136606));
#62012=CARTESIAN_POINT('Ctrl Pts',(5.44588808866382,-5.73814025942146,63.3750081176793));
#62013=CARTESIAN_POINT('Ctrl Pts',(5.43789256014338,-5.74571809923725,63.3745673064618));
#62014=CARTESIAN_POINT('Ctrl Pts',(5.43384922621532,-5.74954211728927,63.3743447989949));
#62015=CARTESIAN_POINT('Ctrl Pts',(5.42432528555825,-5.75853044651465,63.3738216537178));
#62016=CARTESIAN_POINT('Ctrl Pts',(5.4188413288419,-5.76369120965395,63.3735211718836));
#62017=CARTESIAN_POINT('Ctrl Pts',(5.40265994777439,-5.77887544362545,63.3726367479052));
#62018=CARTESIAN_POINT('Ctrl Pts',(5.3919419943126,-5.78887704457624,63.372053764352));
#62019=CARTESIAN_POINT('Ctrl Pts',(5.30031123459827,-5.87390824924702,63.3670936249897));
#62020=CARTESIAN_POINT('Ctrl Pts',(5.21786276207866,-5.947268847781,63.362789508506));
#62021=CARTESIAN_POINT('Ctrl Pts',(4.41624326512983,-6.63102330214115,63.3223712004803));
#62022=CARTESIAN_POINT('Ctrl Pts',(3.59505534477739,-7.10977555305068,63.2928519502779));
#62023=CARTESIAN_POINT('Ctrl Pts',(2.44847729209401,-7.52766630663646,63.2494133018637));
#62024=CARTESIAN_POINT('Ctrl Pts',(2.18317760616102,-7.60884422009957,63.2391360996766));
#62025=CARTESIAN_POINT('Ctrl Pts',(1.9030926786154,-7.67869064814262,63.2275628635226));
#62026=CARTESIAN_POINT('Ctrl Pts',(1.89198924616834,-7.68143401345262,63.2271028956903));
#62027=CARTESIAN_POINT('Ctrl Pts',(1.87632441958178,-7.68526835372855,63.2264522738007));
#62028=CARTESIAN_POINT('Ctrl Pts',(1.87176789857552,-7.6863793771852,63.2262628215316));
#62029=CARTESIAN_POINT('Ctrl Pts',(1.86396266427317,-7.68827518733989,63.2259379434895));
#62030=CARTESIAN_POINT('Ctrl Pts',(1.86071444492254,-7.68906196648387,63.2258026385819));
#62031=CARTESIAN_POINT('Ctrl Pts',(1.85451332557606,-7.69055983336048,63.2255441322447));
#62032=CARTESIAN_POINT('Ctrl Pts',(1.85156052017422,-7.69127127757958,63.2254209529526));
#62033=CARTESIAN_POINT('Ctrl Pts',(1.84466740737854,-7.69292789356277,63.2251332013336));
#62034=CARTESIAN_POINT('Ctrl Pts',(1.84072678530712,-7.69387173802188,63.224968549599));
#62035=CARTESIAN_POINT('Ctrl Pts',(1.82681955226321,-7.69719145544059,63.2243869322008));
#62036=CARTESIAN_POINT('Ctrl Pts',(1.81684909027408,-7.69955098427875,63.2239689971357));
#62037=CARTESIAN_POINT('Ctrl Pts',(1.71229761515064,-7.72407890233106,63.2195766644576));
#62038=CARTESIAN_POINT('Ctrl Pts',(1.61732403433772,-7.74452190314256,63.2155026220458));
#62039=CARTESIAN_POINT('Ctrl Pts',(1.38592891000282,-7.78988765208269,63.2054166934043));
#62040=CARTESIAN_POINT('Ctrl Pts',(1.2491833889571,-7.81298190173457,63.1993228071755));
#62041=CARTESIAN_POINT('Ctrl Pts',(0.726161255954787,-7.88723082450871,
63.1756956064618));
#62042=CARTESIAN_POINT('Ctrl Pts',(0.336905156081771,-7.91341924702081,
63.1574804741885));
#62043=CARTESIAN_POINT('Ctrl Pts',(-0.417462906007593,-7.90839513239287,
63.1226286602222));
#62044=CARTESIAN_POINT('Ctrl Pts',(-0.781656927756021,-7.88073833424636,
63.1060071737824));
#62045=CARTESIAN_POINT('Ctrl Pts',(-1.39371326583922,-7.7913960768418,63.0790164059279));
#62046=CARTESIAN_POINT('Ctrl Pts',(-1.64286666338273,-7.74269299004363,
63.068292933197));
#62047=CARTESIAN_POINT('Ctrl Pts',(-1.9277192577267,-7.67263889127527,63.0563515270936));
#62048=CARTESIAN_POINT('Ctrl Pts',(-1.96610142180214,-7.66289334083986,
63.0547491010746));
#62049=CARTESIAN_POINT('Ctrl Pts',(-2.01496393843085,-7.65009544855771,
63.0527173631103));
#62050=CARTESIAN_POINT('Ctrl Pts',(-2.02551299594876,-7.64730914438126,
63.0522792165842));
#62051=CARTESIAN_POINT('Ctrl Pts',(-2.04241015141029,-7.64280871204743,
63.0515781872817));
#62052=CARTESIAN_POINT('Ctrl Pts',(-2.04876191680676,-7.6411084826779,63.0513148421149));
#62053=CARTESIAN_POINT('Ctrl Pts',(-2.06079522574288,-7.63787134477648,
63.0508162728669));
#62054=CARTESIAN_POINT('Ctrl Pts',(-2.06647718619806,-7.6363360115257,63.0505809965113));
#62055=CARTESIAN_POINT('Ctrl Pts',(-2.07934327170509,-7.63284403078826,
63.0500485608063));
#62056=CARTESIAN_POINT('Ctrl Pts',(-2.08652636320027,-7.63088357767284,
63.0497515285542));
#62057=CARTESIAN_POINT('Ctrl Pts',(-2.10496928071966,-7.62582203615739,
63.0489894583112));
#62058=CARTESIAN_POINT('Ctrl Pts',(-2.11622504508396,-7.62270614414721,
63.0485249144724));
#62059=CARTESIAN_POINT('Ctrl Pts',(-2.18136083557474,-7.60451945130429,
63.0458398035159));
#62060=CARTESIAN_POINT('Ctrl Pts',(-2.23508732211326,-7.58890216100012,
63.0436375293616));
#62061=CARTESIAN_POINT('Ctrl Pts',(-3.20395181154837,-7.29608961704842,
63.0041357442748));
#62062=CARTESIAN_POINT('Ctrl Pts',(-4.06132829524855,-6.85590793380312,
62.9739122953314));
#62063=CARTESIAN_POINT('Ctrl Pts',(-4.94136981320677,-6.17984006139831,
62.9341996321728));
#62064=CARTESIAN_POINT('Ctrl Pts',(-5.06053099202144,-6.08264590409552,
62.9285731183903));
#62065=CARTESIAN_POINT('Ctrl Pts',(-5.25598298303272,-5.91350445812071,
62.9187780032969));
#62066=CARTESIAN_POINT('Ctrl Pts',(-5.33381422272958,-5.84339937378735,
62.9147170813021));
#62067=CARTESIAN_POINT('Ctrl Pts',(-5.4233394050688,-5.75948206639975,62.9098235529183));
#62068=CARTESIAN_POINT('Ctrl Pts',(-5.43640919932414,-5.74714702990013,
62.9091034507351));
#62069=CARTESIAN_POINT('Ctrl Pts',(-5.45353595967742,-5.73087240418694,
62.9081521337923));
#62070=CARTESIAN_POINT('Ctrl Pts',(-5.45763095582354,-5.72697278903235,
62.907924092695));
#62071=CARTESIAN_POINT('Ctrl Pts',(-5.46434583781644,-5.72056454569913,
62.9075491989302));
#62072=CARTESIAN_POINT('Ctrl Pts',(-5.46696816190752,-5.71805852308085,
62.9074025540742));
#62073=CARTESIAN_POINT('Ctrl Pts',(-5.4720497004845,-5.71319566248862,62.9071179222737));
#62074=CARTESIAN_POINT('Ctrl Pts',(-5.47450911867186,-5.7108390374761,62.9069799521728));
#62075=CARTESIAN_POINT('Ctrl Pts',(-5.48018816696163,-5.70539030933474,
62.9066608792007));
#62076=CARTESIAN_POINT('Ctrl Pts',(-5.48340670085129,-5.70229707048499,
62.9064796869394));
#62077=CARTESIAN_POINT('Ctrl Pts',(-5.49371482737696,-5.69237343401278,
62.9058982213199));
#62078=CARTESIAN_POINT('Ctrl Pts',(-5.50079426524045,-5.68553254908063,
62.905497128717));
#62079=CARTESIAN_POINT('Ctrl Pts',(-5.56359780145813,-5.62461817598976,
62.9019234905728));
#62080=CARTESIAN_POINT('Ctrl Pts',(-5.6185340923889,-5.56974182785456,62.8986892485283));
#62081=CARTESIAN_POINT('Ctrl Pts',(-5.67534262057534,-5.51129948746517,
62.8952386707162));
#62082=CARTESIAN_POINT('Ctrl Pts',(-5.67803122667456,-5.50852950344129,
62.8950751097641));
#62083=CARTESIAN_POINT('Ctrl Pts',(-5.69261932790654,-5.4934778260836,62.8941862719127));
#62084=CARTESIAN_POINT('Ctrl Pts',(-5.70448093400352,-5.48115961311917,
62.8934585910519));
#62085=CARTESIAN_POINT('Ctrl Pts',(-6.24308788190891,-4.91817715748503,
62.8601935377421));
#62086=CARTESIAN_POINT('Ctrl Pts',(-6.68756186300077,-4.29432807408607,
62.8234329591282));
#62087=CARTESIAN_POINT('Ctrl Pts',(-7.12366409251882,-3.44588679001686,
62.7806759099165));
#62088=CARTESIAN_POINT('Ctrl Pts',(-7.20513390733723,-3.27212120769043,
62.7722276079567));
#62089=CARTESIAN_POINT('Ctrl Pts',(-7.36119616298685,-2.90509018382808,
62.7550709903763));
#62090=CARTESIAN_POINT('Ctrl Pts',(-7.4346810007932,-2.71150969312545,62.7464017701289));
#62091=CARTESIAN_POINT('Ctrl Pts',(-7.51176582974629,-2.48164305530003,
62.7365421595076));
#62092=CARTESIAN_POINT('Ctrl Pts',(-7.52281287159221,-2.44795111802535,
62.735107666452));
#62093=CARTESIAN_POINT('Ctrl Pts',(-7.53691346826921,-2.40394923385608,
62.7332478863943));
#62094=CARTESIAN_POINT('Ctrl Pts',(-7.54017294959365,-2.39370600503139,
62.7328159091998));
#62095=CARTESIAN_POINT('Ctrl Pts',(-7.54543185889127,-2.37706205824172,
62.7321155558766));
#62096=CARTESIAN_POINT('Ctrl Pts',(-7.54744403879132,-2.37066540184412,
62.7318467661456));
#62097=CARTESIAN_POINT('Ctrl Pts',(-7.55128740645077,-2.35839296618936,
62.7313317859079));
#62098=CARTESIAN_POINT('Ctrl Pts',(-7.55311987483477,-2.35251759491574,
62.7310855540372));
#62099=CARTESIAN_POINT('Ctrl Pts',(-7.55727925155486,-2.33912659191759,
62.7305250581618));
#62100=CARTESIAN_POINT('Ctrl Pts',(-7.55960180996909,-2.33160961015453,
62.7302109351507));
#62101=CARTESIAN_POINT('Ctrl Pts',(-7.56678783091468,-2.30822837883013,
62.7292354455046));
#62102=CARTESIAN_POINT('Ctrl Pts',(-7.57161261218675,-2.29235223779771,
62.7285753295871));
#62103=CARTESIAN_POINT('Ctrl Pts',(-7.60785615022647,-2.1717285639451,62.7235768505951));
#62104=CARTESIAN_POINT('Ctrl Pts',(-7.63715052624431,-2.06635262251859,
62.719307344021));
#62105=CARTESIAN_POINT('Ctrl Pts',(-7.68213387188573,-1.89048872157463,
62.7123303695666));
#62106=CARTESIAN_POINT('Ctrl Pts',(-7.69905907623131,-1.82033460666389,
62.7095858501598));
#62107=CARTESIAN_POINT('Ctrl Pts',(-7.84576864342689,-1.17353748112774,
62.6846112895349));
#62108=CARTESIAN_POINT('Ctrl Pts',(-7.91150681219482,-0.584258005828338,
62.6644373132321));
#62109=CARTESIAN_POINT('Ctrl Pts',(-7.91060580399575,0.46049749972319,62.6281482034686));
#62110=CARTESIAN_POINT('Ctrl Pts',(-7.87118945758822,0.913255257185715,
62.6121769119374));
#62111=CARTESIAN_POINT('Ctrl Pts',(-7.78829509126223,1.38823526958181,62.59306333534));
#62112=CARTESIAN_POINT('Ctrl Pts',(-7.78322976338027,1.41635871353383,62.5919225943629));
#62113=CARTESIAN_POINT('Ctrl Pts',(-7.77682397983582,1.45085221115423,62.5905117245318));
#62114=CARTESIAN_POINT('Ctrl Pts',(-7.7756278347614,1.45724916428308,62.5902495764683));
#62115=CARTESIAN_POINT('Ctrl Pts',(-7.77363662771286,1.46782583521355,62.589815310894));
#62116=CARTESIAN_POINT('Ctrl Pts',(-7.77284608319469,1.47200640931157,62.5896434463724));
#62117=CARTESIAN_POINT('Ctrl Pts',(-7.77147477629815,1.47922627612479,62.5893462610977));
#62118=CARTESIAN_POINT('Ctrl Pts',(-7.77089560252826,1.48226586994809,62.5892210300435));
#62119=CARTESIAN_POINT('Ctrl Pts',(-7.76959250367982,1.48908297969179,62.5889399072276));
#62120=CARTESIAN_POINT('Ctrl Pts',(-7.76886760899642,1.49286029736036,62.5887839611286));
#62121=CARTESIAN_POINT('Ctrl Pts',(-7.76693325427897,1.5029003654527,62.5883689885195));
#62122=CARTESIAN_POINT('Ctrl Pts',(-7.76571897624178,1.50916217369208,62.588109691724));
#62123=CARTESIAN_POINT('Ctrl Pts',(-7.76007399132928,1.53808511066186,62.5869097918019));
#62124=CARTESIAN_POINT('Ctrl Pts',(-7.75555169614519,1.56072804379716,62.5859641186058));
#62125=CARTESIAN_POINT('Ctrl Pts',(-7.72029963957853,1.73329641232846,62.5787104949063));
#62126=CARTESIAN_POINT('Ctrl Pts',(-7.68532570494636,1.88231423130748,62.5721798263984));
#62127=CARTESIAN_POINT('Ctrl Pts',(-7.57980728920657,2.27971022146038,62.5542177583192));
#62128=CARTESIAN_POINT('Ctrl Pts',(-7.50139091644964,2.52580288121517,62.5425153881825));
#62129=CARTESIAN_POINT('Ctrl Pts',(-7.18146988446969,3.38248560371697,62.5006625763827));
#62130=CARTESIAN_POINT('Ctrl Pts',(-6.87618048230651,3.96649501451001,62.4703267703));
#62131=CARTESIAN_POINT('Ctrl Pts',(-6.48072918796758,4.5371240398075,62.4409769657717));
#62132=CARTESIAN_POINT('Ctrl Pts',(-6.45901019966186,4.56799000133599,62.4393893559593));
#62133=CARTESIAN_POINT('Ctrl Pts',(-6.36335846992165,4.70187936595585,62.4325026075614));
#62134=CARTESIAN_POINT('Ctrl Pts',(-6.28717385671669,4.80327465678593,62.4272874754914));
#62135=CARTESIAN_POINT('Ctrl Pts',(-6.19891406928886,4.9150410708856,62.4215365002331));
#62136=CARTESIAN_POINT('Ctrl Pts',(-6.18920969064977,4.92725560283619,62.4209079576652));
#62137=CARTESIAN_POINT('Ctrl Pts',(-6.17454211831647,4.94560541293738,62.4199636264361));
#62138=CARTESIAN_POINT('Ctrl Pts',(-6.16960579865482,4.95176206627433,62.4196467753303));
#62139=CARTESIAN_POINT('Ctrl Pts',(-6.16104212414009,4.9624101276146,62.4190987497231));
#62140=CARTESIAN_POINT('Ctrl Pts',(-6.15741905348151,4.96690496487448,62.4188674054333));
#62141=CARTESIAN_POINT('Ctrl Pts',(-6.14988837174393,4.97622674158804,62.4183876066342));
#62142=CARTESIAN_POINT('Ctrl Pts',(-6.14597998966672,4.98105305487234,62.4181391830444));
#62143=CARTESIAN_POINT('Ctrl Pts',(-6.13679599913651,4.99236675164489,62.4175568115567));
#62144=CARTESIAN_POINT('Ctrl Pts',(-6.13151577588889,4.99885038869146,62.417223048027));
#62145=CARTESIAN_POINT('Ctrl Pts',(-6.1143620711042,5.01984551808365,62.4161421966239));
#62146=CARTESIAN_POINT('Ctrl Pts',(-6.10244723556167,5.03432322217302,62.415396764018));
#62147=CARTESIAN_POINT('Ctrl Pts',(-5.78398682149654,5.41849234018072,62.3956130937319));
#62148=CARTESIAN_POINT('Ctrl Pts',(-5.44445470916681,5.75956099169193,62.3780540175138));
#62149=CARTESIAN_POINT('Ctrl Pts',(-4.96336407191662,6.16202252170058,62.3560695677971));
#62150=CARTESIAN_POINT('Ctrl Pts',(-4.84807629523877,6.25313213893486,62.3509848075285));
#62151=CARTESIAN_POINT('Ctrl Pts',(-4.6115995757591,6.42954178443001,62.3408206943881));
#62152=CARTESIAN_POINT('Ctrl Pts',(-4.49041825464805,6.51475264739413,62.3357437288948));
#62153=CARTESIAN_POINT('Ctrl Pts',(-3.96712160646155,6.86117709332413,62.3141275865617));
#62154=CARTESIAN_POINT('Ctrl Pts',(-3.54413330100616,7.08892273531164,62.2974384528388));
#62155=CARTESIAN_POINT('Ctrl Pts',(-3.08724481391446,7.2837587179189,62.2777755919333));
#62156=CARTESIAN_POINT('Ctrl Pts',(-3.07127431262629,7.29050723133412,62.2770862523332));
#62157=CARTESIAN_POINT('Ctrl Pts',(-3.04055341769443,7.30336982970232,62.2757561245411));
#62158=CARTESIAN_POINT('Ctrl Pts',(-3.02580642992365,7.30949186996506,62.2751158084014));
#62159=CARTESIAN_POINT('Ctrl Pts',(-3.00578918095397,7.31773084057933,62.2742440768058));
#62160=CARTESIAN_POINT('Ctrl Pts',(-3.00053494065294,7.31988683827231,62.274015019307));
#62161=CARTESIAN_POINT('Ctrl Pts',(-2.99224898100953,7.32327643536549,62.2736534092099));
#62162=CARTESIAN_POINT('Ctrl Pts',(-2.98921880145346,7.32451381800245,62.273521087041));
#62163=CARTESIAN_POINT('Ctrl Pts',(-2.98337748964284,7.32689490608685,62.2732658501463));
#62164=CARTESIAN_POINT('Ctrl Pts',(-2.98056646495081,7.32803887534106,62.2731429516112));
#62165=CARTESIAN_POINT('Ctrl Pts',(-2.97392781174595,7.33073607721785,62.2728525406626));
#62166=CARTESIAN_POINT('Ctrl Pts',(-2.97009962680472,7.33228792874572,62.2726849433419));
#62167=CARTESIAN_POINT('Ctrl Pts',(-2.95882832237606,7.33684676143428,62.2721910955213));
#62168=CARTESIAN_POINT('Ctrl Pts',(-2.95138188461661,7.33984539425654,62.2718643282391));
#62169=CARTESIAN_POINT('Ctrl Pts',(-2.89220031167994,7.36357281272257,62.2692633722345));
#62170=CARTESIAN_POINT('Ctrl Pts',(-2.8402531463129,7.38376523098079,62.2669565456848));
#62171=CARTESIAN_POINT('Ctrl Pts',(-2.58734664707277,7.47900897408639,62.255627055696));
#62172=CARTESIAN_POINT('Ctrl Pts',(-2.38361528155584,7.54641001514582,62.2462020317969));
#62173=CARTESIAN_POINT('Ctrl Pts',(-1.25651078159794,7.86909604488385,62.1934390942523));
#62174=CARTESIAN_POINT('Ctrl Pts',(-0.294949493266388,7.96338125329544,
62.1475032689685));
#62175=CARTESIAN_POINT('Ctrl Pts',(0.715692789689113,7.87875732724936,62.1059731915442));
#62176=CARTESIAN_POINT('Ctrl Pts',(0.771235192753037,7.87351444020248,62.1037077037033));
#62177=CARTESIAN_POINT('Ctrl Pts',(0.838321498414512,7.86646516463718,62.1009913316676));
#62178=CARTESIAN_POINT('Ctrl Pts',(0.849922035340624,7.86522025480242,62.1005223402112));
#62179=CARTESIAN_POINT('Ctrl Pts',(0.868917657086711,7.863139226174,62.0997555528502));
#62180=CARTESIAN_POINT('Ctrl Pts',(0.876314370984281,7.86231832913185,62.0994572653027));
#62181=CARTESIAN_POINT('Ctrl Pts',(0.889558426021794,7.8608295646086,62.0989236926657));
#62182=CARTESIAN_POINT('Ctrl Pts',(0.895406195920845,7.8601656077742,62.0986882813291));
#62183=CARTESIAN_POINT('Ctrl Pts',(0.907787966926001,7.85874578233914,62.0981902171344));
#62184=CARTESIAN_POINT('Ctrl Pts',(0.914321779268518,7.85798828890454,62.0979276170184));
#62185=CARTESIAN_POINT('Ctrl Pts',(0.931700969017612,7.85595147406421,62.097229730652));
#62186=CARTESIAN_POINT('Ctrl Pts',(0.942544672888111,7.85465784101333,62.0967949076778));
#62187=CARTESIAN_POINT('Ctrl Pts',(0.992795636039444,7.84855743805343,62.0947827476503));
#62188=CARTESIAN_POINT('Ctrl Pts',(1.03216936823762,7.84347649250509,62.0932142942121));
#62189=CARTESIAN_POINT('Ctrl Pts',(1.32398045152804,7.80358459984253,62.0816485923894));
#62190=CARTESIAN_POINT('Ctrl Pts',(1.57465177610998,7.75688997567654,62.0720464924182));
#62191=CARTESIAN_POINT('Ctrl Pts',(2.08916802591955,7.63507126680689,62.0527788769906));
#62192=CARTESIAN_POINT('Ctrl Pts',(2.35223901295436,7.55816889891921,62.0431763295241));
#62193=CARTESIAN_POINT('Ctrl Pts',(2.84348983250134,7.38642332603823,62.0252229098963));
#62194=CARTESIAN_POINT('Ctrl Pts',(3.07225021711206,7.29424171940297,62.0168508495463));
#62195=CARTESIAN_POINT('Ctrl Pts',(3.66538962775336,7.02236844118222,61.9944148772895));
#62196=CARTESIAN_POINT('Ctrl Pts',(4.02084619549653,6.82506233614114,61.9802175514428));
#62197=CARTESIAN_POINT('Ctrl Pts',(4.41322133127512,6.56593744115765,61.9619476235685));
#62198=CARTESIAN_POINT('Ctrl Pts',(4.46645108020621,6.52984466277824,61.959409543361));
#62199=CARTESIAN_POINT('Ctrl Pts',(4.52671311230428,6.48790200643167,61.9564604434949));
#62200=CARTESIAN_POINT('Ctrl Pts',(4.53418372722666,6.48268323864325,61.9560935040183));
#62201=CARTESIAN_POINT('Ctrl Pts',(4.54512042996369,6.47501500313232,61.9555543213263));
#62202=CARTESIAN_POINT('Ctrl Pts',(4.54859361388196,6.47257561943291,61.9553827964435));
#62203=CARTESIAN_POINT('Ctrl Pts',(4.55475263369076,6.46824243872364,61.9550781017596));
#62204=CARTESIAN_POINT('Ctrl Pts',(4.55743925836043,6.46634975906109,61.954945012276));
#62205=CARTESIAN_POINT('Ctrl Pts',(4.56297372485485,6.46244566261971,61.9546704768296));
#62206=CARTESIAN_POINT('Ctrl Pts',(4.56582140753901,6.46043404349387,61.954529015943));
#62207=CARTESIAN_POINT('Ctrl Pts',(4.57319264049173,6.45521965491716,61.9541623206839));
#62208=CARTESIAN_POINT('Ctrl Pts',(4.57771414851098,6.45201401846675,61.9539368793342));
#62209=CARTESIAN_POINT('Ctrl Pts',(4.5875557230671,6.44502103448786,61.9534450742805));
#62210=CARTESIAN_POINT('Ctrl Pts',(4.59287447215981,6.44123184877868,61.9531785790539));
#62211=CARTESIAN_POINT('Ctrl Pts',(4.60831535912621,6.43020259614218,61.9524028785108));
#62212=CARTESIAN_POINT('Ctrl Pts',(4.61842507221944,6.42294525319064,61.951892450943));
#62213=CARTESIAN_POINT('Ctrl Pts',(4.7200848879916,6.3496037824493,61.9467344238851));
#62214=CARTESIAN_POINT('Ctrl Pts',(4.81022346599078,6.28159354561954,61.9419535905088));
#62215=CARTESIAN_POINT('Ctrl Pts',(5.07914361004057,6.06950839979982,61.9271325609015));
#62216=CARTESIAN_POINT('Ctrl Pts',(5.25313147016896,5.91956330116238,61.9167724235427));
#62217=CARTESIAN_POINT('Ctrl Pts',(6.09272473000039,5.12979146979673,61.8638008903368));
#62218=CARTESIAN_POINT('Ctrl Pts',(6.64945863589698,4.38424218008588,61.8198021055462));
#62219=CARTESIAN_POINT('Ctrl Pts',(7.07115389512443,3.54723703613978,61.7813355079288));
#62220=CARTESIAN_POINT('Ctrl Pts',(7.07727501766205,3.53500867410727,61.7807753927345));
#62221=CARTESIAN_POINT('Ctrl Pts',(7.10473691532622,3.47978993010312,61.7782545111206));
#62222=CARTESIAN_POINT('Ctrl Pts',(7.12571811929919,3.4366213039811,61.7763066474846));
#62223=CARTESIAN_POINT('Ctrl Pts',(7.15106927171243,3.38323109207717,61.7739252368066));
#62224=CARTESIAN_POINT('Ctrl Pts',(7.15581200046395,3.37318824950241,61.7734784846607));
#62225=CARTESIAN_POINT('Ctrl Pts',(7.16363659701015,3.35652871034776,61.7727393658837));
#62226=CARTESIAN_POINT('Ctrl Pts',(7.16673047708897,3.34991769250445,61.7724465749429));
#62227=CARTESIAN_POINT('Ctrl Pts',(7.17231511774406,3.33794125818065,61.7719170862362));
#62228=CARTESIAN_POINT('Ctrl Pts',(7.17480901655331,3.33257731605293,61.771680277911));
#62229=CARTESIAN_POINT('Ctrl Pts',(7.18014263837985,3.32107188633906,61.7711730528728));
#62230=CARTESIAN_POINT('Ctrl Pts',(7.18298050430277,3.31492954024937,61.7709027016555));
#62231=CARTESIAN_POINT('Ctrl Pts',(7.19066711075665,3.29823624603744,61.7701691444488));
#62232=CARTESIAN_POINT('Ctrl Pts',(7.19550051601744,3.28767823211026,61.7697064774336));
#62233=CARTESIAN_POINT('Ctrl Pts',(7.21964660206181,3.23462559028851,61.7673880529819));
#62234=CARTESIAN_POINT('Ctrl Pts',(7.23860635575607,3.19197084738868,61.7655446645335));
#62235=CARTESIAN_POINT('Ctrl Pts',(7.40097152010585,2.81780183194893,61.7495497861065));
#62236=CARTESIAN_POINT('Ctrl Pts',(7.52190081977087,2.4769794522955,61.7362055551303));
#62237=CARTESIAN_POINT('Ctrl Pts',(7.75854600509628,1.63011444920188,61.7049235016786));
#62238=CARTESIAN_POINT('Ctrl Pts',(7.8486176987374,1.11869924012562,61.6876223899349));
#62239=CARTESIAN_POINT('Ctrl Pts',(7.91363890963849,0.266949203041437,61.6575337902451));
#62240=CARTESIAN_POINT('Ctrl Pts',(7.91783427997919,-0.0695485862649099,
61.6452876338838));
#62241=CARTESIAN_POINT('Ctrl Pts',(7.89938993817325,-0.429101766765873,
61.6309654440322));
#62242=CARTESIAN_POINT('Ctrl Pts',(7.89806052012822,-0.45291248906759,61.6300115908312));
#62243=CARTESIAN_POINT('Ctrl Pts',(7.89615569121186,-0.484465230673838,
61.6287407452992));
#62244=CARTESIAN_POINT('Ctrl Pts',(7.89567650730703,-0.492213115333169,
61.6284281371634));
#62245=CARTESIAN_POINT('Ctrl Pts',(7.89491426804264,-0.504250113418869,
61.6279416350182));
#62246=CARTESIAN_POINT('Ctrl Pts',(7.89463911856142,-0.508539737088017,
61.6277680947527));
#62247=CARTESIAN_POINT('Ctrl Pts',(7.89410315837529,-0.516790171154996,
61.627434000733));
#62248=CARTESIAN_POINT('Ctrl Pts',(7.89384286242484,-0.520751014724079,
61.6272734698185));
#62249=CARTESIAN_POINT('Ctrl Pts',(7.89324349049632,-0.529767757479902,
61.6269077094448));
#62250=CARTESIAN_POINT('Ctrl Pts',(7.89290253786219,-0.53482352674502,61.6267023977075));
#62251=CARTESIAN_POINT('Ctrl Pts',(7.89218557899021,-0.54530483649764,61.626276292712));
#62252=CARTESIAN_POINT('Ctrl Pts',(7.89180883506443,-0.550730322857615,
61.6260554675534));
#62253=CARTESIAN_POINT('Ctrl Pts',(7.8908310532008,-0.56460431134283,61.6254901216285));
#62254=CARTESIAN_POINT('Ctrl Pts',(7.89022204238863,-0.573052231089277,
61.6251452597735));
#62255=CARTESIAN_POINT('Ctrl Pts',(7.8783849615531,-0.733654064097284,61.6185775413799));
#62256=CARTESIAN_POINT('Ctrl Pts',(7.86277164219871,-0.88544688873738,61.6121723347128));
#62257=CARTESIAN_POINT('Ctrl Pts',(7.8174038127089,-1.2286653070441,61.5973655778602));
#62258=CARTESIAN_POINT('Ctrl Pts',(7.78498756843565,-1.41964264024855,61.5888966547751));
#62259=CARTESIAN_POINT('Ctrl Pts',(7.65721737587657,-2.03462950518168,61.5611886559831));
#62260=CARTESIAN_POINT('Ctrl Pts',(7.53393730256748,-2.45204119837214,61.5417461119891));
#62261=CARTESIAN_POINT('Ctrl Pts',(7.23245424436947,-3.23043532558423,61.5054845859477));
#62262=CARTESIAN_POINT('Ctrl Pts',(7.0597814956763,-3.59216275943425,61.4886267024257));
#62263=CARTESIAN_POINT('Ctrl Pts',(6.84534745355643,-3.96560970148236,61.471190418263));
#62264=CARTESIAN_POINT('Ctrl Pts',(6.8300837192045,-3.9918414886753,61.46996522562));
#62265=CARTESIAN_POINT('Ctrl Pts',(6.80851735931988,-4.02841893095854,61.4682560407387));
#62266=CARTESIAN_POINT('Ctrl Pts',(6.80234141322475,-4.03883882006926,61.467769052098));
#62267=CARTESIAN_POINT('Ctrl Pts',(6.79160764834154,-4.05685407833064,61.4669269115225));
#62268=CARTESIAN_POINT('Ctrl Pts',(6.78706096483878,-4.06445604255309,61.4665714973881));
#62269=CARTESIAN_POINT('Ctrl Pts',(6.77761519835882,-4.08018913024572,61.4658358117663));
#62270=CARTESIAN_POINT('Ctrl Pts',(6.77271422436892,-4.08831911073927,61.4654555848434));
#62271=CARTESIAN_POINT('Ctrl Pts',(6.76126089847395,-4.10724134523986,61.4645704642823));
#62272=CARTESIAN_POINT('Ctrl Pts',(6.7546973140779,-4.11802678496741,61.4640658379744));
#62273=CARTESIAN_POINT('Ctrl Pts',(6.73364692585998,-4.15243155449798,61.4624557287968));
#62274=CARTESIAN_POINT('Ctrl Pts',(6.71906179407703,-4.17599058397504,61.4613526046534));
#62275=CARTESIAN_POINT('Ctrl Pts',(6.68502442888113,-4.23033038742051,61.4588067621071));
#62276=CARTESIAN_POINT('Ctrl Pts',(6.6654828140784,-4.2610545275215,61.4573662430706));
#62277=CARTESIAN_POINT('Ctrl Pts',(6.53569569642452,-4.46203353058331,61.4479353339613));
#62278=CARTESIAN_POINT('Ctrl Pts',(6.41914686498998,-4.62813351139385,61.4401064211871));
#62279=CARTESIAN_POINT('Ctrl Pts',(6.21085389210602,-4.9019538489769,61.4270716921437));
#62280=CARTESIAN_POINT('Ctrl Pts',(6.12237408811986,-5.01202498323201,61.4217934426387));
#62281=CARTESIAN_POINT('Ctrl Pts',(5.9613529236291,-5.20170860658311,61.4125874472854));
#62282=CARTESIAN_POINT('Ctrl Pts',(5.89004438212564,-5.28231755001206,61.4086379537091));
#62283=CARTESIAN_POINT('Ctrl Pts',(5.47865865400861,-5.72866665693717,61.3864803044406));
#62284=CARTESIAN_POINT('Ctrl Pts',(5.10620971446954,-6.06299464460321,61.3688388309151));
#62285=CARTESIAN_POINT('Ctrl Pts',(4.59390058809967,-6.44197263205721,61.3448907802586));
#62286=CARTESIAN_POINT('Ctrl Pts',(4.48092544231186,-6.52106117377738,61.3396218674391));
#62287=CARTESIAN_POINT('Ctrl Pts',(4.31400961149238,-6.63152476371396,61.3317793179069));
#62288=CARTESIAN_POINT('Ctrl Pts',(4.26167106018734,-6.66528012208291,61.3293121390376));
#62289=CARTESIAN_POINT('Ctrl Pts',(4.19985257758221,-6.70412369542239,61.3263829026868));
#62290=CARTESIAN_POINT('Ctrl Pts',(4.19075315020912,-6.70981551380764,61.3259513490234));
#62291=CARTESIAN_POINT('Ctrl Pts',(4.17693855835726,-6.7184176695386,61.3252955542655));
#62292=CARTESIAN_POINT('Ctrl Pts',(4.17223184937826,-6.7213416144,61.3250720129005));
#62293=CARTESIAN_POINT('Ctrl Pts',(4.16391141627536,-6.72649840273857,61.3246766429593));
#62294=CARTESIAN_POINT('Ctrl Pts',(4.16029895481449,-6.72873328726129,61.324504920477));
#62295=CARTESIAN_POINT('Ctrl Pts',(4.15270665852673,-6.73342188400935,61.3241438706768));
#62296=CARTESIAN_POINT('Ctrl Pts',(4.14872644612811,-6.73587497916082,61.323954511186));
#62297=CARTESIAN_POINT('Ctrl Pts',(4.14060388837366,-6.74087116521065,61.3235679082892));
#62298=CARTESIAN_POINT('Ctrl Pts',(4.13646136991116,-6.74341396930759,61.3233706498956));
#62299=CARTESIAN_POINT('Ctrl Pts',(4.12627810102043,-6.74965185601603,61.3228855156285));
#62300=CARTESIAN_POINT('Ctrl Pts',(4.12023473573557,-6.75334264392982,61.3225974113118));
#62301=CARTESIAN_POINT('Ctrl Pts',(4.1036123364545,-6.76346361382753,61.3218044147711));
#62302=CARTESIAN_POINT('Ctrl Pts',(4.09302318346262,-6.7698770653802,61.3212986213026));
#62303=CARTESIAN_POINT('Ctrl Pts',(3.79354731916229,-6.95029885664525,61.3069754204391));
#62304=CARTESIAN_POINT('Ctrl Pts',(3.4938958673471,-7.10565014139569,61.2920483404002));
#62305=CARTESIAN_POINT('Ctrl Pts',(2.38330367620491,-7.59417225138492,61.236897401619));
#62306=CARTESIAN_POINT('Ctrl Pts',(1.52798919228387,-7.8113695664866,61.1956596880325));
#62307=CARTESIAN_POINT('Ctrl Pts',(0.599642799317534,-7.88843294471139,
61.1574956783516));
#62308=CARTESIAN_POINT('Ctrl Pts',(0.544786388673252,-7.89241115018974,
61.1552606651854));
#62309=CARTESIAN_POINT('Ctrl Pts',(0.478245123481413,-7.89653967116389,
61.1525735656734));
#62310=CARTESIAN_POINT('Ctrl Pts',(0.466596437978362,-7.8972365383096,61.1521040527859));
#62311=CARTESIAN_POINT('Ctrl Pts',(0.447484251047435,-7.89833746498598,
61.1513351679276));
#62312=CARTESIAN_POINT('Ctrl Pts',(0.440021663352057,-7.89875672507535,
61.1510353105899));
#62313=CARTESIAN_POINT('Ctrl Pts',(0.426636542794986,-7.89948969458422,
61.1504981267411));
#62314=CARTESIAN_POINT('Ctrl Pts',(0.420714235242946,-7.8998073208754,61.1502606752044));
#62315=CARTESIAN_POINT('Ctrl Pts',(0.408151341442363,-7.90046692902595,
61.1497574552636));
#62316=CARTESIAN_POINT('Ctrl Pts',(0.401510667781274,-7.9008071991472,61.1494917417648));
#62317=CARTESIAN_POINT('Ctrl Pts',(0.383794417911599,-7.90169259146159,
61.1487836205281));
#62318=CARTESIAN_POINT('Ctrl Pts',(0.372718092706051,-7.90222280057098,
61.1483416900395));
#62319=CARTESIAN_POINT('Ctrl Pts',(0.320846568486834,-7.90459651862682,
61.1462757733571));
#62320=CARTESIAN_POINT('Ctrl Pts',(0.280038251950287,-7.9061474363438,61.1446611602098));
#62321=CARTESIAN_POINT('Ctrl Pts',(-0.0259326993814343,-7.91540387151853,
61.132633307875));
#62322=CARTESIAN_POINT('Ctrl Pts',(-0.291330886227619,-7.9100842323467,
61.1226483646982));
#62323=CARTESIAN_POINT('Ctrl Pts',(-0.78599656850133,-7.87523345576896,
61.1046326483856));
#62324=CARTESIAN_POINT('Ctrl Pts',(-1.01520338926843,-7.84897834297204,
61.0965241833831));
#62325=CARTESIAN_POINT('Ctrl Pts',(-1.31194357531869,-7.80176945752871,
61.086150030326));
#62326=CARTESIAN_POINT('Ctrl Pts',(-1.38079627222556,-7.78987832868687,
61.083751286987));
#62327=CARTESIAN_POINT('Ctrl Pts',(-1.50684733463846,-7.76638507354082,
61.0793660548154));
#62328=CARTESIAN_POINT('Ctrl Pts',(-1.56409199861762,-7.75505913973456,
61.0773769175412));
#62329=CARTESIAN_POINT('Ctrl Pts',(-1.66999878403781,-7.73288498133223,
61.0736954606509));
#62330=CARTESIAN_POINT('Ctrl Pts',(-1.71869369956481,-7.72220810733611,
61.0720022032264));
#62331=CARTESIAN_POINT('Ctrl Pts',(-1.80941574484892,-7.7014157102322,61.0688426481332));
#62332=CARTESIAN_POINT('Ctrl Pts',(-1.85146715041356,-7.69141460794823,
61.0673761557768));
#62333=CARTESIAN_POINT('Ctrl Pts',(-1.93020728305919,-7.67200464370164,
61.06462383519));
#62334=CARTESIAN_POINT('Ctrl Pts',(-1.96691449163024,-7.66267595473265,
61.063338147956));
#62335=CARTESIAN_POINT('Ctrl Pts',(-2.03591901926335,-7.64461078701827,
61.0609144736932));
#62336=CARTESIAN_POINT('Ctrl Pts',(-2.06823065595581,-7.63593231283413,
61.0597767729488));
#62337=CARTESIAN_POINT('Ctrl Pts',(-2.12918638008594,-7.61914513125845,
61.0576238848505));
#62338=CARTESIAN_POINT('Ctrl Pts',(-2.15784164755236,-7.61107920012856,
61.0566090335344));
#62339=CARTESIAN_POINT('Ctrl Pts',(-2.43408746857354,-7.53163560743304,
61.0467938395871));
#62340=CARTESIAN_POINT('Ctrl Pts',(-2.67808774422027,-7.44836573925284,
61.0378818421101));
#62341=CARTESIAN_POINT('Ctrl Pts',(-3.0552868471976,-7.2987048299721,61.0231617172854));
#62342=CARTESIAN_POINT('Ctrl Pts',(-3.19142717328143,-7.24021122860647,
61.0176461662436));
#62343=CARTESIAN_POINT('Ctrl Pts',(-3.39392595351592,-7.14638501419299,
61.0090245442973));
#62344=CARTESIAN_POINT('Ctrl Pts',(-3.46155896136129,-7.11387103004195,
61.0060729006649));
#62345=CARTESIAN_POINT('Ctrl Pts',(-3.53721131963036,-7.07616754691953,
61.0026788096852));
#62346=CARTESIAN_POINT('Ctrl Pts',(-3.54569782790225,-7.0719189746135,61.0022967459154));
#62347=CARTESIAN_POINT('Ctrl Pts',(-3.55801694570244,-7.06572394674907,
61.0017401864703));
#62348=CARTESIAN_POINT('Ctrl Pts',(-3.56185567451262,-7.06378960837373,
61.0015664826737));
#62349=CARTESIAN_POINT('Ctrl Pts',(-3.5686286278187,-7.06036978727621,61.0012595141639));
#62350=CARTESIAN_POINT('Ctrl Pts',(-3.57156349981377,-7.05888560489828,
61.0011263350456));
#62351=CARTESIAN_POINT('Ctrl Pts',(-3.57721539444195,-7.05602298069528,
61.000869549538));
#62352=CARTESIAN_POINT('Ctrl Pts',(-3.5799325478822,-7.05464479863411,61.0007459603149));
#62353=CARTESIAN_POINT('Ctrl Pts',(-3.58575297914487,-7.05168835767806,
61.0004809215841));
#62354=CARTESIAN_POINT('Ctrl Pts',(-3.58885601151714,-7.05010961969962,
61.0003394407779));
#62355=CARTESIAN_POINT('Ctrl Pts',(-3.6006589778881,-7.04409478165093,60.99980060489));
#62356=CARTESIAN_POINT('Ctrl Pts',(-3.60935170456554,-7.03964463868951,
60.9994023382798));
#62357=CARTESIAN_POINT('Ctrl Pts',(-3.72039732736456,-6.98253633938219,
60.9942967109243));
#62358=CARTESIAN_POINT('Ctrl Pts',(-3.82159292967034,-6.92766880547784,
60.9894488300577));
#62359=CARTESIAN_POINT('Ctrl Pts',(-4.08079200474085,-6.77972539832798,
60.9765967075683));
#62360=CARTESIAN_POINT('Ctrl Pts',(-4.23681802991186,-6.68333047761783,
60.9684301894143));
#62361=CARTESIAN_POINT('Ctrl Pts',(-4.97848709529102,-6.18870328909454,
60.9280128893947));
#62362=CARTESIAN_POINT('Ctrl Pts',(-5.51232280680041,-5.718384683933,60.8942861970079));
#62363=CARTESIAN_POINT('Ctrl Pts',(-6.1486255251246,-4.98471799443466,60.8520624192308));
#62364=CARTESIAN_POINT('Ctrl Pts',(-6.31084834836532,-4.77767940018079,
60.8410147605737));
#62365=CARTESIAN_POINT('Ctrl Pts',(-6.47408421270489,-4.54648873525531,
60.8295777797758));
#62366=CARTESIAN_POINT('Ctrl Pts',(-6.48563205509533,-4.53000033851557,
60.8287667725967));
#62367=CARTESIAN_POINT('Ctrl Pts',(-6.50155865463927,-4.50707406987797,
60.8276455375746));
#62368=CARTESIAN_POINT('Ctrl Pts',(-6.5059909809571,-4.50067361260898,60.8273332075242));
#62369=CARTESIAN_POINT('Ctrl Pts',(-6.51359638802572,-4.48965638735665,
60.8267967733307));
#62370=CARTESIAN_POINT('Ctrl Pts',(-6.51677402244096,-4.48504277830818,
60.8265724909336));
#62371=CARTESIAN_POINT('Ctrl Pts',(-6.52297403551785,-4.47602047617868,
60.8261345828073));
#62372=CARTESIAN_POINT('Ctrl Pts',(-6.52599685205926,-4.47161208718912,
60.8259209399952));
#62373=CARTESIAN_POINT('Ctrl Pts',(-6.53326003169092,-4.46099662257564,
60.8254072618057));
#62374=CARTESIAN_POINT('Ctrl Pts',(-6.53749602348712,-4.45478655511185,
60.8251073970829));
#62375=CARTESIAN_POINT('Ctrl Pts',(-6.55033035386074,-4.43591338286539,
60.824198001215));
#62376=CARTESIAN_POINT('Ctrl Pts',(-6.55890082210556,-4.42323131819342,
60.8235895550157));
#62377=CARTESIAN_POINT('Ctrl Pts',(-6.64103650996505,-4.30092823208214,
60.817746997335));
#62378=CARTESIAN_POINT('Ctrl Pts',(-6.71188559917261,-4.18950395641703,
60.8126187922149));
#62379=CARTESIAN_POINT('Ctrl Pts',(-6.96513637538515,-3.76828972021598,
60.7938986349276));
#62380=CARTESIAN_POINT('Ctrl Pts',(-7.12915331211552,-3.44794607440122,
60.7809916455826));
#62381=CARTESIAN_POINT('Ctrl Pts',(-7.48001179611938,-2.62966324681593,
60.7499704847939));
#62382=CARTESIAN_POINT('Ctrl Pts',(-7.63955181009023,-2.12200304466565,
60.7324306262417));
#62383=CARTESIAN_POINT('Ctrl Pts',(-7.75159859056179,-1.58023555265639,
60.7125347170563));
#62384=CARTESIAN_POINT('Ctrl Pts',(-7.75605225567748,-1.55822928629906,
60.7117244147999));
#62385=CARTESIAN_POINT('Ctrl Pts',(-7.77264979963041,-1.4743838186034,60.7086280011297));
#62386=CARTESIAN_POINT('Ctrl Pts',(-7.78414811008889,-1.41242008826183,
60.7063208648015));
#62387=CARTESIAN_POINT('Ctrl Pts',(-7.82304913145525,-1.18785978239925,
60.6978714139187));
#62388=CARTESIAN_POINT('Ctrl Pts',(-7.84610574756365,-1.02456182892599,
60.6915605515287));
#62389=CARTESIAN_POINT('Ctrl Pts',(-7.86530173113506,-0.849166449993318,
60.6844939711693));
#62390=CARTESIAN_POINT('Ctrl Pts',(-7.86653577003126,-0.837657422644243,
60.6840289553866));
#62391=CARTESIAN_POINT('Ctrl Pts',(-7.86820691086274,-0.821742423902092,
60.6833840392698));
#62392=CARTESIAN_POINT('Ctrl Pts',(-7.86866558248535,-0.817338702194046,
60.6832053898832));
#62393=CARTESIAN_POINT('Ctrl Pts',(-7.86944910333665,-0.809754303624965,
60.682897365482));
#62394=CARTESIAN_POINT('Ctrl Pts',(-7.86977572177094,-0.806573810145947,
60.6827680930296));
#62395=CARTESIAN_POINT('Ctrl Pts',(-7.87042846414609,-0.800179495977349,
60.682507986923));
#62396=CARTESIAN_POINT('Ctrl Pts',(-7.87075454786571,-0.796965671917656,
60.6823771509921));
#62397=CARTESIAN_POINT('Ctrl Pts',(-7.87141047288421,-0.790461323367632,
60.6821121456393));
#62398=CARTESIAN_POINT('Ctrl Pts',(-7.87174021951579,-0.787170790086976,
60.68197797085));
#62399=CARTESIAN_POINT('Ctrl Pts',(-7.87249334917187,-0.779607531207589,
60.6816693218714));
#62400=CARTESIAN_POINT('Ctrl Pts',(-7.8729153168618,-0.77533466894218,60.6814947676637));
#62401=CARTESIAN_POINT('Ctrl Pts',(-7.87399020034538,-0.764358998692847,
60.6810459253921));
#62402=CARTESIAN_POINT('Ctrl Pts',(-7.87463803491731,-0.757655708433056,
60.6807713526263));
#62403=CARTESIAN_POINT('Ctrl Pts',(-7.88013531242262,-0.700005410187424,
60.6784061558521));
#62404=CARTESIAN_POINT('Ctrl Pts',(-7.88449873614315,-0.649014312055114,
60.6762887246058));
#62405=CARTESIAN_POINT('Ctrl Pts',(-7.90336745621056,-0.400106311807902,
60.6658409886551));
#62406=CARTESIAN_POINT('Ctrl Pts',(-7.91091585282024,-0.201746000078963,
60.6571719939765));
#62407=CARTESIAN_POINT('Ctrl Pts',(-7.9109993003797,-0.00332706956333997,
60.6482969704864));
#62408=CARTESIAN_POINT('',(-7.91186981885086,-0.00113476366102863,58.6438367629128));
#62409=CARTESIAN_POINT('Ctrl Pts',(-7.91099918378876,-0.00359361845736577,
60.642331508237));
#62410=CARTESIAN_POINT('Ctrl Pts',(-7.91108682626939,0.189342721609203,
60.6345315316643));
#62411=CARTESIAN_POINT('Ctrl Pts',(-7.90411218664149,0.382554960580305,
60.6267315550916));
#62412=CARTESIAN_POINT('Ctrl Pts',(-7.89004104426854,0.575476602267969,
60.6189315785189));
#62413=CARTESIAN_POINT('Ctrl Pts',(-7.87598390482651,0.768206257523253,
60.6111393641116));
#62414=CARTESIAN_POINT('Ctrl Pts',(-7.85484434960438,0.960645539965939,
60.6033471497042));
#62415=CARTESIAN_POINT('Ctrl Pts',(-7.82664014023985,1.15222615626722,60.5955549352968));
#62416=CARTESIAN_POINT('Ctrl Pts',(-7.79845839522772,1.34365418064785,60.5877689273052));
#62417=CARTESIAN_POINT('Ctrl Pts',(-7.76322325286589,1.53422455125414,60.5799829193136));
#62418=CARTESIAN_POINT('Ctrl Pts',(-7.72100442904379,1.72337216139934,60.572196911322));
#62419=CARTESIAN_POINT('Ctrl Pts',(-7.67881085024431,1.91240666949041,60.564415559025));
#62420=CARTESIAN_POINT('Ctrl Pts',(-7.62964198436513,2.10001976589426,60.5566342067279));
#62421=CARTESIAN_POINT('Ctrl Pts',(-7.57361898674068,2.28565448913021,60.5488528544309));
#62422=CARTESIAN_POINT('Ctrl Pts',(-7.51628015115184,2.47564930066383,60.5408887379263));
#62423=CARTESIAN_POINT('Ctrl Pts',(-7.45176130606158,2.66357128600721,60.5329246214216));
#62424=CARTESIAN_POINT('Ctrl Pts',(-7.38024728606134,2.84883677956182,60.524960504917));
#62425=CARTESIAN_POINT('Ctrl Pts',(-7.31040575065093,3.02976950475864,60.5171826436687));
#62426=CARTESIAN_POINT('Ctrl Pts',(-7.23389272366826,3.20816826221708,60.5094047824205));
#62427=CARTESIAN_POINT('Ctrl Pts',(-7.15093003176425,3.38350715690276,60.5016269211722));
#62428=CARTESIAN_POINT('Ctrl Pts',(-7.06796419635235,3.55885269528798,60.4938487652159));
#62429=CARTESIAN_POINT('Ctrl Pts',(-6.97854836096569,3.73113781844891,60.4860706092596));
#62430=CARTESIAN_POINT('Ctrl Pts',(-6.88295140546018,3.89985909361783,60.4782924533033));
#62431=CARTESIAN_POINT('Ctrl Pts',(-6.78733364526376,4.06861708746637,60.470512604593));
#62432=CARTESIAN_POINT('Ctrl Pts',(-6.68553226124847,4.23380937952657,60.4627327558827));
#62433=CARTESIAN_POINT('Ctrl Pts',(-6.57786080067544,4.39495941812179,60.4549529071724));
#62434=CARTESIAN_POINT('Ctrl Pts',(-6.46571370897935,4.56280805748254,60.4468496697681));
#62435=CARTESIAN_POINT('Ctrl Pts',(-6.34719832698105,4.72627084304187,60.4387464323637));
#62436=CARTESIAN_POINT('Ctrl Pts',(-6.22271668245228,4.88484575907265,60.4306431949594));
#62437=CARTESIAN_POINT('Ctrl Pts',(-6.10302813294028,5.03731483803252,60.4228519681086));
#62438=CARTESIAN_POINT('Ctrl Pts',(-5.97782445659388,5.18526518610947,60.4150607412579));
#62439=CARTESIAN_POINT('Ctrl Pts',(-5.84750177568918,5.32828715285802,60.4072695144071));
#62440=CARTESIAN_POINT('Ctrl Pts',(-5.71709605754416,5.47140024840582,60.399473323248));
#62441=CARTESIAN_POINT('Ctrl Pts',(-5.58156508413715,5.60957845364282,60.3916771320889));
#62442=CARTESIAN_POINT('Ctrl Pts',(-5.44133979553639,5.74245089047456,60.3838809409298));
#62443=CARTESIAN_POINT('Ctrl Pts',(-5.30094395465509,5.87548493650923,60.3760752674712));
#62444=CARTESIAN_POINT('Ctrl Pts',(-5.15584266786037,6.00320010079997,60.3682695940125));
#62445=CARTESIAN_POINT('Ctrl Pts',(-5.00649830228262,6.12526699411881,60.3604639205539));
#62446=CARTESIAN_POINT('Ctrl Pts',(-4.98896078366883,6.13960131738186,60.3595472998094));
#62447=CARTESIAN_POINT('Ctrl Pts',(-4.97136478452658,6.15385780243507,60.3586306790648));
#62448=CARTESIAN_POINT('Ctrl Pts',(-4.95371107754146,6.16803595646483,60.3577140583202));
#62449=CARTESIAN_POINT('Ctrl Pts',(-4.80134554005385,6.29040470661727,60.3498028919835));
#62450=CARTESIAN_POINT('Ctrl Pts',(-4.64423832116536,6.40728886446966,60.3418917256468));
#62451=CARTESIAN_POINT('Ctrl Pts',(-4.48282075010993,6.51830032465396,60.3339805593101));
#62452=CARTESIAN_POINT('Ctrl Pts',(-4.32157815059095,6.6291914519301,60.3260779684272));
#62453=CARTESIAN_POINT('Ctrl Pts',(-4.15603478696332,6.73422236766679,60.3181753775443));
#62454=CARTESIAN_POINT('Ctrl Pts',(-3.98665579704222,6.83304445733449,60.3102727866614));
#62455=CARTESIAN_POINT('Ctrl Pts',(-3.81742896711696,6.93177777112297,60.3023772949955));
#62456=CARTESIAN_POINT('Ctrl Pts',(-3.64437367100339,7.02431319731362,60.2944818033296));
#62457=CARTESIAN_POINT('Ctrl Pts',(-3.46798506006037,7.11034462056503,60.2865863116636));
#62458=CARTESIAN_POINT('Ctrl Pts',(-3.29172217365904,7.19631472318354,60.2786964476687));
#62459=CARTESIAN_POINT('Ctrl Pts',(-3.11213101467736,7.27578990853649,60.2708065836738));
#62460=CARTESIAN_POINT('Ctrl Pts',(-2.92973268421597,7.34850919568294,60.2629167196788));
#62461=CARTESIAN_POINT('Ctrl Pts',(-2.74743052171536,7.42119014220677,60.2550310155473));
#62462=CARTESIAN_POINT('Ctrl Pts',(-2.56232445649966,7.48712216087777,60.2471453114157));
#62463=CARTESIAN_POINT('Ctrl Pts',(-2.37495724374363,7.54609164338664,60.2392596072841));
#62464=CARTESIAN_POINT('Ctrl Pts',(-2.18765406241649,7.60504097348906,60.2313765980365));
#62465=CARTESIAN_POINT('Ctrl Pts',(-1.99809160216031,7.65703240626555,60.223493588789));
#62466=CARTESIAN_POINT('Ctrl Pts',(-1.80682978364659,7.70190152708587,60.2156105795414));
#62467=CARTESIAN_POINT('Ctrl Pts',(-1.61556506466181,7.74677132834302,60.2077274507486));
#62468=CARTESIAN_POINT('Ctrl Pts',(-1.42260126968149,7.78451851484864,60.1998443219558));
#62469=CARTESIAN_POINT('Ctrl Pts',(-1.22851113939037,7.81502919894697,60.1919611931629));
#62470=CARTESIAN_POINT('Ctrl Pts',(-1.03440897909205,7.84554177414482,60.1840775757616));
#62471=CARTESIAN_POINT('Ctrl Pts',(-0.839180685131621,7.86881689901266,
60.1761939583602));
#62472=CARTESIAN_POINT('Ctrl Pts',(-0.643406833433908,7.88479223865097,
60.1683103409589));
#62473=CARTESIAN_POINT('Ctrl Pts',(-0.447587938824595,7.90077125383535,
60.1604249097245));
#62474=CARTESIAN_POINT('Ctrl Pts',(-0.251223580167572,7.90944710905219,
60.15253947849));
#62475=CARTESIAN_POINT('Ctrl Pts',(-0.054897316110019,7.91080952145126,
60.1446540472556));
#62476=CARTESIAN_POINT('Ctrl Pts',(0.141507119782876,7.91217247632628,60.1367654762547));
#62477=CARTESIAN_POINT('Ctrl Pts',(0.337873086207642,7.90621618352908,60.1288769052538));
#62478=CARTESIAN_POINT('Ctrl Pts',(0.533618919363395,7.89298244321482,60.1209883342528));
#62479=CARTESIAN_POINT('Ctrl Pts',(0.729573112571408,7.87973461635385,60.113091366327));
#62480=CARTESIAN_POINT('Ctrl Pts',(0.92490550979953,7.85919389251085,60.1051943984011));
#62481=CARTESIAN_POINT('Ctrl Pts',(1.11904034249819,7.83145386961205,60.0972974304752));
#62482=CARTESIAN_POINT('Ctrl Pts',(1.31329359668001,7.80369692540856,60.0893956454301));
#62483=CARTESIAN_POINT('Ctrl Pts',(1.50634749149054,7.76873198829577,60.0814938603849));
#62484=CARTESIAN_POINT('Ctrl Pts',(1.69763803616429,7.72670344313591,60.0735920753397));
#62485=CARTESIAN_POINT('Ctrl Pts',(1.88917602195545,7.68462053255931,60.0656800690547));
#62486=CARTESIAN_POINT('Ctrl Pts',(2.07894576880726,7.63545584984425,60.0577680627698));
#62487=CARTESIAN_POINT('Ctrl Pts',(2.26639889844067,7.57940347475624,60.0498560564848));
#62488=CARTESIAN_POINT('Ctrl Pts',(2.34493975122494,7.55591813018714,60.0465410106274));
#62489=CARTESIAN_POINT('Ctrl Pts',(2.42307415975829,7.53122421861491,60.04322596477));
#62490=CARTESIAN_POINT('Ctrl Pts',(2.50076292126058,7.50533848747998,60.0399109189125));
#62491=CARTESIAN_POINT('Ctrl Pts',(2.68450289825263,7.44411671548642,60.0320705770433));
#62492=CARTESIAN_POINT('Ctrl Pts',(2.86626968753469,7.37605151947719,60.0242302351742));
#62493=CARTESIAN_POINT('Ctrl Pts',(3.04551022817515,7.3012867667337,60.016389893305));
#62494=CARTESIAN_POINT('Ctrl Pts',(3.22455037255659,7.22660560320893,60.0085583171713));
#62495=CARTESIAN_POINT('Ctrl Pts',(3.40106957125277,7.14523993174107,60.0007267410377));
#62496=CARTESIAN_POINT('Ctrl Pts',(3.57452900934866,7.05738360593534,59.992895164904));
#62497=CARTESIAN_POINT('Ctrl Pts',(3.74782824265011,6.96960842304562,59.9850708219083));
#62498=CARTESIAN_POINT('Ctrl Pts',(3.91807303175677,6.87535468175213,59.9772464789126));
#62499=CARTESIAN_POINT('Ctrl Pts',(4.08474349608296,6.77486469025087,59.969422135917));
#62500=CARTESIAN_POINT('Ctrl Pts',(4.25129241672361,6.67444798062336,59.9616034987882));
#62501=CARTESIAN_POINT('Ctrl Pts',(4.41427190443657,6.56780425941505,59.9537848616594));
#62502=CARTESIAN_POINT('Ctrl Pts',(4.57318553252301,6.45522231105345,59.9459662245306));
#62503=CARTESIAN_POINT('Ctrl Pts',(4.73201414592293,6.3427005911264,59.9381517701707));
#62504=CARTESIAN_POINT('Ctrl Pts',(4.88678094648591,6.22424717507849,59.9303373158108));
#62505=CARTESIAN_POINT('Ctrl Pts',(5.03701726940283,6.10019491719221,59.9225228614509));
#62506=CARTESIAN_POINT('Ctrl Pts',(5.18720239934277,5.97618493007147,59.9147110698637));
#62507=CARTESIAN_POINT('Ctrl Pts',(5.33285985672674,5.84658012593787,59.9068992782766));
#62508=CARTESIAN_POINT('Ctrl Pts',(5.47355279435779,5.71175461722386,59.8990874866894));
#62509=CARTESIAN_POINT('Ctrl Pts',(5.61425231664508,5.57692279845872,59.8912753294978));
#62510=CARTESIAN_POINT('Ctrl Pts',(5.74998659478077,5.43687002364502,59.8834631723062));
#62511=CARTESIAN_POINT('Ctrl Pts',(5.88035413514493,5.29200871553363,59.8756510151146));
#62512=CARTESIAN_POINT('Ctrl Pts',(6.01073233317344,5.14713556487927,59.8678382192721));
#62513=CARTESIAN_POINT('Ctrl Pts',(6.13574268345728,4.9974533588667,59.8600254234296));
#62514=CARTESIAN_POINT('Ctrl Pts',(6.25502270872204,4.84340912099851,59.8522126275871));
#62515=CARTESIAN_POINT('Ctrl Pts',(6.37433347358118,4.68932518446848,59.8443978183129));
#62516=CARTESIAN_POINT('Ctrl Pts',(6.48791075613094,4.53087725474849,59.8365830090388));
#62517=CARTESIAN_POINT('Ctrl Pts',(6.59543420639039,4.36854307855326,59.8287681997647));
#62518=CARTESIAN_POINT('Ctrl Pts',(6.70300428775412,4.20613850076768,59.8209500013397));
#62519=CARTESIAN_POINT('Ctrl Pts',(6.80451511277483,4.03984461203916,59.8131318029148));
#62520=CARTESIAN_POINT('Ctrl Pts',(6.89969117463817,3.87016571927097,59.8053136044899));
#62521=CARTESIAN_POINT('Ctrl Pts',(6.99497802092188,3.70028932119088,59.7974863057243));
#62522=CARTESIAN_POINT('Ctrl Pts',(7.0839152048176,3.5270203563457,59.7896590069588));
#62523=CARTESIAN_POINT('Ctrl Pts',(7.16627399083047,3.35088616463567,59.7818317081933));
#62524=CARTESIAN_POINT('Ctrl Pts',(7.24868654099437,3.17463699180775,59.7739992997352));
#62525=CARTESIAN_POINT('Ctrl Pts',(7.32451199867448,2.9955191873616,59.7661668912772));
#62526=CARTESIAN_POINT('Ctrl Pts',(7.39357079451981,2.81407745210109,59.7583344828191));
#62527=CARTESIAN_POINT('Ctrl Pts',(7.46272869946862,2.63237532238254,59.7504908337512));
#62528=CARTESIAN_POINT('Ctrl Pts',(7.52510043433205,2.44834293229416,59.7426471846833));
#62529=CARTESIAN_POINT('Ctrl Pts',(7.58055672223744,2.26253857004489,59.7348035356154));
#62530=CARTESIAN_POINT('Ctrl Pts',(7.6104772987424,2.16229071997026,59.7305716169119));
#62531=CARTESIAN_POINT('Ctrl Pts',(7.63838569171401,2.06152721563189,59.7263396982084));
#62532=CARTESIAN_POINT('Ctrl Pts',(7.66426784507321,1.96033655247686,59.7221077795048));
#62533=CARTESIAN_POINT('Ctrl Pts',(7.71269233422802,1.77101280871747,59.714190026352));
#62534=CARTESIAN_POINT('Ctrl Pts',(7.75416568177515,1.57962758394762,59.7062722731992));
#62535=CARTESIAN_POINT('Ctrl Pts',(7.7885102267516,1.38673337299777,59.6983545200463));
#62536=CARTESIAN_POINT('Ctrl Pts',(7.82281531231705,1.19406078361706,59.6904458638221));
#62537=CARTESIAN_POINT('Ctrl Pts',(7.8500078495628,0.999882997071532,59.6825372075979));
#62538=CARTESIAN_POINT('Ctrl Pts',(7.86996001785461,0.80476724422025,59.6746285513738));
#62539=CARTESIAN_POINT('Ctrl Pts',(7.8898929559655,0.609839546680698,59.6667275176239));
#62540=CARTESIAN_POINT('Ctrl Pts',(7.90259939169801,0.413976023955987,59.658826483874));
#62541=CARTESIAN_POINT('Ctrl Pts',(7.90800254266134,0.217753955788902,59.6509254501241));
#62542=CARTESIAN_POINT('Ctrl Pts',(7.91340148584017,0.0216846984879661,
59.6430305694223));
#62543=CARTESIAN_POINT('Ctrl Pts',(7.91150846620884,-0.174742205258469,
59.6351356887204));
#62544=CARTESIAN_POINT('Ctrl Pts',(7.90229848811574,-0.370944207022699,
59.6272408080186));
#62545=CARTESIAN_POINT('Ctrl Pts',(7.89309397856442,-0.567029711349835,
59.6193506150027));
#62546=CARTESIAN_POINT('Ctrl Pts',(7.87658118360316,-0.762890236703942,
59.6114604219868));
#62547=CARTESIAN_POINT('Ctrl Pts',(7.8527871867078,-0.957942795931853,59.6035702289709));
#62548=CARTESIAN_POINT('Ctrl Pts',(7.8290029166758,-1.15291561867838,59.5956832614253));
#62549=CARTESIAN_POINT('Ctrl Pts',(7.79794341847744,-1.34708079217972,59.5877962938796));
#62550=CARTESIAN_POINT('Ctrl Pts',(7.75968768845748,-1.53985972659895,59.579909326334));
#62551=CARTESIAN_POINT('Ctrl Pts',(7.72143528068662,-1.73262191948324,59.5720230437177));
#62552=CARTESIAN_POINT('Ctrl Pts',(7.67598794689021,-1.92399777416498,59.5641367611014));
#62553=CARTESIAN_POINT('Ctrl Pts',(7.62347603004193,-2.11341766325923,59.556250478485));
#62554=CARTESIAN_POINT('Ctrl Pts',(7.5709642054908,-2.30283721942114,59.54836420973));
#62555=CARTESIAN_POINT('Ctrl Pts',(7.5113879141532,-2.49030048463943,59.5404779409749));
#62556=CARTESIAN_POINT('Ctrl Pts',(7.44492776239345,-2.67525169147563,59.5325916722198));
#62557=CARTESIAN_POINT('Ctrl Pts',(7.37845658837979,-2.86023357201797,59.5247040955463));
#62558=CARTESIAN_POINT('Ctrl Pts',(7.30509939563164,-3.04270223978297,59.5168165188729));
#62559=CARTESIAN_POINT('Ctrl Pts',(7.22508553692539,-3.22212041738224,59.5089289421994));
#62560=CARTESIAN_POINT('Ctrl Pts',(7.14504499732114,-3.40159842259356,59.5010387353862));
#62561=CARTESIAN_POINT('Ctrl Pts',(7.05834350931513,-3.57802359641537,59.493148528573));
#62562=CARTESIAN_POINT('Ctrl Pts',(6.96525721812272,-3.75088161441937,59.4852583217598));
#62563=CARTESIAN_POINT('Ctrl Pts',(6.87208103710106,-3.92390655472229,59.4773604956791));
#62564=CARTESIAN_POINT('Ctrl Pts',(6.77250790116481,-4.09335715532156,59.4694626695985));
#62565=CARTESIAN_POINT('Ctrl Pts',(6.66685883195437,-4.25874562691786,59.4615648435179));
#62566=CARTESIAN_POINT('Ctrl Pts',(6.56115126285717,-4.4242256772373,59.4536626442617));
#62567=CARTESIAN_POINT('Ctrl Pts',(6.44936124829765,-4.58563883126795,59.4457604450055));
#62568=CARTESIAN_POINT('Ctrl Pts',(6.33185140915414,-4.74252872762967,59.4378582457493));
#62569=CARTESIAN_POINT('Ctrl Pts',(6.21419972672546,-4.89960800199133,59.4299465079395));
#62570=CARTESIAN_POINT('Ctrl Pts',(6.09081464487292,-5.05215284559114,59.4220347701297));
#62571=CARTESIAN_POINT('Ctrl Pts',(5.96209779950831,-5.1997414194456,59.4141230323198));
#62572=CARTESIAN_POINT('Ctrl Pts',(5.90885233461222,-5.26079343020591,59.4108502349122));
#62573=CARTESIAN_POINT('Ctrl Pts',(5.85469493588517,-5.32099778462534,59.4075774375047));
#62574=CARTESIAN_POINT('Ctrl Pts',(5.79965576047404,-5.38032657559002,59.4043046400971));
#62575=CARTESIAN_POINT('Ctrl Pts',(5.65982344722424,-5.53105706929629,59.3959897838355));
#62576=CARTESIAN_POINT('Ctrl Pts',(5.5139920804601,-5.67646244899675,59.387674927574));
#62577=CARTESIAN_POINT('Ctrl Pts',(5.36258350565656,-5.81606560699415,59.3793600713124));
#62578=CARTESIAN_POINT('Ctrl Pts',(5.21136138525026,-5.95549684855477,59.3710554545073));
#62579=CARTESIAN_POINT('Ctrl Pts',(5.05457596951866,-6.08913992139619,59.3627508377022));
#62580=CARTESIAN_POINT('Ctrl Pts',(4.8926869871892,-6.2165533091408,59.3544462208971));
#62581=CARTESIAN_POINT('Ctrl Pts',(4.73098668713763,-6.34381819605548,59.3461512831572));
#62582=CARTESIAN_POINT('Ctrl Pts',(4.56419491403394,-6.46486769894665,59.3378563454173));
#62583=CARTESIAN_POINT('Ctrl Pts',(4.39280624966499,-6.57929891803863,59.3295614076774));
#62584=CARTESIAN_POINT('Ctrl Pts',(4.22167446503814,-6.69355862600904,59.3212789025069));
#62585=CARTESIAN_POINT('Ctrl Pts',(4.04595978210803,-6.80121968385556,59.3129963973365));
#62586=CARTESIAN_POINT('Ctrl Pts',(3.86618772683885,-6.90192099787013,59.304713892166));
#62587=CARTESIAN_POINT('Ctrl Pts',(3.68658081780607,-7.00252980338562,59.2964389956562));
#62588=CARTESIAN_POINT('Ctrl Pts',(3.50292422415731,-7.0961914719479,59.2881640991463));
#62589=CARTESIAN_POINT('Ctrl Pts',(3.31577171043993,-7.18258859773037,59.2798892026364));
#62590=CARTESIAN_POINT('Ctrl Pts',(3.12883327465321,-7.26888689653191,59.2716237715229));
#62591=CARTESIAN_POINT('Ctrl Pts',(2.93840716391858,-7.34793711142126,59.2633583404094));
#62592=CARTESIAN_POINT('Ctrl Pts',(2.74507121305907,-7.41946797521456,59.2550929092959));
#62593=CARTESIAN_POINT('Ctrl Pts',(2.66951983156124,-7.44742064286531,59.2518629629951));
#62594=CARTESIAN_POINT('Ctrl Pts',(2.59352435622807,-7.4742255494801,59.2486330166942));
#62595=CARTESIAN_POINT('Ctrl Pts',(2.51712021785742,-7.49986845276992,59.2454030703934));
#62596=CARTESIAN_POINT('Ctrl Pts',(2.32157511884167,-7.56549767351361,59.2371365002483));
#62597=CARTESIAN_POINT('Ctrl Pts',(2.12357222812108,-7.62343805701521,59.2288699301033));
#62598=CARTESIAN_POINT('Ctrl Pts',(1.9237325732266,-7.67353725388148,59.2206033599582));
#62599=CARTESIAN_POINT('Ctrl Pts',(1.72371385968645,-7.72368134020848,59.2123293828705));
#62600=CARTESIAN_POINT('Ctrl Pts',(1.52185538124776,-7.76597014237096,59.2040554057828));
#62601=CARTESIAN_POINT('Ctrl Pts',(1.3187880454904,-7.80030249997214,59.1957814286951));
#62602=CARTESIAN_POINT('Ctrl Pts',(1.11552557817975,-7.83466784823743,59.1874995009738));
#62603=CARTESIAN_POINT('Ctrl Pts',(0.91105222372173,-7.86106143930347,59.1792175732524));
#62604=CARTESIAN_POINT('Ctrl Pts',(0.706004523238845,-7.87943390182101,
59.170935645531));
#62605=CARTESIAN_POINT('Ctrl Pts',(0.500616932063557,-7.89783681885714,
59.1626399895399));
#62606=CARTESIAN_POINT('Ctrl Pts',(0.294653384464272,-7.90819199911998,
59.1543443335488));
#62607=CARTESIAN_POINT('Ctrl Pts',(0.0887529832293941,-7.91050212742326,
59.1460486775576));
#62608=CARTESIAN_POINT('Ctrl Pts',(-0.11733351212049,-7.91281434363545,
59.1377455238989));
#62609=CARTESIAN_POINT('Ctrl Pts',(-0.323356453953252,-7.9070669972986,
59.1294423702402));
#62610=CARTESIAN_POINT('Ctrl Pts',(-0.528680035056985,-7.89331479294549,
59.1211392165815));
#62611=CARTESIAN_POINT('Ctrl Pts',(-0.734316660042689,-7.87954162147593,
59.1128234036294));
#62612=CARTESIAN_POINT('Ctrl Pts',(-0.939251500532301,-7.85773922317631,
59.1045075906773));
#62613=CARTESIAN_POINT('Ctrl Pts',(-1.14285525923557,-7.82801397906503,
59.0961917777252));
#62614=CARTESIAN_POINT('Ctrl Pts',(-1.22194060497823,-7.8164678699814,59.09296168538));
#62615=CARTESIAN_POINT('Ctrl Pts',(-1.30082524599181,-7.80372693627788,
59.0897315930347));
#62616=CARTESIAN_POINT('Ctrl Pts',(-1.37947282804922,-7.78979946575481,
59.0865015006895));
#62617=CARTESIAN_POINT('Ctrl Pts',(-1.57209219270116,-7.75568906524173,
59.0785905348463));
#62618=CARTESIAN_POINT('Ctrl Pts',(-1.76368872443122,-7.71438698870522,
59.0706795690031));
#62619=CARTESIAN_POINT('Ctrl Pts',(-1.9536858869878,-7.6659658527145,59.0627686031599));
#62620=CARTESIAN_POINT('Ctrl Pts',(-2.14349078997446,-7.61759371443856,
59.0548656424831));
#62621=CARTESIAN_POINT('Ctrl Pts',(-2.3316992164698,-7.56211695071439,59.0469626818062));
#62622=CARTESIAN_POINT('Ctrl Pts',(-2.51774246360124,-7.49965958473978,
59.0390597211294));
#62623=CARTESIAN_POINT('Ctrl Pts',(-2.70363188161947,-7.43725386138789,
59.0311632949839));
#62624=CARTESIAN_POINT('Ctrl Pts',(-2.88735936205729,-7.36787914342932,
59.0232668688384));
#62625=CARTESIAN_POINT('Ctrl Pts',(-3.0683687865582,-7.29170994963975,59.0153704426929));
#62626=CARTESIAN_POINT('Ctrl Pts',(-3.24926203291897,-7.21558964388623,
59.0074790847482));
#62627=CARTESIAN_POINT('Ctrl Pts',(-3.4274403828353,-7.13268368430048,58.9995877268034));
#62628=CARTESIAN_POINT('Ctrl Pts',(-3.60236494652799,-7.04321572806246,
58.9916963688587));
#62629=CARTESIAN_POINT('Ctrl Pts',(-3.77720959417117,-6.95378864616175,
58.9838086161604));
#62630=CARTESIAN_POINT('Ctrl Pts',(-3.94880311176592,-6.85780569820013,
58.975920863462));
#62631=CARTESIAN_POINT('Ctrl Pts',(-4.11662833311003,-6.75553788880173,
58.9680331107637));
#62632=CARTESIAN_POINT('Ctrl Pts',(-4.28440792071733,-6.65329788727548,
58.9601475028421));
#62633=CARTESIAN_POINT('Ctrl Pts',(-4.44842096051296,-6.54477660959954,
58.9522618949205));
#62634=CARTESIAN_POINT('Ctrl Pts',(-4.60817631522549,-6.43029019934519,
58.9443762869989));
#62635=CARTESIAN_POINT('Ctrl Pts',(-4.76795051169629,-6.31579028641188,
58.9364897490382));
#62636=CARTESIAN_POINT('Ctrl Pts',(-4.92346573571054,-6.19532403030867,
58.9286032110776));
#62637=CARTESIAN_POINT('Ctrl Pts',(-5.07426067561686,-6.06925033228062,
58.9207166731169));
#62638=CARTESIAN_POINT('Ctrl Pts',(-5.22507461283565,-5.94316075134934,
58.9128291416015));
#62639=CARTESIAN_POINT('Ctrl Pts',(-5.37116681609724,-5.81146254138928,
58.9049416100861));
#62640=CARTESIAN_POINT('Ctrl Pts',(-5.51210988437816,-5.67455422236325,
58.8970540785707));
#62641=CARTESIAN_POINT('Ctrl Pts',(-5.65309433250902,-5.53760570806003,
58.889164231334));
#62642=CARTESIAN_POINT('Ctrl Pts',(-5.7889263859168,-5.39544427648208,58.8812743840973));
#62643=CARTESIAN_POINT('Ctrl Pts',(-5.91921609724654,-5.24850471983187,
58.8733845368605));
#62644=CARTESIAN_POINT('Ctrl Pts',(-6.04956589922947,-5.10149739348712,
58.8654910507634));
#62645=CARTESIAN_POINT('Ctrl Pts',(-6.17436803699042,-4.9497078081706,58.8575975646663));
#62646=CARTESIAN_POINT('Ctrl Pts',(-6.29327322210822,-4.79360335779836,
58.8497040785691));
#62647=CARTESIAN_POINT('Ctrl Pts',(-6.41231586145556,-4.63731845089738,
58.841801467613));
#62648=CARTESIAN_POINT('Ctrl Pts',(-6.52544772314626,-4.47670898990953,
58.8338988566568));
#62649=CARTESIAN_POINT('Ctrl Pts',(-6.63236254373327,-4.31227180132282,
58.8259962457006));
#62650=CARTESIAN_POINT('Ctrl Pts',(-6.73934827605431,-4.14772554903365,
58.8180883933023));
#62651=CARTESIAN_POINT('Ctrl Pts',(-6.84010857048051,-3.97934680260961,
58.810180540904));
#62652=CARTESIAN_POINT('Ctrl Pts',(-6.93438330255126,-3.8076566564356,58.8022726885057));
#62653=CARTESIAN_POINT('Ctrl Pts',(-7.02878702919564,-3.63573158944329,
58.7943540159223));
#62654=CARTESIAN_POINT('Ctrl Pts',(-7.11668731464863,-3.46048637948607,
58.786435343339));
#62655=CARTESIAN_POINT('Ctrl Pts',(-7.19787183142198,-3.28246280990692,
58.7785166707556));
#62656=CARTESIAN_POINT('Ctrl Pts',(-7.23142521223477,-3.20888606324205,
58.775243900931));
#62657=CARTESIAN_POINT('Ctrl Pts',(-7.2638320247923,-3.13483492169906,58.7719711311064));
#62658=CARTESIAN_POINT('Ctrl Pts',(-7.29507977676371,-3.06034835446117,
58.7686983612817));
#62659=CARTESIAN_POINT('Ctrl Pts',(-7.37856743028714,-2.86133535911363,
58.7599541843109));
#62660=CARTESIAN_POINT('Ctrl Pts',(-7.4539897791399,-2.6587079227428,58.75121000734));
#62661=CARTESIAN_POINT('Ctrl Pts',(-7.52105080707951,-2.45310329120661,
58.7424658303692));
#62662=CARTESIAN_POINT('Ctrl Pts',(-7.58782306424936,-2.24838401155866,
58.7337593066045));
#62663=CARTESIAN_POINT('Ctrl Pts',(-7.64630574341749,-2.04071331339552,
58.7250527828399));
#62664=CARTESIAN_POINT('Ctrl Pts',(-7.69625194727979,-1.83074492051518,
58.7163462590753));
#62665=CARTESIAN_POINT('Ctrl Pts',(-7.74606533383241,-1.6213348771169,58.7076628877621));
#62666=CARTESIAN_POINT('Ctrl Pts',(-7.78738746955122,-1.40963953497845,
58.698979516449));
#62667=CARTESIAN_POINT('Ctrl Pts',(-7.82002030366252,-1.19632915633863,
58.6902961451359));
#62668=CARTESIAN_POINT('Ctrl Pts',(-7.85250523590745,-0.983985564800771,
58.6816521294858));
#62669=CARTESIAN_POINT('Ctrl Pts',(-7.87637936152144,-0.770041747798524,
58.6730081138357));
#62670=CARTESIAN_POINT('Ctrl Pts',(-7.89149535562621,-0.555177496058689,
58.6643640981856));
#62671=CARTESIAN_POINT('Ctrl Pts',(-7.90433832557822,-0.372622838407328,
58.6570199015361));
#62672=CARTESIAN_POINT('Ctrl Pts',(-7.91085984755608,-0.189404127067722,
58.6496757048866));
#62673=CARTESIAN_POINT('Ctrl Pts',(-7.91099776453137,-0.00594723293680172,
58.642331508237));
#62674=CARTESIAN_POINT('',(-7.911,4.9293902293357E-13,56.642331508237));
#62675=CARTESIAN_POINT('Ctrl Pts',(-7.911,6.63358257213531E-13,58.642331508237));
#62676=CARTESIAN_POINT('Ctrl Pts',(-7.91099999999982,2.20167589666731,58.5537440725043));
#62677=CARTESIAN_POINT('Ctrl Pts',(-6.94214576672346,4.38610418338718,58.4651566367716));
#62678=CARTESIAN_POINT('Ctrl Pts',(-3.67820201488267,7.34180684107638,58.2879817653061));
#62679=CARTESIAN_POINT('Ctrl Pts',(-1.40868175871738,8.08992666571334,58.1993943295734));
#62680=CARTESIAN_POINT('Ctrl Pts',(2.97309270521256,7.6545422802526,58.022219458108));
#62681=CARTESIAN_POINT('Ctrl Pts',(5.05102072675575,6.47444880834243,57.9336320223752));
#62682=CARTESIAN_POINT('Ctrl Pts',(7.66951518847849,2.93425195367758,57.7564571509098));
#62683=CARTESIAN_POINT('Ctrl Pts',(8.18956872247063,0.601881960099865,57.6678697151771));
#62684=CARTESIAN_POINT('Ctrl Pts',(7.32306689761382,-3.71537198232365,57.4906948437116));
#62685=CARTESIAN_POINT('Ctrl Pts',(5.94329958850274,-5.6664351893643,57.4021074079789));
#62686=CARTESIAN_POINT('Ctrl Pts',(2.16154501637974,-7.9220591323296,57.2249325365135));
#62687=CARTESIAN_POINT('Ctrl Pts',(-0.210816529298906,-8.20894963713003,
57.1363451007807));
#62688=CARTESIAN_POINT('Ctrl Pts',(-4.42123908576293,-6.9198224471792,56.9591702293153));
#62689=CARTESIAN_POINT('Ctrl Pts',(-6.22631625634065,-5.35390358803658,
56.8705827935826));
#62690=CARTESIAN_POINT('Ctrl Pts',(-7.65317280859467,-2.31334857514629,
56.7354407413122));
#62691=CARTESIAN_POINT('Ctrl Pts',(-7.91100000000007,-1.15702837836549,
56.6888861247746));
#62692=CARTESIAN_POINT('Ctrl Pts',(-7.911,4.9293902293357E-13,56.642331508237));
#62693=CARTESIAN_POINT('',(-7.911,1.51545442861334E-13,52.642331508237));
#62694=CARTESIAN_POINT('Ctrl Pts',(-7.91099980728415,0.00174618159620388,
56.6387979549077));
#62695=CARTESIAN_POINT('Ctrl Pts',(-7.91084820449805,0.68857601317406,56.6151031213445));
#62696=CARTESIAN_POINT('Ctrl Pts',(-7.82125530223842,1.37238516702683,56.5930307210947));
#62697=CARTESIAN_POINT('Ctrl Pts',(-7.61840630808201,2.1340358358552,56.5631137361859));
#62698=CARTESIAN_POINT('Ctrl Pts',(-7.59039980943151,2.23160318732258,56.5591722855295));
#62699=CARTESIAN_POINT('Ctrl Pts',(-7.55535200479549,2.34539675655594,56.5544191086037));
#62700=CARTESIAN_POINT('Ctrl Pts',(-7.55012304885116,2.36217522631301,56.5537142523069));
#62701=CARTESIAN_POINT('Ctrl Pts',(-7.54316836291411,2.38423213767859,56.5527821986768));
#62702=CARTESIAN_POINT('Ctrl Pts',(-7.54149288624599,2.38952649786587,56.5525580620559));
#62703=CARTESIAN_POINT('Ctrl Pts',(-7.53874602785033,2.39817466492789,56.5521912589115));
#62704=CARTESIAN_POINT('Ctrl Pts',(-7.5376779778534,2.40152953304869,56.5520487973686));
#62705=CARTESIAN_POINT('Ctrl Pts',(-7.5356043339553,2.4080280762334,56.5517725153031));
#62706=CARTESIAN_POINT('Ctrl Pts',(-7.53459901537137,2.41117182534847,56.551638712335));
#62707=CARTESIAN_POINT('Ctrl Pts',(-7.53226961020979,2.41844046589533,56.5513290063651));
#62708=CARTESIAN_POINT('Ctrl Pts',(-7.53094410322701,2.42256489736126,56.5511530163397));
#62709=CARTESIAN_POINT('Ctrl Pts',(-7.52737283904243,2.43364594385742,56.550679507872));
#62710=CARTESIAN_POINT('Ctrl Pts',(-7.52512083150402,2.44060052211482,56.5503816097484));
#62711=CARTESIAN_POINT('Ctrl Pts',(-7.50915335961539,2.48967855821255,56.5482743345795));
#62712=CARTESIAN_POINT('Ctrl Pts',(-7.4950941684472,2.5316885195273,56.5464443878642));
#62713=CARTESIAN_POINT('Ctrl Pts',(-7.22814463990183,3.3076375383237,56.5121901198727));
#62714=CARTESIAN_POINT('Ctrl Pts',(-6.86894496350255,4.00052861050787,56.4745166261569));
#62715=CARTESIAN_POINT('Ctrl Pts',(-6.33139272484424,4.74527014589443,56.4329966167731));
#62716=CARTESIAN_POINT('Ctrl Pts',(-6.24511494801689,4.85825731680045,56.426648399571));
#62717=CARTESIAN_POINT('Ctrl Pts',(-6.02994215817876,5.12483117511727,56.4115888345783));
#62718=CARTESIAN_POINT('Ctrl Pts',(-5.89815979262237,5.27596586528857,56.4029831231325));
#62719=CARTESIAN_POINT('Ctrl Pts',(-5.68150113490863,5.50616413561056,56.3897890670311));
#62720=CARTESIAN_POINT('Ctrl Pts',(-5.60039079547315,5.58864233171825,56.3850422023488));
#62721=CARTESIAN_POINT('Ctrl Pts',(-5.50942505051269,5.6771721421646,56.3799224421398));
#62722=CARTESIAN_POINT('Ctrl Pts',(-5.50133474165043,5.6850122234436,56.3794688224971));
#62723=CARTESIAN_POINT('Ctrl Pts',(-5.48797801151744,5.69790062783065,56.3787227404949));
#62724=CARTESIAN_POINT('Ctrl Pts',(-5.48272131887853,5.70295898279377,56.378429828522));
#62725=CARTESIAN_POINT('Ctrl Pts',(-5.4733390843291,5.71196225916846,56.3779083084703));
#62726=CARTESIAN_POINT('Ctrl Pts',(-5.46921625872517,5.71590999734119,56.3776795745311));
#62727=CARTESIAN_POINT('Ctrl Pts',(-5.46122648705428,5.72354390199454,56.3772371469045));
#62728=CARTESIAN_POINT('Ctrl Pts',(-5.45736007406763,5.72723061898702,56.3770234287103));
#62729=CARTESIAN_POINT('Ctrl Pts',(-5.44942715339064,5.7347795208465,56.376585712194));
#62730=CARTESIAN_POINT('Ctrl Pts',(-5.44536026712633,5.73864130384497,56.376361731779));
#62731=CARTESIAN_POINT('Ctrl Pts',(-5.43562095466984,5.74786976319059,56.3758263472073));
#62732=CARTESIAN_POINT('Ctrl Pts',(-5.42994467687421,5.75323237702149,56.3755151233153));
#62733=CARTESIAN_POINT('Ctrl Pts',(-5.4095039470628,5.77248637984806,56.3743972821306));
#62734=CARTESIAN_POINT('Ctrl Pts',(-5.39469399256677,5.78632946637346,56.3735928002347));
#62735=CARTESIAN_POINT('Ctrl Pts',(-5.18158927956634,5.98399230869551,56.3620939646881));
#62736=CARTESIAN_POINT('Ctrl Pts',(-4.97404324807321,6.1575921851026,56.3518575389367));
#62737=CARTESIAN_POINT('Ctrl Pts',(-4.65321842494282,6.3991156360056,56.3371904487959));
#62738=CARTESIAN_POINT('Ctrl Pts',(-4.54648912519221,6.47538112010362,56.3324853777765));
#62739=CARTESIAN_POINT('Ctrl Pts',(-4.31160821998684,6.63454846901163,56.3224457912904));
#62740=CARTESIAN_POINT('Ctrl Pts',(-4.18285442050865,6.71646701018821,56.3171362598408));
#62741=CARTESIAN_POINT('Ctrl Pts',(-3.94581484207716,6.85782010059937,56.307614806393));
#62742=CARTESIAN_POINT('Ctrl Pts',(-3.8383543163265,6.91853942024402,56.3033881959249));
#62743=CARTESIAN_POINT('Ctrl Pts',(-3.5156802167663,7.09103000341992,56.2908673393033));
#62744=CARTESIAN_POINT('Ctrl Pts',(-3.29670491068004,7.19544623343171,56.2825924325451));
#62745=CARTESIAN_POINT('Ctrl Pts',(-2.858419944565,7.38022555928906,56.2659118569252));
#62746=CARTESIAN_POINT('Ctrl Pts',(-2.6396655276265,7.46126317552849,56.2575302895396));
#62747=CARTESIAN_POINT('Ctrl Pts',(-2.319361546293,7.56406915329006,56.2447726794681));
#62748=CARTESIAN_POINT('Ctrl Pts',(-2.22045331329989,7.59369248779834,56.2407678726379));
#62749=CARTESIAN_POINT('Ctrl Pts',(-2.10383913719518,7.62614575653695,56.2359400614301));
#62750=CARTESIAN_POINT('Ctrl Pts',(-2.08666471780555,7.63086289753016,56.2352263638029));
#62751=CARTESIAN_POINT('Ctrl Pts',(-2.0640349636981,7.63699629647951,56.2342822679548));
#62752=CARTESIAN_POINT('Ctrl Pts',(-2.05859375640707,7.63846480057348,56.2340549831037));
#62753=CARTESIAN_POINT('Ctrl Pts',(-2.049651950738,7.64086781773522,56.233681010764));
#62754=CARTESIAN_POINT('Ctrl Pts',(-2.04615230225382,7.64180573445595,56.2335345290203));
#62755=CARTESIAN_POINT('Ctrl Pts',(-2.03935960652088,7.64362119741479,56.2332499892446));
#62756=CARTESIAN_POINT('Ctrl Pts',(-2.03606663342336,7.64449902076446,56.2331119476084));
#62757=CARTESIAN_POINT('Ctrl Pts',(-2.02844902415641,7.64652441151045,56.2327923827668));
#62758=CARTESIAN_POINT('Ctrl Pts',(-2.02412398308849,7.64767043748335,56.2326107693108));
#62759=CARTESIAN_POINT('Ctrl Pts',(-2.01022576107042,7.65134049733844,56.2320266119199));
#62760=CARTESIAN_POINT('Ctrl Pts',(-2.00064884565773,7.6538502213843,56.2316232380672));
#62761=CARTESIAN_POINT('Ctrl Pts',(-1.91442021617504,7.67627437698169,56.2279838990482));
#62762=CARTESIAN_POINT('Ctrl Pts',(-1.83748052196763,7.69505410092623,56.2246837374486));
#62763=CARTESIAN_POINT('Ctrl Pts',(-1.08233639329698,7.86740167957996,56.1918690604129));
#62764=CARTESIAN_POINT('Ctrl Pts',(-0.386971163054789,7.93206985564289,
56.1586017557931));
#62765=CARTESIAN_POINT('Ctrl Pts',(0.540843078214959,7.8959332211934,56.1164228042473));
#62766=CARTESIAN_POINT('Ctrl Pts',(0.77329510403888,7.87656632993453,56.1060100791956));
#62767=CARTESIAN_POINT('Ctrl Pts',(1.19459226643754,7.82263211511709,56.0875430221281));
#62768=CARTESIAN_POINT('Ctrl Pts',(1.38368227988135,7.7914089784371,56.0794042934287));
#62769=CARTESIAN_POINT('Ctrl Pts',(1.65828317213273,7.7357524261427,56.0678137934268));
#62770=CARTESIAN_POINT('Ctrl Pts',(1.74480491738745,7.71669781337492,56.0641951087904));
#62771=CARTESIAN_POINT('Ctrl Pts',(1.84493711061928,7.69287550797246,56.0600442287473));
#62772=CARTESIAN_POINT('Ctrl Pts',(1.8588749301217,7.68951952466818,56.0594672858678));
#62773=CARTESIAN_POINT('Ctrl Pts',(1.87873080151293,7.68468143731248,56.058646548968));
#62774=CARTESIAN_POINT('Ctrl Pts',(1.88465634121034,7.68323035534389,56.058401768185));
#62775=CARTESIAN_POINT('Ctrl Pts',(1.89660855662261,7.68028876574276,56.057908329374));
#62776=CARTESIAN_POINT('Ctrl Pts',(1.90263516825522,7.6787980152487,56.0576596792959));
#62777=CARTESIAN_POINT('Ctrl Pts',(1.91426583863499,7.67590650454088,56.0571801094962));
#62778=CARTESIAN_POINT('Ctrl Pts',(1.91987012863229,7.67450669794312,56.0569491596193));
#62779=CARTESIAN_POINT('Ctrl Pts',(1.93313891194257,7.6711770554237,56.0564026732089));
#62780=CARTESIAN_POINT('Ctrl Pts',(1.94080206316005,7.66924186739701,56.056087307343));
#62781=CARTESIAN_POINT('Ctrl Pts',(1.96763555511756,7.66242276802149,56.0549838752324));
#62782=CARTESIAN_POINT('Ctrl Pts',(1.98679053717376,7.65747841800647,56.0541977357732));
#62783=CARTESIAN_POINT('Ctrl Pts',(2.21985310861163,7.5963861241652,56.0446510118746));
#62784=CARTESIAN_POINT('Ctrl Pts',(2.43134146712307,7.53136226518839,56.036181076726));
#62785=CARTESIAN_POINT('Ctrl Pts',(2.77083090779123,7.41118926126218,56.0227849629902));
#62786=CARTESIAN_POINT('Ctrl Pts',(2.90058178980716,7.36137603874583,56.0177132520234));
#62787=CARTESIAN_POINT('Ctrl Pts',(3.32410669621311,7.18584119993391,56.0012272631558));
#62788=CARTESIAN_POINT('Ctrl Pts',(3.6115808603374,7.04574267515473,55.9901609389683));
#62789=CARTESIAN_POINT('Ctrl Pts',(4.36862835434026,6.61826197626851,55.9600633063668));
#62790=CARTESIAN_POINT('Ctrl Pts',(4.81790901423686,6.29872335029346,55.9411649348257));
#62791=CARTESIAN_POINT('Ctrl Pts',(5.24656979657568,5.92097057094752,55.9184160237587));
#62792=CARTESIAN_POINT('Ctrl Pts',(5.26270917098474,5.90663011349884,55.9175517850571));
#62793=CARTESIAN_POINT('Ctrl Pts',(5.28342709550625,5.88806911440244,55.9164320875113));
#62794=CARTESIAN_POINT('Ctrl Pts',(5.28805977367231,5.88390887074007,55.9161810486407));
#62795=CARTESIAN_POINT('Ctrl Pts',(5.29552087569938,5.87719271317207,55.9157756567925));
#62796=CARTESIAN_POINT('Ctrl Pts',(5.29835237955799,5.87464020980595,55.9156215573586));
#62797=CARTESIAN_POINT('Ctrl Pts',(5.30375298379715,5.86976467021196,55.9153271549309));
#62798=CARTESIAN_POINT('Ctrl Pts',(5.3063223985772,5.8674419979258,55.915186878865));
#62799=CARTESIAN_POINT('Ctrl Pts',(5.31217295970117,5.86214628367038,55.9148669926695));
#62800=CARTESIAN_POINT('Ctrl Pts',(5.31545313422395,5.85917217554512,55.9146873028564));
#62801=CARTESIAN_POINT('Ctrl Pts',(5.32407911899824,5.85133785847745,55.9142138688774));
#62802=CARTESIAN_POINT('Ctrl Pts',(5.32942075978555,5.84647308758946,55.913919786027));
#62803=CARTESIAN_POINT('Ctrl Pts',(5.36308930692496,5.81572578500935,55.9120604737163));
#62804=CARTESIAN_POINT('Ctrl Pts',(5.39123383724379,5.78964514813365,55.9104807227237));
#62805=CARTESIAN_POINT('Ctrl Pts',(5.8756537307755,5.33415365066025,55.8828638661877));
#62806=CARTESIAN_POINT('Ctrl Pts',(6.27949311272607,4.85225847995284,55.8534082387061));
#62807=CARTESIAN_POINT('Ctrl Pts',(6.78989512557029,4.07126134493764,55.8107953536195));
#62808=CARTESIAN_POINT('Ctrl Pts',(6.94251186674836,3.8051798655182,55.7970010505346));
#62809=CARTESIAN_POINT('Ctrl Pts',(7.16667801156803,3.35573576703768,55.7751570648926));
#62810=CARTESIAN_POINT('Ctrl Pts',(7.24751566716183,3.1773825500198,55.7668367656126));
#62811=CARTESIAN_POINT('Ctrl Pts',(7.35559268135786,2.91328085874929,55.7550296928161));
#62812=CARTESIAN_POINT('Ctrl Pts',(7.38811691399282,2.82978412726945,55.751369050144));
#62813=CARTESIAN_POINT('Ctrl Pts',(7.42420634024071,2.7322679062073,55.7471756010224));
#62814=CARTESIAN_POINT('Ctrl Pts',(7.42915951143515,2.71877116547598,55.7465970073129));
#62815=CARTESIAN_POINT('Ctrl Pts',(7.43616375053874,2.69952346777953,55.7457744264836));
#62816=CARTESIAN_POINT('Ctrl Pts',(7.43824498144354,2.69378356112058,55.7455294451465));
#62817=CARTESIAN_POINT('Ctrl Pts',(7.44242982144057,2.68220020204575,55.7450357123211));
#62818=CARTESIAN_POINT('Ctrl Pts',(7.44453319856616,2.67635667028695,55.7447869686078));
#62819=CARTESIAN_POINT('Ctrl Pts',(7.44857844331403,2.66507664054373,55.7443074480895));
#62820=CARTESIAN_POINT('Ctrl Pts',(7.45052124514183,2.65964048360582,55.7440766406591));
#62821=CARTESIAN_POINT('Ctrl Pts',(7.45510523723345,2.64676956932004,55.74353084638));
#62822=CARTESIAN_POINT('Ctrl Pts',(7.45774126125705,2.63933297102187,55.7432160295765));
#62823=CARTESIAN_POINT('Ctrl Pts',(7.46555432544673,2.61718604773805,55.7422800576544));
#62824=CARTESIAN_POINT('Ctrl Pts',(7.47069901234106,2.60246430623219,55.7416599656982));
#62825=CARTESIAN_POINT('Ctrl Pts',(7.51719198918745,2.46814868853098,55.736021268645));
#62826=CARTESIAN_POINT('Ctrl Pts',(7.55570983343924,2.34759112008196,55.7310961753692));
#62827=CARTESIAN_POINT('Ctrl Pts',(7.5983421122805,2.2022127096188,55.7253061348779));
#62828=CARTESIAN_POINT('Ctrl Pts',(7.60525071758175,2.17823442479767,55.7243559319127));
#62829=CARTESIAN_POINT('Ctrl Pts',(7.6283771171136,2.09651625872132,55.7211335542453));
#62830=CARTESIAN_POINT('Ctrl Pts',(7.64405187247924,2.03862429279536,55.7188777140182));
#62831=CARTESIAN_POINT('Ctrl Pts',(7.68415106515411,1.88355574459934,55.7129027526282));
#62832=CARTESIAN_POINT('Ctrl Pts',(7.70739044450382,1.78608316840343,55.7092174628827));
#62833=CARTESIAN_POINT('Ctrl Pts',(7.82155584536658,1.26341895491585,55.6897809216656));
#62834=CARTESIAN_POINT('Ctrl Pts',(7.87916492944024,0.831707580002971,55.6749176540655));
#62835=CARTESIAN_POINT('Ctrl Pts',(7.92672072185146,-0.11366514564192,55.6423643266124));
#62836=CARTESIAN_POINT('Ctrl Pts',(7.90277216693031,-0.626015841465745,
55.6247047098509));
#62837=CARTESIAN_POINT('Ctrl Pts',(7.82528101283342,-1.16180071787526,55.6032593012995));
#62838=CARTESIAN_POINT('Ctrl Pts',(7.82086231688285,-1.19118277998328,55.6020734922564));
#62839=CARTESIAN_POINT('Ctrl Pts',(7.81522175338531,-1.22730470455429,55.6006029275131));
#62840=CARTESIAN_POINT('Ctrl Pts',(7.81415646726147,-1.23406912165202,55.6003269896369));
#62841=CARTESIAN_POINT('Ctrl Pts',(7.81247112870737,-1.24468110429705,55.5998932239698));
#62842=CARTESIAN_POINT('Ctrl Pts',(7.81185701158553,-1.24852962268448,55.5997357346517));
#62843=CARTESIAN_POINT('Ctrl Pts',(7.81076264030382,-1.25535535658988,55.5994560883905));
#62844=CARTESIAN_POINT('Ctrl Pts',(7.81028352671805,-1.2583327567511,55.599333996981));
#62845=CARTESIAN_POINT('Ctrl Pts',(7.80917653949306,-1.26518702149594,55.599052678061));
#62846=CARTESIAN_POINT('Ctrl Pts',(7.8085474815737,-1.26906369116488,55.5988933821728));
#62847=CARTESIAN_POINT('Ctrl Pts',(7.80681295743093,-1.27970285659211,55.5984556945209));
#62848=CARTESIAN_POINT('Ctrl Pts',(7.80570159982083,-1.28646433563965,55.5981769594429));
#62849=CARTESIAN_POINT('Ctrl Pts',(7.80005370564234,-1.32054925730895,55.5967689789163));
#62850=CARTESIAN_POINT('Ctrl Pts',(7.79538253039404,-1.34784988784197,55.5956319684102));
#62851=CARTESIAN_POINT('Ctrl Pts',(7.78963031808254,-1.38043819715496,55.5942641433041));
#62852=CARTESIAN_POINT('Ctrl Pts',(7.78868706162772,-1.38575032539242,55.594040841202));
#62853=CARTESIAN_POINT('Ctrl Pts',(7.69839780702839,-1.89122697518797,55.5727607158837));
#62854=CARTESIAN_POINT('Ctrl Pts',(7.56108723122098,-2.38158539426013,55.5492259732346));
#62855=CARTESIAN_POINT('Ctrl Pts',(7.26975362807105,-3.13434227944995,55.5118692456279));
#62856=CARTESIAN_POINT('Ctrl Pts',(7.1460330732033,-3.40699911797003,55.4980459094883));
#62857=CARTESIAN_POINT('Ctrl Pts',(6.87882754887679,-3.91689899996896,55.4721219402893));
#62858=CARTESIAN_POINT('Ctrl Pts',(6.73773519694541,-4.15491393276698,55.4599867327234));
#62859=CARTESIAN_POINT('Ctrl Pts',(6.50374156720802,-4.50627029680868,55.4421399394595));
#62860=CARTESIAN_POINT('Ctrl Pts',(6.41969039350662,-4.62522482468499,55.4361082705959));
#62861=CARTESIAN_POINT('Ctrl Pts',(6.31573783490234,-4.76404758226554,55.4290787944988));
#62862=CARTESIAN_POINT('Ctrl Pts',(6.29895824101679,-4.78621132675783,55.4279567753096));
#62863=CARTESIAN_POINT('Ctrl Pts',(6.27625922212665,-4.81586776477866,55.4264557325126));
#62864=CARTESIAN_POINT('Ctrl Pts',(6.27044265640776,-4.82343871576265,55.4260725585723));
#62865=CARTESIAN_POINT('Ctrl Pts',(6.26075616423924,-4.83599970306573,55.4254368709044));
#62866=CARTESIAN_POINT('Ctrl Pts',(6.25689395081798,-4.84099565839245,55.4251840449573));
#62867=CARTESIAN_POINT('Ctrl Pts',(6.24937209811012,-4.85070149102846,55.4246928878978));
#62868=CARTESIAN_POINT('Ctrl Pts',(6.24571310664411,-4.85541186362224,55.4244545307481));
#62869=CARTESIAN_POINT('Ctrl Pts',(6.23721541806494,-4.86632579319855,55.4239022744056));
#62870=CARTESIAN_POINT('Ctrl Pts',(6.23237278316318,-4.87252628408058,55.4235885357871));
#62871=CARTESIAN_POINT('Ctrl Pts',(6.21668772134498,-4.89254773626665,55.4225755059916));
#62872=CARTESIAN_POINT('Ctrl Pts',(6.20580847202311,-4.90633985677398,55.4218777181546));
#62873=CARTESIAN_POINT('Ctrl Pts',(6.10395458900891,-5.03458389145896,55.4153897574647));
#62874=CARTESIAN_POINT('Ctrl Pts',(6.00986696252896,-5.14653266939225,55.4097293684111));
#62875=CARTESIAN_POINT('Ctrl Pts',(5.90796260437688,-5.26117385195258,55.4039176977383));
#62876=CARTESIAN_POINT('Ctrl Pts',(5.90319057552617,-5.26652764775033,55.4036462524957));
#62877=CARTESIAN_POINT('Ctrl Pts',(5.89337042810843,-5.2775148712053,55.4030891014652));
#62878=CARTESIAN_POINT('Ctrl Pts',(5.88832149611894,-5.28314756347061,55.4028034284323));
#62879=CARTESIAN_POINT('Ctrl Pts',(5.8770420733321,-5.29569486457616,55.4021669600065));
#62880=CARTESIAN_POINT('Ctrl Pts',(5.87080743907096,-5.30260574099432,55.401816329154));
#62881=CARTESIAN_POINT('Ctrl Pts',(5.83984553269885,-5.33680440087251,55.4000808297787));
#62882=CARTESIAN_POINT('Ctrl Pts',(5.81493996889262,-5.36393048591619,55.3987030061713));
#62883=CARTESIAN_POINT('Ctrl Pts',(5.72405437049743,-5.4615422688328,55.3937389888923));
#62884=CARTESIAN_POINT('Ctrl Pts',(5.65697394735353,-5.53099347393197,55.3901957522666));
#62885=CARTESIAN_POINT('Ctrl Pts',(5.13709506540786,-6.04989160703775,55.3635699516005));
#62886=CARTESIAN_POINT('Ctrl Pts',(4.63273366873903,-6.4442731164629,55.3426791621788));
#62887=CARTESIAN_POINT('Ctrl Pts',(3.8924164676964,-6.89089218349173,55.312254666605));
#62888=CARTESIAN_POINT('Ctrl Pts',(3.69339570909893,-6.99957984611477,55.3040694496615));
#62889=CARTESIAN_POINT('Ctrl Pts',(3.40410149492052,-7.14179072188917,55.2917915188516));
#62890=CARTESIAN_POINT('Ctrl Pts',(3.31745094337936,-7.18245080889313,55.2880670801005));
#62891=CARTESIAN_POINT('Ctrl Pts',(3.21460597424199,-7.22845191248364,55.2835676450676));
#62892=CARTESIAN_POINT('Ctrl Pts',(3.19910254904616,-7.23532663346636,55.2828872863945));
#62893=CARTESIAN_POINT('Ctrl Pts',(3.17854109133271,-7.24436524443233,55.2819820443794));
#62894=CARTESIAN_POINT('Ctrl Pts',(3.17350263495465,-7.2465738311059,55.2817599892528));
#62895=CARTESIAN_POINT('Ctrl Pts',(3.16523460645284,-7.25018781076949,55.2813952146852));
#62896=CARTESIAN_POINT('Ctrl Pts',(3.16200638500934,-7.25159630884115,55.281252693481));
#62897=CARTESIAN_POINT('Ctrl Pts',(3.15575419107739,-7.25431922082423,55.2809764799473));
#62898=CARTESIAN_POINT('Ctrl Pts',(3.1527303366362,-7.2556339003957,55.2808428047618));
#62899=CARTESIAN_POINT('Ctrl Pts',(3.14571336446607,-7.25867945079962,55.2805324071035));
#62900=CARTESIAN_POINT('Ctrl Pts',(3.14171965223378,-7.26040891186302,55.2803555950225));
#62901=CARTESIAN_POINT('Ctrl Pts',(3.12908647037998,-7.26586728520703,55.2797958245416));
#62902=CARTESIAN_POINT('Ctrl Pts',(3.12044180225646,-7.26958406668447,55.2794120938581));
#62903=CARTESIAN_POINT('Ctrl Pts',(3.04172521177515,-7.30326204433802,55.2759117958871));
#62904=CARTESIAN_POINT('Ctrl Pts',(2.97123256422584,-7.33222374590426,55.272733090728));
#62905=CARTESIAN_POINT('Ctrl Pts',(2.43191404305138,-7.5447468374978,55.2481434555556));
#62906=CARTESIAN_POINT('Ctrl Pts',(1.94697302397703,-7.68418104906985,55.2245559813647));
#62907=CARTESIAN_POINT('Ctrl Pts',(1.00887152905044,-7.85935212631907,55.1800277190929));
#62908=CARTESIAN_POINT('Ctrl Pts',(0.559325978150801,-7.90407850563647,
55.1591525951807));
#62909=CARTESIAN_POINT('Ctrl Pts',(0.00925545095834248,-7.91161581539457,
55.1350186138469));
#62910=CARTESIAN_POINT('Ctrl Pts',(-0.0898978754489525,-7.91111052715705,
55.1307208119828));
#62911=CARTESIAN_POINT('Ctrl Pts',(-0.3253246899419,-7.90548385530522,55.1206455361017));
#62912=CARTESIAN_POINT('Ctrl Pts',(-0.461528531496933,-7.89870274656284,
55.1149198563143));
#62913=CARTESIAN_POINT('Ctrl Pts',(-0.666568296919142,-7.88317235246538,
55.1064545426749));
#62914=CARTESIAN_POINT('Ctrl Pts',(-0.735572017726542,-7.87703331012308,
55.1036319376856));
#62915=CARTESIAN_POINT('Ctrl Pts',(-0.818239526009785,-7.86858285679967,
55.1002809385554));
#62916=CARTESIAN_POINT('Ctrl Pts',(-0.831987956484899,-7.86714103973553,
55.0997246470571));
#62917=CARTESIAN_POINT('Ctrl Pts',(-0.852997722175903,-7.86488202571483,
55.0988760808557));
#62918=CARTESIAN_POINT('Ctrl Pts',(-0.860261787491571,-7.86409079613217,
55.0985829721546));
#62919=CARTESIAN_POINT('Ctrl Pts',(-0.873404999756046,-7.86264075896253,
55.0980531421119));
#62920=CARTESIAN_POINT('Ctrl Pts',(-0.879284519257728,-7.86198541924955,
55.0978163095551));
#62921=CARTESIAN_POINT('Ctrl Pts',(-0.891018681482649,-7.86066418499986,
55.0973440102623));
#62922=CARTESIAN_POINT('Ctrl Pts',(-0.896873326236978,-7.8599983433187,
55.0971085419958));
#62923=CARTESIAN_POINT('Ctrl Pts',(-0.913289997807218,-7.85811271387323,
55.096448783869));
#62924=CARTESIAN_POINT('Ctrl Pts',(-0.923850335808975,-7.85687817152676,
55.0960249680496));
#62925=CARTESIAN_POINT('Ctrl Pts',(-0.966829367758204,-7.85176591468876,
55.0943024661485));
#62926=CARTESIAN_POINT('Ctrl Pts',(-0.999226614946151,-7.84770878731557,
55.0930095431726));
#62927=CARTESIAN_POINT('Ctrl Pts',(-1.50340318242531,-7.78139772556402,
55.0729716394644));
#62928=CARTESIAN_POINT('Ctrl Pts',(-1.96867227984588,-7.67689802705709,
55.0556970234804));
#62929=CARTESIAN_POINT('Ctrl Pts',(-2.64383141451025,-7.45979175542451,
55.0309089999737));
#62930=CARTESIAN_POINT('Ctrl Pts',(-2.86264026685125,-7.37859266160762,
55.0229059714501));
#62931=CARTESIAN_POINT('Ctrl Pts',(-3.55695528195361,-7.08539436583882,
54.9969469010359));
#62932=CARTESIAN_POINT('Ctrl Pts',(-4.01520842627125,-6.83613969233397,
54.9789572998664));
#62933=CARTESIAN_POINT('Ctrl Pts',(-4.46705360645275,-6.52916711821197,
54.9572455646012));
#62934=CARTESIAN_POINT('Ctrl Pts',(-4.48839543329875,-6.51451437869448,
54.9562105098672));
#62935=CARTESIAN_POINT('Ctrl Pts',(-4.51598331356562,-6.49537334221285,
54.9548604752397));
#62936=CARTESIAN_POINT('Ctrl Pts',(-4.52229545808426,-6.49098019811319,
54.9545507625569));
#62937=CARTESIAN_POINT('Ctrl Pts',(-4.53250468772385,-6.48385262942805,
54.9540485134785));
#62938=CARTESIAN_POINT('Ctrl Pts',(-4.5364057384734,-6.48112387168912,54.9538562858985));
#62939=CARTESIAN_POINT('Ctrl Pts',(-4.54386221993309,-6.47589808463257,
54.9534882657051));
#62940=CARTESIAN_POINT('Ctrl Pts',(-4.54741806257322,-6.47340164367663,
54.9533125048534));
#62941=CARTESIAN_POINT('Ctrl Pts',(-4.55556269303644,-6.46767354235411,
54.9529093338039));
#62942=CARTESIAN_POINT('Ctrl Pts',(-4.56015009855247,-6.46443992771909,
54.9526818191273));
#62943=CARTESIAN_POINT('Ctrl Pts',(-4.57427488508008,-6.45446099506771,
54.9519799718867));
#62944=CARTESIAN_POINT('Ctrl Pts',(-4.58380074190543,-6.44769945155181,
54.9515047820107));
#62945=CARTESIAN_POINT('Ctrl Pts',(-4.65590750633217,-6.39627682941083,
54.9478938751817));
#62946=CARTESIAN_POINT('Ctrl Pts',(-4.71784799825,-6.35072765210209,54.9447124525033));
#62947=CARTESIAN_POINT('Ctrl Pts',(-5.30843764849882,-5.9030170426427,54.9136730013443));
#62948=CARTESIAN_POINT('Ctrl Pts',(-5.78511889449883,-5.43668609128565,
54.8833606481556));
#62949=CARTESIAN_POINT('Ctrl Pts',(-6.32077581368699,-4.76138607988594,
54.8457241851147));
#62950=CARTESIAN_POINT('Ctrl Pts',(-6.43778686188287,-4.60194621603398,
54.8371982221568));
#62951=CARTESIAN_POINT('Ctrl Pts',(-6.66582480445574,-4.26547547627779,
54.8199650076297));
#62952=CARTESIAN_POINT('Ctrl Pts',(-6.77606153115479,-4.08809214991765,
54.8112814047331));
#62953=CARTESIAN_POINT('Ctrl Pts',(-6.90762868687323,-3.85641172438153,
54.8004205113061));
#62954=CARTESIAN_POINT('Ctrl Pts',(-6.93555226552375,-3.80596378835723,
54.7980834234914));
#62955=CARTESIAN_POINT('Ctrl Pts',(-6.9709058180247,-3.74041120160998,54.7950812787241));
#62956=CARTESIAN_POINT('Ctrl Pts',(-6.97884232755549,-3.7255823237436,54.794404423413));
#62957=CARTESIAN_POINT('Ctrl Pts',(-6.99159056556223,-3.70157934882366,
54.793312445532));
#62958=CARTESIAN_POINT('Ctrl Pts',(-6.99643165665369,-3.69242093843017,
54.7928966471493));
#62959=CARTESIAN_POINT('Ctrl Pts',(-7.00563055017833,-3.67493536345932,
54.7921043962801));
#62960=CARTESIAN_POINT('Ctrl Pts',(-7.00999153089272,-3.66660988769852,
54.7917278709205));
#62961=CARTESIAN_POINT('Ctrl Pts',(-7.0198696855995,-3.64766962722157,54.7908728526065));
#62962=CARTESIAN_POINT('Ctrl Pts',(-7.02537764467635,-3.63705004954421,
54.7903945710845));
#62963=CARTESIAN_POINT('Ctrl Pts',(-7.03952710152867,-3.60961722974583,
54.7891619324868));
#62964=CARTESIAN_POINT('Ctrl Pts',(-7.04813247566949,-3.59278540522781,
54.7884084055063));
#62965=CARTESIAN_POINT('Ctrl Pts',(-7.09913965331621,-3.49212853534224,
54.7839186813037));
#62966=CARTESIAN_POINT('Ctrl Pts',(-7.14010652271412,-3.40758343678757,
54.7802157934016));
#62967=CARTESIAN_POINT('Ctrl Pts',(-7.46585600995661,-2.70363793335301,
54.7499235717611));
#62968=CARTESIAN_POINT('Ctrl Pts',(-7.67097718628547,-2.05055992411536,
54.7255615778351));
#62969=CARTESIAN_POINT('Ctrl Pts',(-7.82622536317759,-1.17374586088003,
54.6932538320962));
#62970=CARTESIAN_POINT('Ctrl Pts',(-7.85446598018569,-0.966872766718426,
54.6856307079517));
#62971=CARTESIAN_POINT('Ctrl Pts',(-7.89284770347138,-0.568737706153017,
54.6706510248433));
#62972=CARTESIAN_POINT('Ctrl Pts',(-7.90429036087689,-0.377749577358185,
54.6633297457561));
#62973=CARTESIAN_POINT('Ctrl Pts',(-7.90947036055082,-0.158136250474576,
54.6545964830001));
#62974=CARTESIAN_POINT('Ctrl Pts',(-7.90998734532517,-0.129725193635088,
54.653460612989));
#62975=CARTESIAN_POINT('Ctrl Pts',(-7.91045310642648,-0.0933590609501438,
54.6519983368111));
#62976=CARTESIAN_POINT('Ctrl Pts',(-7.9105429723662,-0.0854057662753664,
54.6516780241876));
#62977=CARTESIAN_POINT('Ctrl Pts',(-7.9106680307464,-0.0726328915355494,
54.65116276784));
#62978=CARTESIAN_POINT('Ctrl Pts',(-7.91071081352397,-0.0678133781019686,
54.6509681573814));
#62979=CARTESIAN_POINT('Ctrl Pts',(-7.91078367967065,-0.0586628668222935,
54.6505982939529));
#62980=CARTESIAN_POINT('Ctrl Pts',(-7.91081461074806,-0.0543318760141865,
54.6504230786353));
#62981=CARTESIAN_POINT('Ctrl Pts',(-7.91087676061146,-0.0444988918204385,
54.6500249139243));
#62982=CARTESIAN_POINT('Ctrl Pts',(-7.91090579612882,-0.0389968909106522,
54.6498018669501));
#62983=CARTESIAN_POINT('Ctrl Pts',(-7.91097620417129,-0.0223676890769472,
54.6491269481663));
#62984=CARTESIAN_POINT('Ctrl Pts',(-7.91099983988053,-0.0112404600942861,
54.648674274225));
#62985=CARTESIAN_POINT('Ctrl Pts',(-7.91100139378223,0.0972945637295643,
54.6442482693096));
#62986=CARTESIAN_POINT('Ctrl Pts',(-7.90920388637905,0.194682414279019,
54.6401883349836));
#62987=CARTESIAN_POINT('Ctrl Pts',(-7.89916025783172,0.466590621048157,
54.628612833795));
#62988=CARTESIAN_POINT('Ctrl Pts',(-7.88693120459857,0.640897614751237,
54.620928536967));
#62989=CARTESIAN_POINT('Ctrl Pts',(-7.80809395681931,1.40241207555216,54.5866014928774));
#62990=CARTESIAN_POINT('Ctrl Pts',(-7.6815849677591,1.98151717405071,54.5586767167013));
#62991=CARTESIAN_POINT('Ctrl Pts',(-7.42074431963833,2.75051765220838,54.5223541201694));
#62992=CARTESIAN_POINT('Ctrl Pts',(-7.34098473291401,2.95681351732233,54.5126687284206));
#62993=CARTESIAN_POINT('Ctrl Pts',(-7.17904591430735,3.32854580044242,54.4954035306613));
#62994=CARTESIAN_POINT('Ctrl Pts',(-7.0995176153692,3.4949639688742,54.4877456364344));
#62995=CARTESIAN_POINT('Ctrl Pts',(-7.00571124286028,3.67481581921132,54.4795473328018));
#62996=CARTESIAN_POINT('Ctrl Pts',(-6.99712276538628,3.69114268698732,54.4788037945686));
#62997=CARTESIAN_POINT('Ctrl Pts',(-6.98494621866495,3.71409532607323,54.4777594796682));
#62998=CARTESIAN_POINT('Ctrl Pts',(-6.98140570698104,3.72074617835415,54.4774569892371));
#62999=CARTESIAN_POINT('Ctrl Pts',(-6.97523305518618,3.73230167714746,54.4769316257539));
#63000=CARTESIAN_POINT('Ctrl Pts',(-6.9726052329809,3.73720861721454,54.4767085968184));
#63001=CARTESIAN_POINT('Ctrl Pts',(-6.96711529483525,3.74743404830302,54.4762439615806));
#63002=CARTESIAN_POINT('Ctrl Pts',(-6.96425226205133,3.75275204465178,54.476002388677));
#63003=CARTESIAN_POINT('Ctrl Pts',(-6.95747641027568,3.76530352477339,54.4754324005983));
#63004=CARTESIAN_POINT('Ctrl Pts',(-6.9535583929155,3.77253420263692,54.4751041742924));
#63005=CARTESIAN_POINT('Ctrl Pts',(-6.94063027685553,3.79630439988731,54.4740255936312));
#63006=CARTESIAN_POINT('Ctrl Pts',(-6.93157235509077,3.81281791188241,54.473276979358));
#63007=CARTESIAN_POINT('Ctrl Pts',(-6.79315143912481,4.06304977760698,54.4619432880323));
#63008=CARTESIAN_POINT('Ctrl Pts',(-6.6520856600882,4.29011100597494,54.4518029210906));
#63009=CARTESIAN_POINT('Ctrl Pts',(-6.30205851439357,4.79461171703886,54.4293335472646));
#63010=CARTESIAN_POINT('Ctrl Pts',(-6.08578840830188,5.06630437406255,54.4172875773013));
#63011=CARTESIAN_POINT('Ctrl Pts',(-5.54891953301019,5.65657266600778,54.3900555011515));
#63012=CARTESIAN_POINT('Ctrl Pts',(-5.21750374315478,5.96363479823766,54.3750734310482));
#63013=CARTESIAN_POINT('Ctrl Pts',(-4.78790630533758,6.29830432492145,54.3555834466411));
#63014=CARTESIAN_POINT('Ctrl Pts',(-4.71304484278565,6.35451742239266,54.3521830055718));
#63015=CARTESIAN_POINT('Ctrl Pts',(-4.61844990458297,6.42295705860252,54.3478587710352));
#63016=CARTESIAN_POINT('Ctrl Pts',(-4.59963516703533,6.43644414359359,54.3469973593468));
#63017=CARTESIAN_POINT('Ctrl Pts',(-4.55845615084983,6.46568998733497,54.3451085296948));
#63018=CARTESIAN_POINT('Ctrl Pts',(-4.53606883258644,6.48141566419631,54.3440794215045));
#63019=CARTESIAN_POINT('Ctrl Pts',(-4.50113396791089,6.50568554640207,54.3424693579879));
#63020=CARTESIAN_POINT('Ctrl Pts',(-4.48864251060131,6.51431038815002,54.3418928350978));
#63021=CARTESIAN_POINT('Ctrl Pts',(-4.47246666620241,6.52541053268169,54.3411451041064));
#63022=CARTESIAN_POINT('Ctrl Pts',(-4.46880485544798,6.52791880036227,54.3409757596515));
#63023=CARTESIAN_POINT('Ctrl Pts',(-4.38439703140805,6.58563217884506,54.3370704168385));
#63024=CARTESIAN_POINT('Ctrl Pts',(-4.30263918899262,6.63933604256428,54.333249549241));
#63025=CARTESIAN_POINT('Ctrl Pts',(-4.21212501950866,6.69641758896424,54.3289552114098));
#63026=CARTESIAN_POINT('Ctrl Pts',(-4.2043316587103,6.70131337933255,54.3285849506606));
#63027=CARTESIAN_POINT('Ctrl Pts',(-4.19278990924557,6.70853584926152,54.3280358193725));
#63028=CARTESIAN_POINT('Ctrl Pts',(-4.18904806790678,6.71087302431279,54.3278576688444));
#63029=CARTESIAN_POINT('Ctrl Pts',(-4.18265607223728,6.71485807148709,54.3275531321573));
#63030=CARTESIAN_POINT('Ctrl Pts',(-4.18000689312152,6.71650750854074,54.3274268541708));
#63031=CARTESIAN_POINT('Ctrl Pts',(-4.17484480726642,6.71971729945578,54.3271806724549));
#63032=CARTESIAN_POINT('Ctrl Pts',(-4.17233200835366,6.72127780718651,54.3270607803698));
#63033=CARTESIAN_POINT('Ctrl Pts',(-4.16629971214822,6.7250193198404,54.3267728313904));
#63034=CARTESIAN_POINT('Ctrl Pts',(-4.16277937927967,6.72719897007644,54.3266046815977));
#63035=CARTESIAN_POINT('Ctrl Pts',(-4.15215023733279,6.73376857440024,54.326096655016));
#63036=CARTESIAN_POINT('Ctrl Pts',(-4.14503620344684,6.73815001896247,54.3257562005799));
#63037=CARTESIAN_POINT('Ctrl Pts',(-4.08034280503776,6.77785265155747,54.3226563459042));
#63038=CARTESIAN_POINT('Ctrl Pts',(-4.02232174770383,6.81244531857652,54.3198486142397));
#63039=CARTESIAN_POINT('Ctrl Pts',(-3.86989094279651,6.90069974314022,54.3124166351989));
#63040=CARTESIAN_POINT('Ctrl Pts',(-3.77480844072638,6.95316707137615,54.307726125373));
#63041=CARTESIAN_POINT('Ctrl Pts',(-3.5125096643223,7.09093981235793,54.2947053308149));
#63042=CARTESIAN_POINT('Ctrl Pts',(-3.34329192713029,7.17227613945592,54.2862181017761));
#63043=CARTESIAN_POINT('Ctrl Pts',(-2.71430949998211,7.44750473671709,54.2547718989931));
#63044=CARTESIAN_POINT('Ctrl Pts',(-2.239339324259,7.60382884953763,54.231304310802));
#63045=CARTESIAN_POINT('Ctrl Pts',(-1.56151033566278,7.75784059404436,54.2001202101018));
#63046=CARTESIAN_POINT('Ctrl Pts',(-1.36865451119107,7.79417710300998,54.1914845072642));
#63047=CARTESIAN_POINT('Ctrl Pts',(-0.963286642336671,7.85504146375148,
54.1738878755487));
#63048=CARTESIAN_POINT('Ctrl Pts',(-0.750726622021704,7.87819882917556,
54.1649747842295));
#63049=CARTESIAN_POINT('Ctrl Pts',(-0.518440318842779,7.89401702015003,
54.1555702635607));
#63050=CARTESIAN_POINT('Ctrl Pts',(-0.4993988475509,7.89524451024308,54.1548017542104));
#63051=CARTESIAN_POINT('Ctrl Pts',(-0.472758356611746,7.89686510134103,
54.1537299031472));
#63052=CARTESIAN_POINT('Ctrl Pts',(-0.465163005852263,7.89731614353443,
54.153424693541));
#63053=CARTESIAN_POINT('Ctrl Pts',(-0.452020716693898,7.89807755952089,
54.1528972439245));
#63054=CARTESIAN_POINT('Ctrl Pts',(-0.446474086565619,7.89839304888848,
54.1526748390884));
#63055=CARTESIAN_POINT('Ctrl Pts',(-0.43497060420794,7.89903520463919,54.1522139990201));
#63056=CARTESIAN_POINT('Ctrl Pts',(-0.429013704269862,7.89936097620649,
54.1519755927668));
#63057=CARTESIAN_POINT('Ctrl Pts',(-0.415053910109282,7.90010857366783,
54.1514174390923));
#63058=CARTESIAN_POINT('Ctrl Pts',(-0.407050725320346,7.90052497822478,
54.1510978665853));
#63059=CARTESIAN_POINT('Ctrl Pts',(-0.381176740330629,7.9018317781422,54.1500660474147));
#63060=CARTESIAN_POINT('Ctrl Pts',(-0.363303488125574,7.9026737082129,54.1493553625864));
#63061=CARTESIAN_POINT('Ctrl Pts',(0.0630626495372903,7.92130841543808,
54.1324509563313));
#63062=CARTESIAN_POINT('Ctrl Pts',(0.472336952076169,7.9074679656097,54.1173449989784));
#63063=CARTESIAN_POINT('Ctrl Pts',(1.3219132479206,7.81251035575637,54.087116533106));
#63064=CARTESIAN_POINT('Ctrl Pts',(1.76008875075446,7.72559743536786,54.0721723812568));
#63065=CARTESIAN_POINT('Ctrl Pts',(2.56974624454654,7.492505065984,54.0430045594239));
#63066=CARTESIAN_POINT('Ctrl Pts',(2.94205885645191,7.35428138251562,54.0289021492482));
#63067=CARTESIAN_POINT('Ctrl Pts',(3.32536579388838,7.17819631233874,54.0121623010053));
#63068=CARTESIAN_POINT('Ctrl Pts',(3.34828475148504,7.1675343847979,54.0111525553832));
#63069=CARTESIAN_POINT('Ctrl Pts',(3.37714670378542,7.15393912831975,54.0098693391469));
#63070=CARTESIAN_POINT('Ctrl Pts',(3.38313786960205,7.15110782088136,54.0096023332876));
#63071=CARTESIAN_POINT('Ctrl Pts',(3.39262832704831,7.14660822086276,54.0091783599521));
#63072=CARTESIAN_POINT('Ctrl Pts',(3.3961299375109,7.14494488960087,54.0090217113406));
#63073=CARTESIAN_POINT('Ctrl Pts',(3.40265850190072,7.14183781433899,54.008729242071));
#63074=CARTESIAN_POINT('Ctrl Pts',(3.40568576466494,7.14039471732286,54.0085934624138));
#63075=CARTESIAN_POINT('Ctrl Pts',(3.41240562783139,7.13718611103132,54.0082917004765));
#63076=CARTESIAN_POINT('Ctrl Pts',(3.41609777544479,7.13541966115768,54.0081256589838));
#63077=CARTESIAN_POINT('Ctrl Pts',(3.42677648790989,7.13030041129808,54.0076447242336));
#63078=CARTESIAN_POINT('Ctrl Pts',(3.43375948253413,7.12694021784625,54.0073293690345));
#63079=CARTESIAN_POINT('Ctrl Pts',(3.48122845167115,7.10401235057283,54.0051798296094));
#63080=CARTESIAN_POINT('Ctrl Pts',(3.5215511694137,7.08411040434333,54.0033250721157));
#63081=CARTESIAN_POINT('Ctrl Pts',(3.64159235850062,7.0235839383093,53.9977220212574));
#63082=CARTESIAN_POINT('Ctrl Pts',(3.72079180005881,6.98195055737766,53.9939170533948));
#63083=CARTESIAN_POINT('Ctrl Pts',(3.95807439182758,6.85203247401155,53.9822268946967));
#63084=CARTESIAN_POINT('Ctrl Pts',(4.11384480221491,6.75965805012074,53.9741564195072));
#63085=CARTESIAN_POINT('Ctrl Pts',(4.66141019158781,6.40900211585848,53.9446984926822));
#63086=CARTESIAN_POINT('Ctrl Pts',(5.03322842158587,6.12133028790897,53.9226780181487));
#63087=CARTESIAN_POINT('Ctrl Pts',(5.72872561091578,5.47677844320272,53.8796468509303));
#63088=CARTESIAN_POINT('Ctrl Pts',(6.04981130166447,5.11989115546819,53.8587703798929));
#63089=CARTESIAN_POINT('Ctrl Pts',(6.35667546462409,4.70932218796625,53.8379354926226));
#63090=CARTESIAN_POINT('Ctrl Pts',(6.376518142503,4.68241976401718,53.8365833034318));
#63091=CARTESIAN_POINT('Ctrl Pts',(6.4026258039801,4.64654962589455,53.8347974171092));
#63092=CARTESIAN_POINT('Ctrl Pts',(6.40904341252182,4.63769373173109,53.8343578719279));
#63093=CARTESIAN_POINT('Ctrl Pts',(6.41899593857839,4.62389976315787,53.8336753527245));
#63094=CARTESIAN_POINT('Ctrl Pts',(6.42254355787134,4.61897089476357,53.8334318937847));
#63095=CARTESIAN_POINT('Ctrl Pts',(6.42961224410748,4.60912615946927,53.8329464524287));
#63096=CARTESIAN_POINT('Ctrl Pts',(6.43313335727791,4.60421033090008,53.8327044683241));
#63097=CARTESIAN_POINT('Ctrl Pts',(6.4410235796382,4.59316806449455,53.8321618341848));
#63098=CARTESIAN_POINT('Ctrl Pts',(6.44538959361138,4.58703941656409,53.831861301918));
#63099=CARTESIAN_POINT('Ctrl Pts',(6.45813461694831,4.56909488756851,53.8309832134038));
#63100=CARTESIAN_POINT('Ctrl Pts',(6.46648994586387,4.55726218305472,53.8304065550506));
#63101=CARTESIAN_POINT('Ctrl Pts',(6.52719175045507,4.47079405004421,53.8262096622014));
#63102=CARTESIAN_POINT('Ctrl Pts',(6.57827811890939,4.39528033877656,53.822637098113));
#63103=CARTESIAN_POINT('Ctrl Pts',(6.73780986071604,4.15045307413853,53.8113351755653));
#63104=CARTESIAN_POINT('Ctrl Pts',(6.84111286162604,3.97787925983614,53.803792237628));
#63105=CARTESIAN_POINT('Ctrl Pts',(7.17577841544393,3.36712299310398,53.7782987806675));
#63106=CARTESIAN_POINT('Ctrl Pts',(7.37249837230412,2.91128668839764,53.7614063117358));
#63107=CARTESIAN_POINT('Ctrl Pts',(7.6617425154968,2.01923996278327,53.7288011478788));
#63108=CARTESIAN_POINT('Ctrl Pts',(7.7626401538392,1.58775562584783,53.7131765404564));
#63109=CARTESIAN_POINT('Ctrl Pts',(7.83102565803567,1.12238408748307,53.6945249145642));
#63110=CARTESIAN_POINT('Ctrl Pts',(7.83495871367955,1.0945916207366,53.6934042014381));
#63111=CARTESIAN_POINT('Ctrl Pts',(7.83970063798375,1.05974773550727,53.6919899806515));
#63112=CARTESIAN_POINT('Ctrl Pts',(7.84064807983595,1.0527150819112,53.6917040767372));
#63113=CARTESIAN_POINT('Ctrl Pts',(7.84212129303695,1.04166742391493,53.6912542013861));
#63114=CARTESIAN_POINT('Ctrl Pts',(7.84265344815074,1.03765326041308,53.6910905845958));
#63115=CARTESIAN_POINT('Ctrl Pts',(7.84358621813709,1.03057546304203,53.6908018191059));
#63116=CARTESIAN_POINT('Ctrl Pts',(7.84398811960136,1.02751200765785,53.6906767427893));
#63117=CARTESIAN_POINT('Ctrl Pts',(7.84490749495456,1.0204721822949,53.6903891077557));
#63118=CARTESIAN_POINT('Ctrl Pts',(7.84542373860193,1.01649566693804,53.6902264809888));
#63119=CARTESIAN_POINT('Ctrl Pts',(7.84684738297746,1.00546394646195,53.6897748971894));
#63120=CARTESIAN_POINT('Ctrl Pts',(7.84774828983688,0.998407921708941,53.6894855802659));
#63121=CARTESIAN_POINT('Ctrl Pts',(7.85263788064273,0.959696458744219,53.6878957150061));
#63122=CARTESIAN_POINT('Ctrl Pts',(7.85644450044818,0.928018715253356,53.6865852392076));
#63123=CARTESIAN_POINT('Ctrl Pts',(7.92026897711992,0.368325073013722,53.6632747814623));
#63124=CARTESIAN_POINT('Ctrl Pts',(7.92712024046717,-0.164357049041584,
53.6387148386669));
#63125=CARTESIAN_POINT('Ctrl Pts',(7.85654579817689,-0.966144067404371,
53.6017567592807));
#63126=CARTESIAN_POINT('Ctrl Pts',(7.81844345881557,-1.23721369436539,53.5892470523026));
#63127=CARTESIAN_POINT('Ctrl Pts',(7.72253631184899,-1.73187737823185,53.5667313754097));
#63128=CARTESIAN_POINT('Ctrl Pts',(7.66884339775479,-1.95596973967448,53.5566511928367));
#63129=CARTESIAN_POINT('Ctrl Pts',(7.55492458046071,-2.35387496549663,53.5390551539159));
#63130=CARTESIAN_POINT('Ctrl Pts',(7.49827564471101,-2.52853337112462,53.5314385790942));
#63131=CARTESIAN_POINT('Ctrl Pts',(7.42969323098445,-2.71732933217363,53.5233204662122));
#63132=CARTESIAN_POINT('Ctrl Pts',(7.42373394927293,-2.73356808244131,53.5226231363781));
#63133=CARTESIAN_POINT('Ctrl Pts',(7.41483133141846,-2.7575834457663,53.5215932140294));
#63134=CARTESIAN_POINT('Ctrl Pts',(7.41192893743517,-2.76537512115204,53.5212592718277));
#63135=CARTESIAN_POINT('Ctrl Pts',(7.4069510193809,-2.7786745471853,53.5206896322138));
#63136=CARTESIAN_POINT('Ctrl Pts',(7.40488162544707,-2.78418457649695,53.5204537324379));
#63137=CARTESIAN_POINT('Ctrl Pts',(7.4008534483558,-2.79487386071654,53.5199962973385));
#63138=CARTESIAN_POINT('Ctrl Pts',(7.3988953730365,-2.80005337813129,53.51977473875));
#63139=CARTESIAN_POINT('Ctrl Pts',(7.39421482738385,-2.81239520638055,53.5192470254165));
#63140=CARTESIAN_POINT('Ctrl Pts',(7.39148738407393,-2.81955563198677,53.5189410356066));
#63141=CARTESIAN_POINT('Ctrl Pts',(7.38333736115095,-2.84085899647557,53.5180311902216));
#63142=CARTESIAN_POINT('Ctrl Pts',(7.37788454782948,-2.85499037276248,53.5174283379661));
#63143=CARTESIAN_POINT('Ctrl Pts',(7.33271992907483,-2.97104437362298,53.5124829437925));
#63144=CARTESIAN_POINT('Ctrl Pts',(7.29093783803178,-3.07215117576059,53.5082098766322));
#63145=CARTESIAN_POINT('Ctrl Pts',(7.11722107459119,-3.46899678306391,53.4915539112372));
#63146=CARTESIAN_POINT('Ctrl Pts',(6.96927564021247,-3.75739183977866,53.4797247739583));
#63147=CARTESIAN_POINT('Ctrl Pts',(6.64558138941399,-4.30309985339854,53.4572738053077));
#63148=CARTESIAN_POINT('Ctrl Pts',(6.47150008237445,-4.56071392238005,53.4466391962093));
#63149=CARTESIAN_POINT('Ctrl Pts',(6.01997632535334,-5.15080069639834,53.4210911927234));
#63150=CARTESIAN_POINT('Ctrl Pts',(5.72954266995674,-5.47203302482016,53.4061854269505));
#63151=CARTESIAN_POINT('Ctrl Pts',(5.40201028312265,-5.77948894587036,53.3890880750929));
#63152=CARTESIAN_POINT('Ctrl Pts',(5.38963063290485,-5.79103524501524,53.3884414177846));
#63153=CARTESIAN_POINT('Ctrl Pts',(5.3678184195355,-5.81124861838055,53.3873010956351));
#63154=CARTESIAN_POINT('Ctrl Pts',(5.35840165976526,-5.81993270919212,53.3868084874449));
#63155=CARTESIAN_POINT('Ctrl Pts',(5.28992254482219,-5.88277673681315,53.3832236397932));
#63156=CARTESIAN_POINT('Ctrl Pts',(5.23006311297005,-5.93605775906779,53.3800761611036));
#63157=CARTESIAN_POINT('Ctrl Pts',(5.16198390594688,-5.99482604457503,53.3764680886912));
#63158=CARTESIAN_POINT('Ctrl Pts',(5.15454944248595,-6.00121964215105,53.3760737019837));
#63159=CARTESIAN_POINT('Ctrl Pts',(5.14397392694059,-6.01028037771302,53.375512126942));
#63160=CARTESIAN_POINT('Ctrl Pts',(5.14084262287012,-6.01295893105309,53.3753457806313));
#63161=CARTESIAN_POINT('Ctrl Pts',(5.13509905765693,-6.01786427651866,53.3750405311192));
#63162=CARTESIAN_POINT('Ctrl Pts',(5.13248743573662,-6.02009181860882,53.374901683641));
#63163=CARTESIAN_POINT('Ctrl Pts',(5.12719691676145,-6.02459833906063,53.3746203103493));
#63164=CARTESIAN_POINT('Ctrl Pts',(5.12451794823885,-6.02687723189729,53.374477778232));
#63165=CARTESIAN_POINT('Ctrl Pts',(5.11792432965599,-6.0324785883757,53.3741268387473));
#63166=CARTESIAN_POINT('Ctrl Pts',(5.11400798976526,-6.03579900624991,53.373918280347));
#63167=CARTESIAN_POINT('Ctrl Pts',(5.09944612203629,-6.04812074933684,53.3731423803979));
#63168=CARTESIAN_POINT('Ctrl Pts',(5.08878012974753,-6.05709766608196,53.3725732160128));
#63169=CARTESIAN_POINT('Ctrl Pts',(4.82807335440149,-6.27534404011813,53.3586418954421));
#63170=CARTESIAN_POINT('Ctrl Pts',(4.56537686471979,-6.46896667355995,53.3441806890438));
#63171=CARTESIAN_POINT('Ctrl Pts',(4.01111413607448,-6.82688029823039,53.3141243232239));
#63172=CARTESIAN_POINT('Ctrl Pts',(3.71953711401065,-6.9900196176755,53.2985455209948));
#63173=CARTESIAN_POINT('Ctrl Pts',(2.89880342900438,-7.38329152675879,53.2566522391708));
#63174=CARTESIAN_POINT('Ctrl Pts',(2.35335763240726,-7.57482331444368,53.2310240059406));
#63175=CARTESIAN_POINT('Ctrl Pts',(1.75265460559258,-7.71451513144251,53.2059054740924));
#63176=CARTESIAN_POINT('Ctrl Pts',(1.71337138506902,-7.72333480052468,53.2042756314812));
#63177=CARTESIAN_POINT('Ctrl Pts',(1.66292521790088,-7.73425688957956,53.2021988056117));
#63178=CARTESIAN_POINT('Ctrl Pts',(1.65182309670722,-7.73663559778787,53.2017427413106));
#63179=CARTESIAN_POINT('Ctrl Pts',(1.63412205955062,-7.74038833179083,53.2010171866495));
#63180=CARTESIAN_POINT('Ctrl Pts',(1.62752646252181,-7.74177783500172,53.2007471878776));
#63181=CARTESIAN_POINT('Ctrl Pts',(1.61518925979152,-7.7443604671018,53.2002428032749));
#63182=CARTESIAN_POINT('Ctrl Pts',(1.60944809036837,-7.74555564397812,53.2000083503237));
#63183=CARTESIAN_POINT('Ctrl Pts',(1.59665533552149,-7.74820395806832,53.19948651846));
#63184=CARTESIAN_POINT('Ctrl Pts',(1.58960308055271,-7.7496538556851,53.199199246041));
#63185=CARTESIAN_POINT('Ctrl Pts',(1.56906269175149,-7.75384760794976,53.1983636901308));
#63186=CARTESIAN_POINT('Ctrl Pts',(1.55556933227962,-7.75656589689976,53.1978162454392));
#63187=CARTESIAN_POINT('Ctrl Pts',(1.45991495959644,-7.77557619468792,53.1939455916218));
#63188=CARTESIAN_POINT('Ctrl Pts',(1.37750540830707,-7.79059793923101,53.1906641501927));
#63189=CARTESIAN_POINT('Ctrl Pts',(1.11931529864668,-7.83343618984169,53.1805403464521));
#63190=CARTESIAN_POINT('Ctrl Pts',(0.942821423590777,-7.85663297225901,
53.1738474455045));
#63191=CARTESIAN_POINT('Ctrl Pts',(0.698487286303601,-7.88039308502629,
53.1648346432874));
#63192=CARTESIAN_POINT('Ctrl Pts',(0.631204760605771,-7.88606748810711,
53.1623788327571));
#63193=CARTESIAN_POINT('Ctrl Pts',(0.512766192067003,-7.89453072918604,
53.1580960525916));
#63194=CARTESIAN_POINT('Ctrl Pts',(0.461640722211808,-7.89768526391019,
53.1562604792607));
#63195=CARTESIAN_POINT('Ctrl Pts',(0.102699998759804,-7.91633518719077,
53.1434546825544));
#63196=CARTESIAN_POINT('Ctrl Pts',(-0.205765113024291,-7.9143273820681,
53.1328829458629));
#63197=CARTESIAN_POINT('Ctrl Pts',(-1.07041971224426,-7.85810306177393,
53.1032396024818));
#63198=CARTESIAN_POINT('Ctrl Pts',(-1.62204423100101,-7.76301502540086,
53.0843670750515));
#63199=CARTESIAN_POINT('Ctrl Pts',(-2.19360315738441,-7.60087632333886,
53.0609227427606));
#63200=CARTESIAN_POINT('Ctrl Pts',(-2.22815122294207,-7.59082062390545,
53.0594897195736));
#63201=CARTESIAN_POINT('Ctrl Pts',(-2.26916432534553,-7.57857907398771,
53.0577682496949));
#63202=CARTESIAN_POINT('Ctrl Pts',(-2.27569714609764,-7.57661995977173,
53.0574934294246));
#63203=CARTESIAN_POINT('Ctrl Pts',(-2.28627967858125,-7.5734314642,53.0570472400486));
#63204=CARTESIAN_POINT('Ctrl Pts',(-2.29033096223412,-7.57220727363559,
53.0568761870642));
#63205=CARTESIAN_POINT('Ctrl Pts',(-2.29751496473137,-7.57003016565,53.0565724366728));
#63206=CARTESIAN_POINT('Ctrl Pts',(-2.30064808102345,-7.56907855219083,
53.0564398193403));
#63207=CARTESIAN_POINT('Ctrl Pts',(-2.30722503698683,-7.56707648912086,
53.0561611273542));
#63208=CARTESIAN_POINT('Ctrl Pts',(-2.3106687403075,-7.56602563674595,53.0560150278176));
#63209=CARTESIAN_POINT('Ctrl Pts',(-2.31976697874516,-7.56324250166316,
53.0556285703246));
#63210=CARTESIAN_POINT('Ctrl Pts',(-2.32542028228102,-7.56150623123615,
53.0553879669446));
#63211=CARTESIAN_POINT('Ctrl Pts',(-2.35099484507061,-7.5536202522019,53.0542973946147));
#63212=CARTESIAN_POINT('Ctrl Pts',(-2.37089352503012,-7.54739819758797,
53.0534430216105));
#63213=CARTESIAN_POINT('Ctrl Pts',(-2.51800736355599,-7.50075844345554,
53.0470845300441));
#63214=CARTESIAN_POINT('Ctrl Pts',(-2.64419985437063,-7.45720737089999,
53.0413976549571));
#63215=CARTESIAN_POINT('Ctrl Pts',(-3.01779869987117,-7.31759730086645,
53.0239919044625));
#63216=CARTESIAN_POINT('Ctrl Pts',(-3.26152976506177,-7.21226365561203,
53.0118803527195));
#63217=CARTESIAN_POINT('Ctrl Pts',(-3.59508680838912,-7.04773959719167,
52.9946563558052));
#63218=CARTESIAN_POINT('Ctrl Pts',(-3.68971812254812,-6.99866147430354,
52.9896926528854));
#63219=CARTESIAN_POINT('Ctrl Pts',(-3.88616914120351,-6.89168505301032,
52.9792598173926));
#63220=CARTESIAN_POINT('Ctrl Pts',(-3.98775433606687,-6.83340683129726,
52.9737904063483));
#63221=CARTESIAN_POINT('Ctrl Pts',(-4.48409256518029,-6.53382520938955,
52.946788641531));
#63222=CARTESIAN_POINT('Ctrl Pts',(-4.85847679960628,-6.26045056837409,
52.9256034945241));
#63223=CARTESIAN_POINT('Ctrl Pts',(-5.3769776025157,-5.80715928738465,52.8959088128475));
#63224=CARTESIAN_POINT('Ctrl Pts',(-5.54066492631449,-5.65119728822662,
52.886459357009));
#63225=CARTESIAN_POINT('Ctrl Pts',(-5.71098955644581,-5.47438577363508,
52.8765319542371));
#63226=CARTESIAN_POINT('Ctrl Pts',(-5.7244673050893,-5.46029077912868,52.8757456889945));
#63227=CARTESIAN_POINT('Ctrl Pts',(-5.74320502269232,-5.44054929301917,
52.8746515346896));
#63228=CARTESIAN_POINT('Ctrl Pts',(-5.74850900211401,-5.43494478311402,
52.8743417022937));
#63229=CARTESIAN_POINT('Ctrl Pts',(-5.75765706129074,-5.42525001003886,
52.8738071134581));
#63230=CARTESIAN_POINT('Ctrl Pts',(-5.76150499894516,-5.42116340411987,
52.8735821873183));
#63231=CARTESIAN_POINT('Ctrl Pts',(-5.76946234814722,-5.41269445889231,
52.8731169196789));
#63232=CARTESIAN_POINT('Ctrl Pts',(-5.77357112450705,-5.40831152602033,
52.8728766060831));
#63233=CARTESIAN_POINT('Ctrl Pts',(-5.78316402911962,-5.39805514839312,
52.8723153653332));
#63234=CARTESIAN_POINT('Ctrl Pts',(-5.78864421347987,-5.39217801477691,
52.8719946107387));
#63235=CARTESIAN_POINT('Ctrl Pts',(-5.80623464543317,-5.37325572400189,
52.870964613048));
#63236=CARTESIAN_POINT('Ctrl Pts',(-5.81830986357289,-5.36017799799626,
52.8702568959081));
#63237=CARTESIAN_POINT('Ctrl Pts',(-6.0688096175932,-5.08703741676485,52.8555610459253));
#63238=CARTESIAN_POINT('Ctrl Pts',(-6.28962674410215,-4.81134367714607,
52.8423619123879));
#63239=CARTESIAN_POINT('Ctrl Pts',(-6.61278549892338,-4.34743028797965,
52.8220501574856));
#63240=CARTESIAN_POINT('Ctrl Pts',(-6.72718047041968,-4.1682285009271,52.8146070437094));
#63241=CARTESIAN_POINT('Ctrl Pts',(-6.88317394012459,-3.9006771859441,52.8038761104926));
#63242=CARTESIAN_POINT('Ctrl Pts',(-6.93057345379505,-3.8158246466999,52.8005258083642));
#63243=CARTESIAN_POINT('Ctrl Pts',(-7.01962318096328,-3.64927603782986,
52.7940227074274));
#63244=CARTESIAN_POINT('Ctrl Pts',(-7.06144007828467,-3.56768681235174,
52.7908699696546));
#63245=CARTESIAN_POINT('Ctrl Pts',(-7.31670804373829,-3.04755280095899,
52.7708917995774));
#63246=CARTESIAN_POINT('Ctrl Pts',(-7.4906257351634,-2.59080444162496,52.7539208301729));
#63247=CARTESIAN_POINT('Ctrl Pts',(-7.62995306471455,-2.09015823298453,
52.7333427922374));
#63248=CARTESIAN_POINT('Ctrl Pts',(-7.63834607804533,-2.05927520108679,
52.7320660303111));
#63249=CARTESIAN_POINT('Ctrl Pts',(-7.64875762255149,-2.02002521652862,
52.7304347182502));
#63250=CARTESIAN_POINT('Ctrl Pts',(-7.65095029426418,-2.01170441113285,
52.7300883962383));
#63251=CARTESIAN_POINT('Ctrl Pts',(-7.65439977852426,-1.99852700673814,
52.7295391753409));
#63252=CARTESIAN_POINT('Ctrl Pts',(-7.65566555909101,-1.99367274478783,
52.7293366912091));
#63253=CARTESIAN_POINT('Ctrl Pts',(-7.65799945232955,-1.98468727911223,
52.7289615851987));
#63254=CARTESIAN_POINT('Ctrl Pts',(-7.65906884212541,-1.98055640647481,
52.7287890217172));
#63255=CARTESIAN_POINT('Ctrl Pts',(-7.66143437093945,-1.97138819985877,
52.7284057722394));
#63256=CARTESIAN_POINT('Ctrl Pts',(-7.66272888445041,-1.96635045146487,
52.7281950128939));
#63257=CARTESIAN_POINT('Ctrl Pts',(-7.66641950164567,-1.9519289997621,52.7275911932014));
#63258=CARTESIAN_POINT('Ctrl Pts',(-7.66880333801117,-1.9425421892554,52.7271975860729));
#63259=CARTESIAN_POINT('Ctrl Pts',(-7.67410921618356,-1.92148729396025,
52.7263134348816));
#63260=CARTESIAN_POINT('Ctrl Pts',(-7.67702189196768,-1.90981688933012,
52.725822484112));
#63261=CARTESIAN_POINT('Ctrl Pts',(-7.68610790668835,-1.87305471216532,
52.7242732952206));
#63262=CARTESIAN_POINT('Ctrl Pts',(-7.69218489282864,-1.84793946362036,
52.7232109958669));
#63263=CARTESIAN_POINT('Ctrl Pts',(-7.83953709636964,-1.22563271150984,
52.6967992752754));
#63264=CARTESIAN_POINT('Ctrl Pts',(-7.91096660799007,-0.61407003492305,
52.6689754571467));
#63265=CARTESIAN_POINT('Ctrl Pts',(-7.91099998829544,-0.000430336557561556,
52.6419314571579));
#63266=CARTESIAN_POINT('',(-7.911,2.06501482580279E-13,50.642331508237));
#63267=CARTESIAN_POINT('Ctrl Pts',(-7.911,1.51545442861334E-13,52.642331508237));
#63268=CARTESIAN_POINT('Ctrl Pts',(-7.91099999999996,2.20167589666687,52.5537440725043));
#63269=CARTESIAN_POINT('Ctrl Pts',(-6.94214576672367,4.38610418338687,52.4651566367716));
#63270=CARTESIAN_POINT('Ctrl Pts',(-3.67820201488288,7.3418068410763,52.2879817653061));
#63271=CARTESIAN_POINT('Ctrl Pts',(-1.40868175871752,8.08992666571334,52.1993943295734));
#63272=CARTESIAN_POINT('Ctrl Pts',(2.97309270521258,7.65454228025262,52.022219458108));
#63273=CARTESIAN_POINT('Ctrl Pts',(5.05102072675584,6.47444880834238,51.9336320223752));
#63274=CARTESIAN_POINT('Ctrl Pts',(7.66951518847859,2.93425195367736,51.7564571509098));
#63275=CARTESIAN_POINT('Ctrl Pts',(8.18956872247067,0.601881960099537,51.6678697151771));
#63276=CARTESIAN_POINT('Ctrl Pts',(7.32306689761363,-3.71537198232408,51.4906948437116));
#63277=CARTESIAN_POINT('Ctrl Pts',(5.94329958850236,-5.66643518936472,51.4021074079789));
#63278=CARTESIAN_POINT('Ctrl Pts',(2.16154501637906,-7.9220591323298,51.2249325365134));
#63279=CARTESIAN_POINT('Ctrl Pts',(-0.210816529299704,-8.20894963713003,
51.1363451007807));
#63280=CARTESIAN_POINT('Ctrl Pts',(-4.42123908576373,-6.91982244717871,
50.9591702293153));
#63281=CARTESIAN_POINT('Ctrl Pts',(-6.22631625634134,-5.35390358803581,
50.8705827935825));
#63282=CARTESIAN_POINT('Ctrl Pts',(-7.65317280859479,-2.31334857514567,
50.7354407413122));
#63283=CARTESIAN_POINT('Ctrl Pts',(-7.91100000000003,-1.15702837836533,
50.6888861247746));
#63284=CARTESIAN_POINT('Ctrl Pts',(-7.911,2.06501482580279E-13,50.642331508237));
#63285=CARTESIAN_POINT('',(-7.91099943894101,0.00297944206225246,48.6425309018316));
#63286=CARTESIAN_POINT('Ctrl Pts',(-7.91099989537763,0.00128659828464795,
50.642331508237));
#63287=CARTESIAN_POINT('Ctrl Pts',(-7.91096572008773,0.211422674174465,
50.6339190564692));
#63288=CARTESIAN_POINT('Ctrl Pts',(-7.90255468055934,0.421350259379313,
50.6255066047014));
#63289=CARTESIAN_POINT('Ctrl Pts',(-7.88584196755081,0.630410551001773,
50.6170941529337));
#63290=CARTESIAN_POINT('Ctrl Pts',(-7.86909991135218,0.839837898282741,
50.6086669310821));
#63291=CARTESIAN_POINT('Ctrl Pts',(-7.84402707863192,1.048394644105,50.6002397092305));
#63292=CARTESIAN_POINT('Ctrl Pts',(-7.81075000739738,1.25543033336855,50.591812487379));
#63293=CARTESIAN_POINT('Ctrl Pts',(-7.77738440477785,1.46301682700379,50.5833628454767));
#63294=CARTESIAN_POINT('Ctrl Pts',(-7.73577093775734,1.66907390387563,50.5749132035745));
#63295=CARTESIAN_POINT('Ctrl Pts',(-7.68608714525271,1.87296166420486,50.5664635616723));
#63296=CARTESIAN_POINT('Ctrl Pts',(-7.63633259403002,2.07713979762805,50.5580018859499));
#63297=CARTESIAN_POINT('Ctrl Pts',(-7.57848482854346,2.27914218659757,50.5495402102274));
#63298=CARTESIAN_POINT('Ctrl Pts',(-7.5127706875228,2.47834573792646,50.5410785345049));
#63299=CARTESIAN_POINT('Ctrl Pts',(-7.4469154620526,2.67797696772681,50.5325986920554));
#63300=CARTESIAN_POINT('Ctrl Pts',(-7.37316017474965,2.87479709133008,50.5241188496059));
#63301=CARTESIAN_POINT('Ctrl Pts',(-7.29178003110565,3.06820223876603,50.5156390071564));
#63302=CARTESIAN_POINT('Ctrl Pts',(-7.26035893702876,3.14287649049904,50.5123649169984));
#63303=CARTESIAN_POINT('Ctrl Pts',(-7.2278016498811,3.21704191783815,50.5090908268404));
#63304=CARTESIAN_POINT('Ctrl Pts',(-7.19412580975778,3.29066480112711,50.5058167366824));
#63305=CARTESIAN_POINT('Ctrl Pts',(-7.10860288381246,3.47763695601159,50.4975018804206));
#63306=CARTESIAN_POINT('Ctrl Pts',(-7.01571379924195,3.66143339218067,50.4891870241587));
#63307=CARTESIAN_POINT('Ctrl Pts',(-6.91570954292541,3.84146879694349,50.4808721678969));
#63308=CARTESIAN_POINT('Ctrl Pts',(-6.81582843837433,4.02128249436345,50.4725675510915));
#63309=CARTESIAN_POINT('Ctrl Pts',(-6.70884977933363,4.19734414270669,50.4642629342861));
#63310=CARTESIAN_POINT('Ctrl Pts',(-6.59507168477514,4.36909034842234,50.4559583174807));
#63311=CARTESIAN_POINT('Ctrl Pts',(-6.48142619905779,4.54063638322284,50.4476633797407));
#63312=CARTESIAN_POINT('Ctrl Pts',(-6.36099724542115,4.70787676367204,50.4393684420007));
#63313=CARTESIAN_POINT('Ctrl Pts',(-6.23412814604646,4.87027383816058,50.4310735042606));
#63314=CARTESIAN_POINT('Ctrl Pts',(-6.10744919986194,5.03242750963024,50.4227909990899));
#63315=CARTESIAN_POINT('Ctrl Pts',(-5.9743495511192,5.1897521316094,50.4145084939192));
#63316=CARTESIAN_POINT('Ctrl Pts',(-5.83521501341863,5.34174004863339,50.4062259887485));
#63317=CARTESIAN_POINT('Ctrl Pts',(-5.69620829060746,5.4935883431084,50.3979510922385));
#63318=CARTESIAN_POINT('Ctrl Pts',(-5.55117793158211,5.64010949349851,50.3896761957284));
#63319=CARTESIAN_POINT('Ctrl Pts',(-5.40055026219762,5.78082847570114,50.3814012992183));
#63320=CARTESIAN_POINT('Ctrl Pts',(-5.25009489111149,5.92138649384398,50.3731358681046));
#63321=CARTESIAN_POINT('Ctrl Pts',(-5.09405519942159,6.05615538767114,50.3648704369908));
#63322=CARTESIAN_POINT('Ctrl Pts',(-4.9328948354957,6.18469639852595,50.3566050058771));
#63323=CARTESIAN_POINT('Ctrl Pts',(-4.86991695643135,6.23492736127152,50.3533750595776));
#63324=CARTESIAN_POINT('Ctrl Pts',(-4.80615751659977,6.28420767292708,50.350145113278));
#63325=CARTESIAN_POINT('Ctrl Pts',(-4.74164569489685,6.33251270066363,50.3469151669785));
#63326=CARTESIAN_POINT('Ctrl Pts',(-4.57653722254991,6.45614227933196,50.3386485968336));
#63327=CARTESIAN_POINT('Ctrl Pts',(-4.40668419390388,6.57324130337467,50.3303820266887));
#63328=CARTESIAN_POINT('Ctrl Pts',(-4.23262855662394,6.68347039356438,50.3221154565438));
#63329=CARTESIAN_POINT('Ctrl Pts',(-4.05841696347715,6.79379825029553,50.3138414794564));
#63330=CARTESIAN_POINT('Ctrl Pts',(-3.87999549225706,6.89724372729374,50.3055675023689));
#63331=CARTESIAN_POINT('Ctrl Pts',(-3.6979315218611,6.99351295556289,50.2972935252814));
#63332=CARTESIAN_POINT('Ctrl Pts',(-3.5156926024737,7.08987469090172,50.2890115975602));
#63333=CARTESIAN_POINT('Ctrl Pts',(-3.32980445543751,7.17904627338473,50.280729669839));
#63334=CARTESIAN_POINT('Ctrl Pts',(-3.14085604662888,7.26078124545526,50.2724477421177));
#63335=CARTESIAN_POINT('Ctrl Pts',(-2.95159443359853,7.34265170285999,50.2641520861268));
#63336=CARTESIAN_POINT('Ctrl Pts',(-2.75926268708295,7.41706078818231,50.2558564301358));
#63337=CARTESIAN_POINT('Ctrl Pts',(-2.56446852670033,7.48381067208167,50.2475607741448));
#63338=CARTESIAN_POINT('Ctrl Pts',(-2.36949831009525,7.55062088495796,50.2392576204863));
#63339=CARTESIAN_POINT('Ctrl Pts',(-2.17206151672117,7.60975798982195,50.2309544668278));
#63340=CARTESIAN_POINT('Ctrl Pts',(-1.97277904660427,7.66107458737214,50.2226513131692));
#63341=CARTESIAN_POINT('Ctrl Pts',(-1.77319274310542,7.71246942409397,50.2143355002173));
#63342=CARTESIAN_POINT('Ctrl Pts',(-1.57175542403136,7.7560198534894,50.2060196872654));
#63343=CARTESIAN_POINT('Ctrl Pts',(-1.36909800993088,7.79162958816725,50.1977038743134));
#63344=CARTESIAN_POINT('Ctrl Pts',(-1.29038025064674,7.80546139656658,50.1944737819672));
#63345=CARTESIAN_POINT('Ctrl Pts',(-1.21147846111171,7.81809569875332,50.1912436896209));
#63346=CARTESIAN_POINT('Ctrl Pts',(-1.13242976097967,7.82952896644795,50.1880135972746));
#63347=CARTESIAN_POINT('Ctrl Pts',(-0.938827999898432,7.85753070154159,
50.1801026314314));
#63348=CARTESIAN_POINT('Ctrl Pts',(-0.743942682173932,7.87838269023725,
50.1721916655883));
#63349=CARTESIAN_POINT('Ctrl Pts',(-0.548344041427492,7.89197312541236,
50.1642806997451));
#63350=CARTESIAN_POINT('Ctrl Pts',(-0.352943328428411,7.90554980832309,
50.1563777390682));
#63351=CARTESIAN_POINT('Ctrl Pts',(-0.156831071094351,7.91187955087205,
50.1484747783913));
#63352=CARTESIAN_POINT('Ctrl Pts',(0.0394138177652493,7.91090181654211,
50.1405718177144));
#63353=CARTESIAN_POINT('Ctrl Pts',(0.235496442323643,7.90992489064788,50.132675391569));
#63354=CARTESIAN_POINT('Ctrl Pts',(0.431711137372738,7.90165252663699,50.1247789654235));
#63355=CARTESIAN_POINT('Ctrl Pts',(0.627475108132371,7.88607608311474,50.1168825392781));
#63356=CARTESIAN_POINT('Ctrl Pts',(0.823113430771456,7.87050963709532,50.1089911813333));
#63357=CARTESIAN_POINT('Ctrl Pts',(1.01830126333165,7.84764847933911,50.1010998233886));
#63358=CARTESIAN_POINT('Ctrl Pts',(1.2124567644762,7.8175360308908,50.0932084654439));
#63359=CARTESIAN_POINT('Ctrl Pts',(1.40652356372339,7.78743733961804,50.0853207127456));
#63360=CARTESIAN_POINT('Ctrl Pts',(1.59955863166727,7.75009401192119,50.0774329600473));
#63361=CARTESIAN_POINT('Ctrl Pts',(1.79098591028883,7.70560123995181,50.069545207349));
#63362=CARTESIAN_POINT('Ctrl Pts',(1.98236113748558,7.66112056611281,50.0616595994274));
#63363=CARTESIAN_POINT('Ctrl Pts',(2.17212911153887,7.60949440070085,50.0537739915058));
#63364=CARTESIAN_POINT('Ctrl Pts',(2.35972433844907,7.55086895969802,50.0458883835842));
#63365=CARTESIAN_POINT('Ctrl Pts',(2.54734169058909,7.49223660433294,50.0380018456236));
#63366=CARTESIAN_POINT('Ctrl Pts',(2.73278545268314,7.42660342019414,50.0301153076629));
#63367=CARTESIAN_POINT('Ctrl Pts',(2.91550504660686,7.35416557627104,50.0222287697023));
#63368=CARTESIAN_POINT('Ctrl Pts',(3.09824765974582,7.28171860654875,50.0143412381869));
#63369=CARTESIAN_POINT('Ctrl Pts',(3.27826510016409,7.20246539522135,50.0064537066716));
#63370=CARTESIAN_POINT('Ctrl Pts',(3.45502656880677,7.11665036438065,49.9985661751562));
#63371=CARTESIAN_POINT('Ctrl Pts',(3.63183993331962,7.03081013887659,49.9906763279194));
#63372=CARTESIAN_POINT('Ctrl Pts',(3.80539511113926,6.93840440521484,49.9827864806827));
#63373=CARTESIAN_POINT('Ctrl Pts',(3.97518549589906,6.83972377170261,49.9748966334459));
#63374=CARTESIAN_POINT('Ctrl Pts',(4.14505418933691,6.74099762589608,49.9670031473488));
#63375=CARTESIAN_POINT('Ctrl Pts',(4.31115433203221,6.6359909861206,49.9591096612516));
#63376=CARTESIAN_POINT('Ctrl Pts',(4.47300770478048,6.52503816639983,49.9512161751545));
#63377=CARTESIAN_POINT('Ctrl Pts',(4.6350481798038,6.41395708537291,49.9433135641983));
#63378=CARTESIAN_POINT('Ctrl Pts',(4.79283179476898,6.29691628933584,49.9354109532422));
#63379=CARTESIAN_POINT('Ctrl Pts',(4.94591195799857,6.17429153050993,49.927508342286));
#63380=CARTESIAN_POINT('Ctrl Pts',(5.09909365233387,6.05158544026207,49.9196004898876));
#63381=CARTESIAN_POINT('Ctrl Pts',(5.24756541598531,5.92328822837078,49.9116926374893));
#63382=CARTESIAN_POINT('Ctrl Pts',(5.39091686108726,5.78981315733463,49.9037847850909));
#63383=CARTESIAN_POINT('Ctrl Pts',(5.53446445162516,5.65615545454349,49.8958661125076));
#63384=CARTESIAN_POINT('Ctrl Pts',(5.67287748753951,5.51730598466832,49.8879474399242));
#63385=CARTESIAN_POINT('Ctrl Pts',(5.80578448127278,5.37371264183452,49.8800287673408));
#63386=CARTESIAN_POINT('Ctrl Pts',(5.86071464715428,5.31436583155929,49.8767559975162));
#63387=CARTESIAN_POINT('Ctrl Pts',(5.91470479491093,5.25420906129168,49.8734832276917));
#63388=CARTESIAN_POINT('Ctrl Pts',(5.96773084404036,5.19327541856673,49.8702104578671));
#63389=CARTESIAN_POINT('Ctrl Pts',(6.09480679920306,5.04724906024012,49.8623673249482));
#63390=CARTESIAN_POINT('Ctrl Pts',(6.21671907405414,4.89632666671056,49.8545241920293));
#63391=CARTESIAN_POINT('Ctrl Pts',(6.33306274314762,4.74091101913499,49.8466810591104));
#63392=CARTESIAN_POINT('Ctrl Pts',(6.44926977898489,4.58567789069569,49.8388471371163));
#63393=CARTESIAN_POINT('Ctrl Pts',(6.55992102252503,4.42596229358886,49.8310132151222));
#63394=CARTESIAN_POINT('Ctrl Pts',(6.66464900251338,4.26220303051103,49.8231792931282));
#63395=CARTESIAN_POINT('Ctrl Pts',(6.76927435842586,4.09860423689934,49.8153530476786));
#63396=CARTESIAN_POINT('Ctrl Pts',(6.86798782162776,3.93096996202489,49.8075268022291));
#63397=CARTESIAN_POINT('Ctrl Pts',(6.96046265731882,3.7597713489081,49.7997005567796));
#63398=CARTESIAN_POINT('Ctrl Pts',(7.05286485010405,3.58870721956345,49.7918804591779));
#63399=CARTESIAN_POINT('Ctrl Pts',(7.139038009825,3.41408463631659,49.7840603615761));
#63400=CARTESIAN_POINT('Ctrl Pts',(7.21869904997974,3.23640310002039,49.7762402639743));
#63401=CARTESIAN_POINT('Ctrl Pts',(7.29831299034876,3.05882661836908,49.7684247900245));
#63402=CARTESIAN_POINT('Ctrl Pts',(7.37142233751846,2.87819510625526,49.7606093160747));
#63403=CARTESIAN_POINT('Ctrl Pts',(7.43779016705609,2.69503217621678,49.7527938421248));
#63404=CARTESIAN_POINT('Ctrl Pts',(7.50413164753822,2.51194196469634,49.7449814710391));
#63405=CARTESIAN_POINT('Ctrl Pts',(7.56373682338245,2.32632266768829,49.7371690999534));
#63406=CARTESIAN_POINT('Ctrl Pts',(7.61641702412088,2.13871753971432,49.7293567288676));
#63407=CARTESIAN_POINT('Ctrl Pts',(7.66909523072578,1.95111951326369,49.721544653508));
#63408=CARTESIAN_POINT('Ctrl Pts',(7.71484888073255,1.76153614158864,49.7137325781484));
#63409=CARTESIAN_POINT('Ctrl Pts',(7.75353914339565,1.57052594751931,49.7059205027888));
#63410=CARTESIAN_POINT('Ctrl Pts',(7.79223053762832,1.37951016699727,49.6981081989504));
#63411=CARTESIAN_POINT('Ctrl Pts',(7.82385806239047,1.18706782562856,49.6902958951119));
#63412=CARTESIAN_POINT('Ctrl Pts',(7.84833400920573,0.993767719311079,49.6824835912734));
#63413=CARTESIAN_POINT('Ctrl Pts',(7.87281497848729,0.800427947795876,49.6746696843496));
#63414=CARTESIAN_POINT('Ctrl Pts',(7.89014140225767,0.606230409680675,49.6668557774257));
#63415=CARTESIAN_POINT('Ctrl Pts',(7.90027743487255,0.41174925870444,49.6590418705019));
#63416=CARTESIAN_POINT('Ctrl Pts',(7.91041733099552,0.217193978181619,49.6512249851846));
#63417=CARTESIAN_POINT('Ctrl Pts',(7.91336135827729,0.0223552204291192,
49.6434080998674));
#63418=CARTESIAN_POINT('Ctrl Pts',(7.90912578952055,-0.172192466562872,
49.6355912145501));
#63419=CARTESIAN_POINT('Ctrl Pts',(7.90488562606776,-0.36695119663747,49.627765849566));
#63420=CARTESIAN_POINT('Ctrl Pts',(7.89345031880717,-0.561417873584109,
49.6199404845819));
#63421=CARTESIAN_POINT('Ctrl Pts',(7.87488814875403,-0.755021618639716,
49.6121151195978));
#63422=CARTESIAN_POINT('Ctrl Pts',(7.85631469743633,-0.948743027473951,
49.6042849987036));
#63423=CARTESIAN_POINT('Ctrl Pts',(7.83060579755964,-1.14160011168952,49.5964548778093));
#63424=CARTESIAN_POINT('Ctrl Pts',(7.79788095963174,-1.33303170983018,49.5886247569151));
#63425=CARTESIAN_POINT('Ctrl Pts',(7.7651113890189,-1.52472498228031,49.5807839327644));
#63426=CARTESIAN_POINT('Ctrl Pts',(7.72530679730214,-1.71498853379204,49.5729431086138));
#63427=CARTESIAN_POINT('Ctrl Pts',(7.67863699410016,-1.9032747864763,49.5651022844631));
#63428=CARTESIAN_POINT('Ctrl Pts',(7.65344952427684,-2.00489197751325,49.5608706291285));
#63429=CARTESIAN_POINT('Ctrl Pts',(7.62626326518703,-2.10593354250732,49.5566389737939));
#63430=CARTESIAN_POINT('Ctrl Pts',(7.59711072894231,-2.20631583690769,49.5524073184593));
#63431=CARTESIAN_POINT('Ctrl Pts',(7.54260941011058,-2.39398278246085,49.544496144123));
#63432=CARTESIAN_POINT('Ctrl Pts',(7.48107696304029,-2.57988131185113,49.5365849697867));
#63433=CARTESIAN_POINT('Ctrl Pts',(7.41264373094572,-2.76344602228288,49.5286737954504));
#63434=CARTESIAN_POINT('Ctrl Pts',(7.34428468935969,-2.94681172473563,49.5207711978543));
#63435=CARTESIAN_POINT('Ctrl Pts',(7.26903988384833,-3.12784832774792,49.5128686002581));
#63436=CARTESIAN_POINT('Ctrl Pts',(7.18709001154408,-3.30600335238234,49.5049660026619));
#63437=CARTESIAN_POINT('Ctrl Pts',(7.10521377135276,-3.48399830439527,49.4970705055644));
#63438=CARTESIAN_POINT('Ctrl Pts',(7.01664460893177,-3.65911652444873,49.4891750084669));
#63439=CARTESIAN_POINT('Ctrl Pts',(6.92161219521525,-3.83082309941969,49.4812795113694));
#63440=CARTESIAN_POINT('Ctrl Pts',(6.82664753310625,-4.0024072593533,49.473389643221));
#63441=CARTESIAN_POINT('Ctrl Pts',(6.72522896642979,-4.17058431964628,49.4654997750726));
#63442=CARTESIAN_POINT('Ctrl Pts',(6.617633325523,-4.33484142373483,49.4576099069242));
#63443=CARTESIAN_POINT('Ctrl Pts',(6.51009443085917,-4.49901189816572,49.4497241999144));
#63444=CARTESIAN_POINT('Ctrl Pts',(6.39638514208911,-4.65926624819583,49.4418384929046));
#63445=CARTESIAN_POINT('Ctrl Pts',(6.27682721679446,-4.81511797264701,49.4339527858948));
#63446=CARTESIAN_POINT('Ctrl Pts',(6.15731016886918,-4.97091641072265,49.4260697750422));
#63447=CARTESIAN_POINT('Ctrl Pts',(6.03194867947861,-5.12231495002544,49.4181867641895));
#63448=CARTESIAN_POINT('Ctrl Pts',(5.901106803828,-5.2688575127645,49.4103037533369));
#63449=CARTESIAN_POINT('Ctrl Pts',(5.77026297555807,-5.41540226243214,49.4024206248421));
#63450=CARTESIAN_POINT('Ctrl Pts',(5.63393882094205,-5.55709062790542,49.3945374963474));
#63451=CARTESIAN_POINT('Ctrl Pts',(5.49253790022358,-5.69350054137237,49.3866543678526));
#63452=CARTESIAN_POINT('Ctrl Pts',(5.35112823654482,-5.82991888920067,49.3787707519361));
#63453=CARTESIAN_POINT('Ctrl Pts',(5.20464142918148,-5.96105789470025,49.3708871360196));
#63454=CARTESIAN_POINT('Ctrl Pts',(5.05351705104708,-6.08653320164907,49.3630035201031));
#63455=CARTESIAN_POINT('Ctrl Pts',(4.90235792553739,-6.21203735859306,49.3551180915409));
#63456=CARTESIAN_POINT('Ctrl Pts',(4.74655936988931,-6.33187500173534,49.3472326629787));
#63457=CARTESIAN_POINT('Ctrl Pts',(4.58659328324015,-6.44570268117731,49.3393472344164));
#63458=CARTESIAN_POINT('Ctrl Pts',(4.42656352648673,-6.55957566659862,49.3314586672761));
#63459=CARTESIAN_POINT('Ctrl Pts',(4.26236321429242,-6.66743372201613,49.3235701001357));
#63460=CARTESIAN_POINT('Ctrl Pts',(4.09449259617966,-6.76897712951004,49.3156815329954));
#63461=CARTESIAN_POINT('Ctrl Pts',(3.92644332723753,-6.87062860126302,49.3077845707048));
#63462=CARTESIAN_POINT('Ctrl Pts',(3.75471624571798,-6.96595182364409,49.2998876084142));
#63463=CARTESIAN_POINT('Ctrl Pts',(3.57983651224036,-7.05469287394078,49.2919906461236));
#63464=CARTESIAN_POINT('Ctrl Pts',(3.40485012539054,-7.14348804447243,49.2840888677366));
#63465=CARTESIAN_POINT('Ctrl Pts',(3.22670756574118,-7.22569289582836,49.2761870893496));
#63466=CARTESIAN_POINT('Ctrl Pts',(3.04595350836448,-7.30110185005538,49.2682853109625));
#63467=CARTESIAN_POINT('Ctrl Pts',(2.86496567357744,-7.37660833409884,49.2603733128476));
#63468=CARTESIAN_POINT('Ctrl Pts',(2.68135991670849,-7.44530124449316,49.2524613147326));
#63469=CARTESIAN_POINT('Ctrl Pts',(2.49569666048523,-7.50702465553716,49.2445493166177));
#63470=CARTESIAN_POINT('Ctrl Pts',(2.41790566520306,-7.53288613009597,49.2412342707623));
#63471=CARTESIAN_POINT('Ctrl Pts',(2.3397536061309,-7.55752470766804,49.237919224907));
#63472=CARTESIAN_POINT('Ctrl Pts',(2.26128219665213,-7.58093159361724,49.2346041790516));
#63473=CARTESIAN_POINT('Ctrl Pts',(2.07401468960909,-7.63679078116675,49.2266930127149));
#63474=CARTESIAN_POINT('Ctrl Pts',(1.88442447998909,-7.68578197425321,49.2187818463782));
#63475=CARTESIAN_POINT('Ctrl Pts',(1.69305742689917,-7.72770842806725,49.2108706800415));
#63476=CARTESIAN_POINT('Ctrl Pts',(1.50189780963638,-7.76958943493268,49.2029680891586));
#63477=CARTESIAN_POINT('Ctrl Pts',(1.30896551909382,-7.80442088290069,49.1950654982757));
#63478=CARTESIAN_POINT('Ctrl Pts',(1.11482283013101,-7.83205535331682,49.1871629073929));
#63479=CARTESIAN_POINT('Ctrl Pts',(0.920854547395602,-7.85966499857082,
49.1792674157269));
#63480=CARTESIAN_POINT('Ctrl Pts',(0.725678371578291,-7.88009049750577,
49.171371924061));
#63481=CARTESIAN_POINT('Ctrl Pts',(0.529868343850086,-7.89323511230887,
49.163476432395));
#63482=CARTESIAN_POINT('Ctrl Pts',(0.334197883670724,-7.9063703580225,49.1555865684001));
#63483=CARTESIAN_POINT('Ctrl Pts',(0.137894814354981,-7.9122350360598,49.1476967044051));
#63484=CARTESIAN_POINT('Ctrl Pts',(-0.0584598142239484,-7.91078399718517,
49.1398068404102));
#63485=CARTESIAN_POINT('Ctrl Pts',(-0.254710916503281,-7.90933372335838,
49.1319211362786));
#63486=CARTESIAN_POINT('Ctrl Pts',(-0.451013179879313,-7.90057542106007,
49.1240354321471));
#63487=CARTESIAN_POINT('Ctrl Pts',(-0.646783368387427,-7.88451598225138,
49.1161497280155));
#63488=CARTESIAN_POINT('Ctrl Pts',(-0.842486653808792,-7.86846203164309,
49.1082667187679));
#63489=CARTESIAN_POINT('Ctrl Pts',(-1.03765788350082,-7.84511194553864,
49.1003837095203));
#63490=CARTESIAN_POINT('Ctrl Pts',(-1.23171647932104,-7.81452465058298,
49.0925007002727));
#63491=CARTESIAN_POINT('Ctrl Pts',(-1.42577801802487,-7.78393689177335,
49.0846175714799));
#63492=CARTESIAN_POINT('Ctrl Pts',(-1.61872654723241,-7.74611175014959,
49.0767344426871));
#63493=CARTESIAN_POINT('Ctrl Pts',(-1.80998867403695,-7.70115978277675,
49.0688513138943));
#63494=CARTESIAN_POINT('Ctrl Pts',(-2.00126265556515,-7.65620502921115,
49.0609676964929));
#63495=CARTESIAN_POINT('Ctrl Pts',(-2.19084969038866,-7.60412264805146,
49.0530840790915));
#63496=CARTESIAN_POINT('Ctrl Pts',(-2.37818857432778,-7.54507389658556,
49.0452004616902));
#63497=CARTESIAN_POINT('Ctrl Pts',(-2.56557056049255,-7.48601155940506,
49.0373150304558));
#63498=CARTESIAN_POINT('Ctrl Pts',(-2.7507030360838,-7.41997976179219,49.0294295992214));
#63499=CARTESIAN_POINT('Ctrl Pts',(-2.933041668067,-7.34718909334602,49.021544167987));
#63500=CARTESIAN_POINT('Ctrl Pts',(-3.11545290238636,-7.27436944161462,
49.013655596986));
#63501=CARTESIAN_POINT('Ctrl Pts',(-3.29506775638119,-7.19478568436457,
49.0057670259851));
#63502=CARTESIAN_POINT('Ctrl Pts',(-3.47136329712847,-7.10869593240204,
48.9978784549842));
#63503=CARTESIAN_POINT('Ctrl Pts',(-3.64784649422363,-7.02251454290646,
48.9899814870584));
#63504=CARTESIAN_POINT('Ctrl Pts',(-3.82100301078051,-6.92981347755794,
48.9820845191325));
#63505=CARTESIAN_POINT('Ctrl Pts',(-3.99033491131733,-6.83089659528836,
48.9741875512066));
#63506=CARTESIAN_POINT('Ctrl Pts',(-4.15977010364698,-6.73191937410994,
48.9662857661614));
#63507=CARTESIAN_POINT('Ctrl Pts',(-4.32537573844868,-6.62671896132088,
48.9583839811162));
#63508=CARTESIAN_POINT('Ctrl Pts',(-4.48668394442731,-6.51564180897156,
48.950482196071));
#63509=CARTESIAN_POINT('Ctrl Pts',(-4.64820080830229,-6.40442097437867,
48.942570189786));
#63510=CARTESIAN_POINT('Ctrl Pts',(-4.80540886433323,-6.28730842182488,
48.9346581835011));
#63511=CARTESIAN_POINT('Ctrl Pts',(-4.95787344496143,-6.16469073869455,
48.9267461772161));
#63512=CARTESIAN_POINT('Ctrl Pts',(-5.02175447060904,-6.11331524329342,
48.9234311313587));
#63513=CARTESIAN_POINT('Ctrl Pts',(-5.08480321349437,-6.06097375796805,
48.9201160855013));
#63514=CARTESIAN_POINT('Ctrl Pts',(-5.14698968350636,-6.00769658004456,
48.9168010396439));
#63515=CARTESIAN_POINT('Ctrl Pts',(-5.29194049870996,-5.8835124871017,48.9090739794108));
#63516=CARTESIAN_POINT('Ctrl Pts',(-5.43264100632112,-5.75386768989842,
48.9013469191777));
#63517=CARTESIAN_POINT('Ctrl Pts',(-5.56863976892367,-5.61908997293705,
48.8936198589445));
#63518=CARTESIAN_POINT('Ctrl Pts',(-5.70448562424255,-5.48446379040295,
48.8859014864654));
#63519=CARTESIAN_POINT('Ctrl Pts',(-5.83564000193244,-5.34471642644837,
48.8781831139862));
#63520=CARTESIAN_POINT('Ctrl Pts',(-5.96168298045172,-5.20021701860531,
48.8704647415071));
#63521=CARTESIAN_POINT('Ctrl Pts',(-6.08761020370407,-5.0558503160325,48.8627534574217));
#63522=CARTESIAN_POINT('Ctrl Pts',(-6.2084351360824,-4.90674052780092,48.8550421733363));
#63523=CARTESIAN_POINT('Ctrl Pts',(-6.32377328171775,-4.75329490789628,
48.847330889251));
#63524=CARTESIAN_POINT('Ctrl Pts',(-6.43902921392429,-4.59995866455981,
48.8396251017956));
#63525=CARTESIAN_POINT('Ctrl Pts',(-6.54880592956319,-4.4422930309143,48.8319193143402));
#63526=CARTESIAN_POINT('Ctrl Pts',(-6.65275792867704,-4.28073976579105,
48.8242135268847));
#63527=CARTESIAN_POINT('Ctrl Pts',(-6.75666117229831,-4.11926227226513,
48.8165113535923));
#63528=CARTESIAN_POINT('Ctrl Pts',(-6.85474494229913,-3.95390108078876,
48.8088091802998));
#63529=CARTESIAN_POINT('Ctrl Pts',(-6.94670589464532,-3.7851285596793,48.8011070070073));
#63530=CARTESIAN_POINT('Ctrl Pts',(-7.0386446643698,-3.61639674951179,48.7934066916164));
#63531=CARTESIAN_POINT('Ctrl Pts',(-7.12446338239918,-3.44425556495067,
48.7857063762255));
#63532=CARTESIAN_POINT('Ctrl Pts',(-7.20390364148951,-3.26920377525388,
48.7780060608346));
#63533=CARTESIAN_POINT('Ctrl Pts',(-7.28333949548774,-3.0941616924647,48.7703061724387));
#63534=CARTESIAN_POINT('Ctrl Pts',(-7.35639744499141,-2.91620965562223,
48.7626062840429));
#63535=CARTESIAN_POINT('Ctrl Pts',(-7.42286640105598,-2.73586830678567,
48.754906395647));
#63536=CARTESIAN_POINT('Ctrl Pts',(-7.489344020102,-2.55550345383751,48.7472055037152));
#63537=CARTESIAN_POINT('Ctrl Pts',(-7.54923081163289,-2.37274900903136,
48.7395046117833));
#63538=CARTESIAN_POINT('Ctrl Pts',(-7.602364917705,-2.18814274169858,48.7318037198515));
#63539=CARTESIAN_POINT('Ctrl Pts',(-7.65554123721299,-2.003389810285,48.7240967097945));
#63540=CARTESIAN_POINT('Ctrl Pts',(-7.70195405461654,-1.81678246596557,
48.7163896997376));
#63541=CARTESIAN_POINT('Ctrl Pts',(-7.74149201967497,-1.62887148336163,
48.7086826896806));
#63542=CARTESIAN_POINT('Ctrl Pts',(-7.78104603419266,-1.44088422294079,
48.7009725511535));
#63543=CARTESIAN_POINT('Ctrl Pts',(-7.81371957484111,-1.25159262641768,
48.6932624126264));
#63544=CARTESIAN_POINT('Ctrl Pts',(-7.83945298081485,-1.06155450241292,
48.6855522740993));
#63545=CARTESIAN_POINT('Ctrl Pts',(-7.86521824036993,-0.871281143521426,
48.6778325917316));
#63546=CARTESIAN_POINT('Ctrl Pts',(-7.88402616789796,-0.680259771110366,
48.6701129093639));
#63547=CARTESIAN_POINT('Ctrl Pts',(-7.89586916802662,-0.489051205301197,
48.6623932269962));
#63548=CARTESIAN_POINT('Ctrl Pts',(-7.90602630093594,-0.325061439598059,
48.6557724519413));
#63549=CARTESIAN_POINT('Ctrl Pts',(-7.91106117209866,-0.160934124743805,
48.6491516768865));
#63550=CARTESIAN_POINT('Ctrl Pts',(-7.91099943894101,0.00297944206225246,
48.6425309018316));
#63551=CARTESIAN_POINT('',(-7.89861493486562,-0.000610740782857052,44.6422669711751));
#63552=CARTESIAN_POINT('Ctrl Pts',(-7.91099937608635,0.00314190409447718,
48.6471968050444));
#63553=CARTESIAN_POINT('Ctrl Pts',(-7.91088721046558,0.285563686941826,
48.6372769727183));
#63554=CARTESIAN_POINT('Ctrl Pts',(-7.89565139589759,0.567761009271943,
48.6270474731004));
#63555=CARTESIAN_POINT('Ctrl Pts',(-7.85923996448297,0.905277399101737,
48.6138200189015));
#63556=CARTESIAN_POINT('Ctrl Pts',(-7.85250280932996,0.961966380417291,
48.6115642746992));
#63557=CARTESIAN_POINT('Ctrl Pts',(-7.84425755833575,1.02547194602397,48.6089941122671));
#63558=CARTESIAN_POINT('Ctrl Pts',(-7.84335315319302,1.03236653728107,48.608714506237));
#63559=CARTESIAN_POINT('Ctrl Pts',(-7.84186956477895,1.04356195870714,48.608259540743));
#63560=CARTESIAN_POINT('Ctrl Pts',(-7.84129592913883,1.04786353319166,48.6080845051546));
#63561=CARTESIAN_POINT('Ctrl Pts',(-7.84028428023256,1.05540232927292,48.6077773442198));
#63562=CARTESIAN_POINT('Ctrl Pts',(-7.83984780029141,1.058639759172,48.6076453091428));
#63563=CARTESIAN_POINT('Ctrl Pts',(-7.83896453275709,1.06516056742372,48.6073791032273));
#63564=CARTESIAN_POINT('Ctrl Pts',(-7.83851768725474,1.06844393710996,48.6072449289816));
#63565=CARTESIAN_POINT('Ctrl Pts',(-7.83765246954365,1.07477170136458,48.606986086716));
#63566=CARTESIAN_POINT('Ctrl Pts',(-7.83723438754337,1.07781612440499,48.6068614361949));
#63567=CARTESIAN_POINT('Ctrl Pts',(-7.8362366696263,1.08505011221129,48.6065649733085));
#63568=CARTESIAN_POINT('Ctrl Pts',(-7.8356554490285,1.08923944675882,48.6063930669918));
#63569=CARTESIAN_POINT('Ctrl Pts',(-7.83359068371568,1.10403473098796,48.6057851838064));
#63570=CARTESIAN_POINT('Ctrl Pts',(-7.83208896872543,1.11463808969363,48.6053481345194));
#63571=CARTESIAN_POINT('Ctrl Pts',(-7.8127078075982,1.24951214628098,48.5997714147074));
#63572=CARTESIAN_POINT('Ctrl Pts',(-7.79189486900127,1.37333720840431,48.594462778753));
#63573=CARTESIAN_POINT('Ctrl Pts',(-7.76496296691875,1.51312726990638,48.5882966040542));
#63574=CARTESIAN_POINT('Ctrl Pts',(-7.76172771917633,1.52963617241184,48.5875656365673));
#63575=CARTESIAN_POINT('Ctrl Pts',(-7.7543746149077,1.56653374870656,48.585925942423));
#63576=CARTESIAN_POINT('Ctrl Pts',(-7.75022896540084,1.58691670400343,48.5850160565843));
#63577=CARTESIAN_POINT('Ctrl Pts',(-7.71473713820974,1.75796300598614,48.5773476381108));
#63578=CARTESIAN_POINT('Ctrl Pts',(-7.67908238742702,1.90769311658165,48.5704201986618));
#63579=CARTESIAN_POINT('Ctrl Pts',(-7.63278398310707,2.07969165962441,48.5622841826174));
#63580=CARTESIAN_POINT('Ctrl Pts',(-7.62637497954438,2.1030723698496,48.5611743431005));
#63581=CARTESIAN_POINT('Ctrl Pts',(-7.42692231684401,2.81779422459459,48.5271362686909));
#63582=CARTESIAN_POINT('Ctrl Pts',(-7.14074121909561,3.47983008713342,48.4928118545262));
#63583=CARTESIAN_POINT('Ctrl Pts',(-6.63083032079658,4.32290000599168,48.4499025809316));
#63584=CARTESIAN_POINT('Ctrl Pts',(-6.48097897180199,4.54448080227559,48.4386618443156));
#63585=CARTESIAN_POINT('Ctrl Pts',(-6.30896901439826,4.77296330526061,48.4271035690781));
#63586=CARTESIAN_POINT('Ctrl Pts',(-6.29770065654915,4.787821548977,48.4263520433476));
#63587=CARTESIAN_POINT('Ctrl Pts',(-6.28140751667153,4.80914833346166,48.4252734678862));
#63588=CARTESIAN_POINT('Ctrl Pts',(-6.2764251030701,4.81564907461297,48.4249447180951));
#63589=CARTESIAN_POINT('Ctrl Pts',(-6.26775467847249,4.82692538761249,48.424374488408));
#63590=CARTESIAN_POINT('Ctrl Pts',(-6.26407128762613,4.83170449332727,48.4241328229148));
#63591=CARTESIAN_POINT('Ctrl Pts',(-6.25697464745524,4.84089044820499,48.4236683299806));
#63592=CARTESIAN_POINT('Ctrl Pts',(-6.25356220216553,4.84529791181364,48.423445470393));
#63593=CARTESIAN_POINT('Ctrl Pts',(-6.24550736329436,4.85567873811038,48.4229205860536));
#63594=CARTESIAN_POINT('Ctrl Pts',(-6.24086104988281,4.86164906067754,48.4226187197296));
#63595=CARTESIAN_POINT('Ctrl Pts',(-6.22474727712517,4.88229343295764,48.421574946252));
#63596=CARTESIAN_POINT('Ctrl Pts',(-6.21323652875118,4.89693370115999,48.4208347904964));
#63597=CARTESIAN_POINT('Ctrl Pts',(-6.08305399232213,5.06131203842615,48.4125247209952));
#63598=CARTESIAN_POINT('Ctrl Pts',(-5.95904278837199,5.20674951721812,48.4051769750983));
#63599=CARTESIAN_POINT('Ctrl Pts',(-5.58633867340523,5.61306949347952,48.3845315118996));
#63600=CARTESIAN_POINT('Ctrl Pts',(-5.3249341083309,5.86164033785009,48.3717704744258));
#63601=CARTESIAN_POINT('Ctrl Pts',(-4.72289078532052,6.36049727373689,48.3446445744573));
#63602=CARTESIAN_POINT('Ctrl Pts',(-4.37732995373802,6.60307375551591,48.330421893523));
#63603=CARTESIAN_POINT('Ctrl Pts',(-3.89722039962396,6.88578192154127,48.3105195163111));
#63604=CARTESIAN_POINT('Ctrl Pts',(-3.77859021653241,6.95158782467247,48.3055879704141));
#63605=CARTESIAN_POINT('Ctrl Pts',(-3.58982729169156,7.05003760696387,48.2976356971118));
#63606=CARTESIAN_POINT('Ctrl Pts',(-3.52080559709052,7.08475953216976,48.2947064126986));
#63607=CARTESIAN_POINT('Ctrl Pts',(-3.40243411480107,7.14215029536211,48.2896291077993));
#63608=CARTESIAN_POINT('Ctrl Pts',(-3.3533385107872,7.16533248214319,48.2875075028415));
#63609=CARTESIAN_POINT('Ctrl Pts',(-3.27449862031682,7.20157167018213,48.2840714610069));
#63610=CARTESIAN_POINT('Ctrl Pts',(-3.24490709516551,7.21495347386696,48.2827756273708));
#63611=CARTESIAN_POINT('Ctrl Pts',(-3.20761990210326,7.23153960203846,48.2811358016783));
#63612=CARTESIAN_POINT('Ctrl Pts',(-3.20000011862806,7.23491462922697,48.2808003313775));
#63613=CARTESIAN_POINT('Ctrl Pts',(-3.18860146669585,7.23994189868385,48.2802979601863));
#63614=CARTESIAN_POINT('Ctrl Pts',(-3.18482659944905,7.24160324383208,48.2801315039591));
#63615=CARTESIAN_POINT('Ctrl Pts',(-3.17712425666305,7.24498591066743,48.2797916870253));
#63616=CARTESIAN_POINT('Ctrl Pts',(-3.17319667763026,7.24670699235288,48.2796183147993));
#63617=CARTESIAN_POINT('Ctrl Pts',(-3.16472024820349,7.25041318707886,48.2792439488039));
#63618=CARTESIAN_POINT('Ctrl Pts',(-3.16017092694726,7.25239721368527,48.2790429032041));
#63619=CARTESIAN_POINT('Ctrl Pts',(-3.14793694902274,7.25771893636277,48.2785019303997));
#63620=CARTESIAN_POINT('Ctrl Pts',(-3.14024886584955,7.26104870208256,48.2781616291837));
#63621=CARTESIAN_POINT('Ctrl Pts',(-3.10509030739884,7.27620985076921,48.276603868408));
#63622=CARTESIAN_POINT('Ctrl Pts',(-3.07755839665891,7.28789749452489,48.275379780911));
#63623=CARTESIAN_POINT('Ctrl Pts',(-2.99276416413623,7.32332754355644,48.2715981228162));
#63624=CARTESIAN_POINT('Ctrl Pts',(-2.93528925475976,7.34655295842242,48.2690186171086));
#63625=CARTESIAN_POINT('Ctrl Pts',(-2.79197971761151,7.40251367595795,48.262556081804));
#63626=CARTESIAN_POINT('Ctrl Pts',(-2.70583728182034,7.43443362697497,48.2586444768703));
#63627=CARTESIAN_POINT('Ctrl Pts',(-2.25282967941924,7.59337859246078,48.2379943958161));
#63628=CARTESIAN_POINT('Ctrl Pts',(-1.87754123797349,7.69476896676719,48.2206460470832));
#63629=CARTESIAN_POINT('Ctrl Pts',(-1.4500534414654,7.77711305912955,48.2013623308277));
#63630=CARTESIAN_POINT('Ctrl Pts',(-1.40369240250953,7.78561430968249,48.1992767220109));
#63631=CARTESIAN_POINT('Ctrl Pts',(-1.30264374679526,7.80321173937491,48.194745025025));
#63632=CARTESIAN_POINT('Ctrl Pts',(-1.24793075909471,7.81214842748517,48.1923002837688));
#63633=CARTESIAN_POINT('Ctrl Pts',(-1.12686412053039,7.83061883731462,48.1869128409071));
#63634=CARTESIAN_POINT('Ctrl Pts',(-1.06047387089712,7.83988580345395,48.1839731525093));
#63635=CARTESIAN_POINT('Ctrl Pts',(-0.909683116964655,7.85898316850082,
48.1773330869217));
#63636=CARTESIAN_POINT('Ctrl Pts',(-0.825225463909605,7.86829988341015,
48.1736400511637));
#63637=CARTESIAN_POINT('Ctrl Pts',(-0.621717635841421,7.88743647435205,
48.1648094599451));
#63638=CARTESIAN_POINT('Ctrl Pts',(-0.502562140077705,7.89592421825133,
48.1596950893038));
#63639=CARTESIAN_POINT('Ctrl Pts',(-0.17637824849564,7.91174516962143,48.1458553765805));
#63640=CARTESIAN_POINT('Ctrl Pts',(0.030821625607908,7.91365129023093,48.1372426468061));
#63641=CARTESIAN_POINT('Ctrl Pts',(0.294789407222997,7.90571081779369,48.1264791180981));
#63642=CARTESIAN_POINT('Ctrl Pts',(0.351694234569414,7.90338380774433,48.1241709485929));
#63643=CARTESIAN_POINT('Ctrl Pts',(0.42529106922276,7.89957776498674,48.1212004553319));
#63644=CARTESIAN_POINT('Ctrl Pts',(0.442009892778786,7.89865992534494,48.1205266387112));
#63645=CARTESIAN_POINT('Ctrl Pts',(0.469050676289211,7.89708930096658,48.1194383704988));
#63646=CARTESIAN_POINT('Ctrl Pts',(0.479374462665852,7.89646934329486,48.1190232514962));
#63647=CARTESIAN_POINT('Ctrl Pts',(0.499081288172488,7.89524713172535,48.1182315291213));
#63648=CARTESIAN_POINT('Ctrl Pts',(0.508464530459459,7.89464839147685,48.1178548544885));
#63649=CARTESIAN_POINT('Ctrl Pts',(0.529815503356921,7.89324777270262,48.1169984284899));
#63650=CARTESIAN_POINT('Ctrl Pts',(0.541782533979159,7.89243540080057,48.1165188911918));
#63651=CARTESIAN_POINT('Ctrl Pts',(0.577321298024332,7.88994167088033,48.1150962230125));
#63652=CARTESIAN_POINT('Ctrl Pts',(0.600887457167115,7.88818190225193,48.1141546980934));
#63653=CARTESIAN_POINT('Ctrl Pts',(0.764257205336719,7.8752461422618,48.1076404492136));
#63654=CARTESIAN_POINT('Ctrl Pts',(0.903752443465567,7.86045953334619,48.1021436763652));
#63655=CARTESIAN_POINT('Ctrl Pts',(1.6469122255149,7.76163807512629,48.0731613590942));
#63656=CARTESIAN_POINT('Ctrl Pts',(2.23972135571986,7.61176833761153,48.0513151149297));
#63657=CARTESIAN_POINT('Ctrl Pts',(3.07314921220822,7.29515198038458,48.0190101585542));
#63658=CARTESIAN_POINT('Ctrl Pts',(3.33128403201259,7.1809486785566,48.0087243526581));
#63659=CARTESIAN_POINT('Ctrl Pts',(3.68152602898821,7.00303929452204,47.9938125844243));
#63660=CARTESIAN_POINT('Ctrl Pts',(3.77922709314576,6.95080099906397,47.9895433387148));
#63661=CARTESIAN_POINT('Ctrl Pts',(3.90639103690575,6.87933585053109,47.9838050285108));
#63662=CARTESIAN_POINT('Ctrl Pts',(3.93687077707966,6.86193858256721,47.9824156055327));
#63663=CARTESIAN_POINT('Ctrl Pts',(3.98027494489441,6.83677991367922,47.9804156408983));
#63664=CARTESIAN_POINT('Ctrl Pts',(3.99329477109151,6.8291833400393,47.9798129471165));
#63665=CARTESIAN_POINT('Ctrl Pts',(4.01329072887739,6.81743972387717,47.9788829475732));
#63666=CARTESIAN_POINT('Ctrl Pts',(4.0202823674889,6.81331905521461,47.9785569446317));
#63667=CARTESIAN_POINT('Ctrl Pts',(4.03326832778059,6.80563855934635,47.9779498832717));
#63668=CARTESIAN_POINT('Ctrl Pts',(4.03926431318597,6.80208154994561,47.9776689668664));
#63669=CARTESIAN_POINT('Ctrl Pts',(4.04917210228179,6.79618621405542,47.9772037434508));
#63670=CARTESIAN_POINT('Ctrl Pts',(4.05308660919297,6.79385242025956,47.9770196685798));
#63671=CARTESIAN_POINT('Ctrl Pts',(4.06076152322341,6.78926771153022,47.9766582354467));
#63672=CARTESIAN_POINT('Ctrl Pts',(4.06452208130228,6.78701705153371,47.9764808904026));
#63673=CARTESIAN_POINT('Ctrl Pts',(4.07322480718344,6.78179872174675,47.9760698936315));
#63674=CARTESIAN_POINT('Ctrl Pts',(4.07816560109326,6.77882877508604,47.9758361228778));
#63675=CARTESIAN_POINT('Ctrl Pts',(4.09407120719461,6.76924411822539,47.9750821409098));
#63676=CARTESIAN_POINT('Ctrl Pts',(4.10502316462872,6.76260820959545,47.9745608065324));
#63677=CARTESIAN_POINT('Ctrl Pts',(4.22080459428456,6.69207010530995,47.9690258830486));
#63678=CARTESIAN_POINT('Ctrl Pts',(4.32413488139296,6.62577136506182,47.9638711596446));
#63679=CARTESIAN_POINT('Ctrl Pts',(4.85884722843049,6.26485385073044,47.9361350953094));
#63680=CARTESIAN_POINT('Ctrl Pts',(5.26178922828531,5.93045751736016,47.9116917965391));
#63681=CARTESIAN_POINT('Ctrl Pts',(5.64834048177626,5.53903808415139,47.8864166317572));
#63682=CARTESIAN_POINT('Ctrl Pts',(5.6677609939118,5.51916464859386,47.88514114323));
#63683=CARTESIAN_POINT('Ctrl Pts',(5.70801223592311,5.47753816892919,47.8824861568855));
#63684=CARTESIAN_POINT('Ctrl Pts',(5.72882427929581,5.45576763295687,47.881106931163));
#63685=CARTESIAN_POINT('Ctrl Pts',(5.79928634076314,5.38121270498719,47.8764161431193));
#63686=CARTESIAN_POINT('Ctrl Pts',(5.84833556943622,5.32786481566565,47.8731145856143));
#63687=CARTESIAN_POINT('Ctrl Pts',(5.96593172055449,5.19638159423117,47.8651174537263));
#63688=CARTESIAN_POINT('Ctrl Pts',(6.0336858454794,5.11755398914653,47.8604399195119));
#63689=CARTESIAN_POINT('Ctrl Pts',(6.22219747362919,4.8892828247905,47.8472439583703));
#63690=CARTESIAN_POINT('Ctrl Pts',(6.33909478434824,4.73674059261592,47.8388396148963));
#63691=CARTESIAN_POINT('Ctrl Pts',(6.55282235508251,4.43573912994225,47.8230806209574));
#63692=CARTESIAN_POINT('Ctrl Pts',(6.65044670928969,4.2879862905131,47.8156995897879));
#63693=CARTESIAN_POINT('Ctrl Pts',(6.75959729366131,4.11008131149444,47.8072206700339));
#63694=CARTESIAN_POINT('Ctrl Pts',(6.77599683018701,4.08298799262269,47.8059402054002));
#63695=CARTESIAN_POINT('Ctrl Pts',(6.79741421437031,4.04712034894147,47.8042591540958));
#63696=CARTESIAN_POINT('Ctrl Pts',(6.80257845141105,4.03843404476803,47.8038531269772));
#63697=CARTESIAN_POINT('Ctrl Pts',(6.81100107311602,4.0242051040034,47.803189785819));
#63698=CARTESIAN_POINT('Ctrl Pts',(6.81426936213079,4.01866836124332,47.802932104313));
#63699=CARTESIAN_POINT('Ctrl Pts',(6.82056844848896,4.00796742674824,47.8024349213729));
#63700=CARTESIAN_POINT('Ctrl Pts',(6.82360013882355,4.00280376736772,47.8021953869255));
#63701=CARTESIAN_POINT('Ctrl Pts',(6.8305557051682,3.99092598711178,47.801645260455));
#63702=CARTESIAN_POINT('Ctrl Pts',(6.83447555244873,3.98420950747386,47.8013348177207));
#63703=CARTESIAN_POINT('Ctrl Pts',(6.84489011194071,3.96630403897546,47.8005088942975));
#63704=CARTESIAN_POINT('Ctrl Pts',(6.85136730420453,3.95510485816732,47.7999940614729));
#63705=CARTESIAN_POINT('Ctrl Pts',(6.87215546145045,3.91895745406219,47.7983379551569));
#63706=CARTESIAN_POINT('Ctrl Pts',(6.88635793025572,3.89394692981299,47.7972006811843));
#63707=CARTESIAN_POINT('Ctrl Pts',(7.15142878931303,3.42117159650883,47.7758624602311));
#63708=CARTESIAN_POINT('Ctrl Pts',(7.35827922229107,2.95011072057071,47.7574079628831));
#63709=CARTESIAN_POINT('Ctrl Pts',(7.60649418201631,2.19223900328639,47.7299201064291));
#63710=CARTESIAN_POINT('Ctrl Pts',(7.68032382267733,1.91762675162704,47.7203536042651));
#63711=CARTESIAN_POINT('Ctrl Pts',(7.79577654976965,1.37268149497652,47.7013822521474));
#63712=CARTESIAN_POINT('Ctrl Pts',(7.83848185921121,1.10298549138838,47.691996410984));
#63713=CARTESIAN_POINT('Ctrl Pts',(7.88968194476937,0.618638925296452,47.6744061477431));
#63714=CARTESIAN_POINT('Ctrl Pts',(7.90353688832454,0.40483022463031,47.6663870864262));
#63715=CARTESIAN_POINT('Ctrl Pts',(7.90933487662088,0.164425106429818,47.6568407385094));
#63716=CARTESIAN_POINT('Ctrl Pts',(7.90983816036681,0.138108840181999,47.6557886089252));
#63717=CARTESIAN_POINT('Ctrl Pts',(7.91030052551998,0.105392338829513,47.6544712285875));
#63718=CARTESIAN_POINT('Ctrl Pts',(7.91038318847114,0.0989937382490356,
47.654213133667));
#63719=CARTESIAN_POINT('Ctrl Pts',(7.91049451209835,0.0894832863733912,
47.6538288478653));
#63720=CARTESIAN_POINT('Ctrl Pts',(7.91052910048243,0.0863714932411258,
47.6537030038978));
#63721=CARTESIAN_POINT('Ctrl Pts',(7.9105927543886,0.0803236903608817,47.6534582160627));
#63722=CARTESIAN_POINT('Ctrl Pts',(7.91062202150291,0.0773876854483604,
47.6533392841217));
#63723=CARTESIAN_POINT('Ctrl Pts',(7.91067963600495,0.0712660210728465,
47.6530911087428));
#63724=CARTESIAN_POINT('Ctrl Pts',(7.91070769362919,0.068080358112815,47.6529618482937));
#63725=CARTESIAN_POINT('Ctrl Pts',(7.91077959104164,0.0593159838862543,
47.6526059213124));
#63726=CARTESIAN_POINT('Ctrl Pts',(7.9108194538566,0.0537372511366036,47.6523790236603));
#63727=CARTESIAN_POINT('Ctrl Pts',(7.91095083274186,0.0321560304680096,
47.6514999661282));
#63728=CARTESIAN_POINT('Ctrl Pts',(7.91099969336156,0.0161534191598449,
47.6508453567158));
#63729=CARTESIAN_POINT('Ctrl Pts',(7.91100477424842,-0.250248746012721,
47.6399028293494));
#63730=CARTESIAN_POINT('Ctrl Pts',(7.8991209536246,-0.500488600898607,47.6289658715112));
#63731=CARTESIAN_POINT('Ctrl Pts',(7.81910148450312,-1.34104792581877,47.5909963376035));
#63732=CARTESIAN_POINT('Ctrl Pts',(7.69639076454295,-1.9241624603802,47.5627575848675));
#63733=CARTESIAN_POINT('Ctrl Pts',(7.40981353914708,-2.78911340422794,47.5218229379346));
#63734=CARTESIAN_POINT('Ctrl Pts',(7.29205781415525,-3.08389578830358,47.5080168173924));
#63735=CARTESIAN_POINT('Ctrl Pts',(7.11104079998649,-3.46822852514133,47.4903388075217));
#63736=CARTESIAN_POINT('Ctrl Pts',(7.06318571930844,-3.56467657678949,47.4859291204014));
#63737=CARTESIAN_POINT('Ctrl Pts',(7.00660087830228,-3.6731021699837,47.4809998663061));
#63738=CARTESIAN_POINT('Ctrl Pts',(6.99979003808101,-3.68606495396276,47.4804110082937));
#63739=CARTESIAN_POINT('Ctrl Pts',(6.9894912852694,-3.70553465451106,47.4795272360412));
#63740=CARTESIAN_POINT('Ctrl Pts',(6.98603020962882,-3.71205568562662,47.4792313462821));
#63741=CARTESIAN_POINT('Ctrl Pts',(6.98005691548964,-3.723272057439,47.4787226011407));
#63742=CARTESIAN_POINT('Ctrl Pts',(6.97754907830417,-3.72796971784579,47.4785095863675));
#63743=CARTESIAN_POINT('Ctrl Pts',(6.97237019710205,-3.73764722355843,47.4780708812793));
#63744=CARTESIAN_POINT('Ctrl Pts',(6.96969855624922,-3.74262674713997,47.4778452129005));
#63745=CARTESIAN_POINT('Ctrl Pts',(6.96248399017405,-3.7560390621629,47.4772375518502));
#63746=CARTESIAN_POINT('Ctrl Pts',(6.95793107428815,-3.76446648493944,47.4768559243261));
#63747=CARTESIAN_POINT('Ctrl Pts',(6.94114731557598,-3.79539866141476,47.4754558668672));
#63748=CARTESIAN_POINT('Ctrl Pts',(6.92882244076337,-3.81785236174675,47.4744408805198));
#63749=CARTESIAN_POINT('Ctrl Pts',(6.73308272085197,-4.17038498500779,47.4585248608936));
#63750=CARTESIAN_POINT('Ctrl Pts',(6.52636836969631,-4.48698880418757,47.4445391321518));
#63751=CARTESIAN_POINT('Ctrl Pts',(6.16255302411474,-4.96556252384246,47.4231909295439));
#63752=CARTESIAN_POINT('Ctrl Pts',(6.01981544687402,-5.13767424317418,47.4154568440733));
#63753=CARTESIAN_POINT('Ctrl Pts',(5.65474529316149,-5.5417373434592,47.3967652757463));
#63754=CARTESIAN_POINT('Ctrl Pts',(5.42521398064285,-5.76663174778966,47.3858976714903));
#63755=CARTESIAN_POINT('Ctrl Pts',(4.93373373572088,-6.19279789274453,47.3630361657022));
#63756=CARTESIAN_POINT('Ctrl Pts',(4.67158810927335,-6.39286311395369,47.3510373574941));
#63757=CARTESIAN_POINT('Ctrl Pts',(4.3889127272084,-6.58190545892171,47.3374574438699));
#63758=CARTESIAN_POINT('Ctrl Pts',(4.38004904190869,-6.58780728206612,47.3370309989742));
#63759=CARTESIAN_POINT('Ctrl Pts',(4.36439557378502,-6.59818447800528,47.3362767326171));
#63760=CARTESIAN_POINT('Ctrl Pts',(4.35761072934331,-6.60266732929056,47.3359494216729));
#63761=CARTESIAN_POINT('Ctrl Pts',(4.34731421420031,-6.60944761178649,47.3354521059797));
#63762=CARTESIAN_POINT('Ctrl Pts',(4.34380760277923,-6.61175272676108,47.3352826342853));
#63763=CARTESIAN_POINT('Ctrl Pts',(4.33774287577367,-6.61573254389019,47.3349893529826));
#63764=CARTESIAN_POINT('Ctrl Pts',(4.33518561665835,-6.61740855756204,47.3348656330602));
#63765=CARTESIAN_POINT('Ctrl Pts',(4.32994350924534,-6.6208398633572,47.334611909692));
#63766=CARTESIAN_POINT('Ctrl Pts',(4.32725856496361,-6.62259500508461,47.3344818961613));
#63767=CARTESIAN_POINT('Ctrl Pts',(4.32083508546776,-6.62678844434955,47.3341707101968));
#63768=CARTESIAN_POINT('Ctrl Pts',(4.31709555650466,-6.62922520947093,47.3339894345693));
#63769=CARTESIAN_POINT('Ctrl Pts',(4.30574988725227,-6.63660464333036,47.3334391073623));
#63770=CARTESIAN_POINT('Ctrl Pts',(4.29813733114477,-6.64153737960748,47.3330693938454));
#63771=CARTESIAN_POINT('Ctrl Pts',(4.2197393895256,-6.69214594442403,47.3292572874959));
#63772=CARTESIAN_POINT('Ctrl Pts',(4.14823946307442,-6.73669995384896,47.3257420135045));
#63773=CARTESIAN_POINT('Ctrl Pts',(3.97009734239516,-6.84379497042627,47.3169169727176));
#63774=CARTESIAN_POINT('Ctrl Pts',(3.86267611333562,-6.90499336531258,47.3115378381864));
#63775=CARTESIAN_POINT('Ctrl Pts',(3.11232979114476,-7.30948000298624,47.2738045112072));
#63776=CARTESIAN_POINT('Ctrl Pts',(2.42606091939876,-7.56501890904921,47.238893713967));
#63777=CARTESIAN_POINT('Ctrl Pts',(1.41079622591448,-7.79039905737326,47.1929630832285));
#63778=CARTESIAN_POINT('Ctrl Pts',(1.10342509319658,-7.8398434252781,47.1796982723357));
#63779=CARTESIAN_POINT('Ctrl Pts',(0.74925910478261,-7.87556640918489,47.1651751942411));
#63780=CARTESIAN_POINT('Ctrl Pts',(0.704564844888434,-7.87969059906658,
47.163355856108));
#63781=CARTESIAN_POINT('Ctrl Pts',(0.648182891380866,-7.88440972545541,
47.1610773389292));
#63782=CARTESIAN_POINT('Ctrl Pts',(0.63652618443597,-7.88535935754181,47.1606071581899));
#63783=CARTESIAN_POINT('Ctrl Pts',(0.617971488106171,-7.88682953358245,
47.1598601536594));
#63784=CARTESIAN_POINT('Ctrl Pts',(0.611074869267015,-7.88736688359064,
47.1595828087022));
#63785=CARTESIAN_POINT('Ctrl Pts',(0.598084553654909,-7.88836188375041,
47.1590609898046));
#63786=CARTESIAN_POINT('Ctrl Pts',(0.591991016696638,-7.88882152027104,
47.1588164544426));
#63787=CARTESIAN_POINT('Ctrl Pts',(0.578294728702754,-7.8898386751054,47.1582673583399));
#63788=CARTESIAN_POINT('Ctrl Pts',(0.570691687346488,-7.89039226596766,
47.157962919541));
#63789=CARTESIAN_POINT('Ctrl Pts',(0.551362985804402,-7.89177153940778,
47.1571899108786));
#63790=CARTESIAN_POINT('Ctrl Pts',(0.539636245587326,-7.89258208042732,
47.1567218102988));
#63791=CARTESIAN_POINT('Ctrl Pts',(0.474917751151294,-7.89691044808477,
47.1541432621886));
#63792=CARTESIAN_POINT('Ctrl Pts',(0.421892837630961,-7.899920763264,47.152048544574));
#63793=CARTESIAN_POINT('Ctrl Pts',(-0.472329576491392,-7.94165820869696,
47.1170129571966));
#63794=CARTESIAN_POINT('Ctrl Pts',(-1.31426262356121,-7.84637854832496,
47.0891281908939));
#63795=CARTESIAN_POINT('Ctrl Pts',(-2.39647098960759,-7.54453962645387,
47.0495012253935));
#63796=CARTESIAN_POINT('Ctrl Pts',(-2.6633563306627,-7.4545063047418,47.0393229717895));
#63797=CARTESIAN_POINT('Ctrl Pts',(-3.00094434289365,-7.32017485820054,
47.0252963779983));
#63798=CARTESIAN_POINT('Ctrl Pts',(-3.07655450506013,-7.2887199470262,47.0220774014341));
#63799=CARTESIAN_POINT('Ctrl Pts',(-3.15998510632024,-7.25248216148423,
47.0184251693154));
#63800=CARTESIAN_POINT('Ctrl Pts',(-3.16830355362299,-7.24885204468059,
47.0180599065823));
#63801=CARTESIAN_POINT('Ctrl Pts',(-3.18066630040037,-7.24343167613642,
47.0175153710854));
#63802=CARTESIAN_POINT('Ctrl Pts',(-3.18471539910629,-7.24165232442901,
47.0173367528613));
#63803=CARTESIAN_POINT('Ctrl Pts',(-3.1916294392087,-7.23860707133666,47.0170312890721));
#63804=CARTESIAN_POINT('Ctrl Pts',(-3.19449512913079,-7.23734286049725,
47.0169045458854));
#63805=CARTESIAN_POINT('Ctrl Pts',(-3.20037665482123,-7.23474402751933,
47.0166441377637));
#63806=CARTESIAN_POINT('Ctrl Pts',(-3.20339240057618,-7.23340922417114,
47.0165104621253));
#63807=CARTESIAN_POINT('Ctrl Pts',(-3.21063986389414,-7.23019599321715,
47.0161888487613));
#63808=CARTESIAN_POINT('Ctrl Pts',(-3.21487076458554,-7.22831573762523,
47.0160008006189));
#63809=CARTESIAN_POINT('Ctrl Pts',(-3.2302523669204,-7.22146381987513,47.0153160679354));
#63810=CARTESIAN_POINT('Ctrl Pts',(-3.24139315815675,-7.21647008217896,
47.0148180618169));
#63811=CARTESIAN_POINT('Ctrl Pts',(-3.41380489813097,-7.13870860837326,
47.0070796647416));
#63812=CARTESIAN_POINT('Ctrl Pts',(-3.57259250770177,-7.06058068783148,
46.9995273596727));
#63813=CARTESIAN_POINT('Ctrl Pts',(-4.39908478511926,-6.61890309859251,
46.9584633062142));
#63814=CARTESIAN_POINT('Ctrl Pts',(-5.01443691017841,-6.16583135000306,
46.9221278095568));
#63815=CARTESIAN_POINT('Ctrl Pts',(-5.71043494809567,-5.47924058558368,
46.8793431069405));
#63816=CARTESIAN_POINT('Ctrl Pts',(-5.85879097719294,-5.32031224824233,
46.870063123635));
#63817=CARTESIAN_POINT('Ctrl Pts',(-6.06284906827188,-5.08281009042416,
46.8570838693297));
#63818=CARTESIAN_POINT('Ctrl Pts',(-6.12395204180475,-5.00902280567634,
46.8531663871853));
#63819=CARTESIAN_POINT('Ctrl Pts',(-6.19285003734239,-4.92267656618556,
46.8487110122654));
#63820=CARTESIAN_POINT('Ctrl Pts',(-6.20196690305786,-4.91118546754688,
46.848120662449));
#63821=CARTESIAN_POINT('Ctrl Pts',(-6.21573598630445,-4.89373112758165,
46.847227840397));
#63822=CARTESIAN_POINT('Ctrl Pts',(-6.22041167539806,-4.88778649180598,
46.846924441389));
#63823=CARTESIAN_POINT('Ctrl Pts',(-6.22881219868047,-4.8770745529271,46.8463789520101));
#63824=CARTESIAN_POINT('Ctrl Pts',(-6.23254009964859,-4.87230966870131,
46.8461367408754));
#63825=CARTESIAN_POINT('Ctrl Pts',(-6.24053214640193,-4.86207030824909,
46.8456171764835));
#63826=CARTESIAN_POINT('Ctrl Pts',(-6.24479456414573,-4.85659448632093,
46.8453398912662));
#63827=CARTESIAN_POINT('Ctrl Pts',(-6.25628100697458,-4.84179801544654,
46.8445921555585));
#63828=CARTESIAN_POINT('Ctrl Pts',(-6.26349141812948,-4.8324667942123,46.8441222394033));
#63829=CARTESIAN_POINT('Ctrl Pts',(-6.28976975759651,-4.79830154404987,
46.8424076360185));
#63830=CARTESIAN_POINT('Ctrl Pts',(-6.30871118790363,-4.77337034884639,
46.8411678937925));
#63831=CARTESIAN_POINT('Ctrl Pts',(-6.61209269558256,-4.36909159813067,
46.8212464697403));
#63832=CARTESIAN_POINT('Ctrl Pts',(-6.86202066896686,-3.9650303849528,46.8039940377157));
#63833=CARTESIAN_POINT('Ctrl Pts',(-7.30284478223114,-3.08433829828622,
46.7695523461206));
#63834=CARTESIAN_POINT('Ctrl Pts',(-7.4866504296468,-2.6066659584237,46.752543446868));
#63835=CARTESIAN_POINT('Ctrl Pts',(-7.66522043561788,-1.96293201441549,
46.7286005782283));
#63836=CARTESIAN_POINT('Ctrl Pts',(-7.70276356087339,-1.81000997970422,
46.7228336843915));
#63837=CARTESIAN_POINT('Ctrl Pts',(-7.75817318410624,-1.55118540512928,
46.7127978269462));
#63838=CARTESIAN_POINT('Ctrl Pts',(-7.77849185530214,-1.44585269489026,
46.7086379478401));
#63839=CARTESIAN_POINT('Ctrl Pts',(-7.79978152516121,-1.32199406141429,
46.7036256519453));
#63840=CARTESIAN_POINT('Ctrl Pts',(-7.80283778688522,-1.30383380835545,
46.7028877164963));
#63841=CARTESIAN_POINT('Ctrl Pts',(-7.80677141519388,-1.27995100885669,
46.7019130834933));
#63842=CARTESIAN_POINT('Ctrl Pts',(-7.80770596995518,-1.27423781161715,
46.701679620768));
#63843=CARTESIAN_POINT('Ctrl Pts',(-7.80922124737563,-1.26491023813689,
46.7012979432075));
#63844=CARTESIAN_POINT('Ctrl Pts',(-7.80980573529075,-1.26129646710877,
46.7011499434841));
#63845=CARTESIAN_POINT('Ctrl Pts',(-7.81092719964687,-1.25433201237616,
46.7008644721098));
#63846=CARTESIAN_POINT('Ctrl Pts',(-7.81146452904037,-1.25098138552524,
46.7007270207855));
#63847=CARTESIAN_POINT('Ctrl Pts',(-7.81269113813946,-1.24330101017495,
46.7004116981351));
#63848=CARTESIAN_POINT('Ctrl Pts',(-7.81337897442365,-1.23897103427697,
46.7002337433392));
#63849=CARTESIAN_POINT('Ctrl Pts',(-7.81556134363772,-1.22515877795945,
46.6996654868646));
#63850=CARTESIAN_POINT('Ctrl Pts',(-7.81704221201616,-1.2156743813109,46.6992743898585));
#63851=CARTESIAN_POINT('Ctrl Pts',(-7.8300968239229,-1.13105439358331,46.6957771884164));
#63852=CARTESIAN_POINT('Ctrl Pts',(-7.84060388370665,-1.05576054745434,
46.6926104264097));
#63853=CARTESIAN_POINT('Ctrl Pts',(-7.890692489434,-0.65467418587675,46.675494812044));
#63854=CARTESIAN_POINT('Ctrl Pts',(-7.91105429201082,-0.326825594517507,
46.6606534484356));
#63855=CARTESIAN_POINT('Ctrl Pts',(-7.91086344611451,0.824330149796626,
46.6077205462351));
#63856=CARTESIAN_POINT('Ctrl Pts',(-7.78228473438266,1.64252519945692,46.5693162931647));
#63857=CARTESIAN_POINT('Ctrl Pts',(-7.51327293775616,2.47740673728522,46.5334218007386));
#63858=CARTESIAN_POINT('Ctrl Pts',(-7.49625419425399,2.52843579870849,46.5312382504718));
#63859=CARTESIAN_POINT('Ctrl Pts',(-7.4749613761652,2.59017490666403,46.5286086037491));
#63860=CARTESIAN_POINT('Ctrl Pts',(-7.47118288529898,2.60105361693812,46.5281457092195));
#63861=CARTESIAN_POINT('Ctrl Pts',(-7.46493895531249,2.61890474916414,46.527386884856));
#63862=CARTESIAN_POINT('Ctrl Pts',(-7.46248747642138,2.62588201494009,46.527090480468));
#63863=CARTESIAN_POINT('Ctrl Pts',(-7.45806913171659,2.63840110798912,46.5265589874387));
#63864=CARTESIAN_POINT('Ctrl Pts',(-7.45610586545242,2.643944194469,46.5263237764266));
#63865=CARTESIAN_POINT('Ctrl Pts',(-7.45192400210159,2.65570956728015,46.5258247839785));
#63866=CARTESIAN_POINT('Ctrl Pts',(-7.44970378740904,2.66193127615737,46.5255610579146));
#63867=CARTESIAN_POINT('Ctrl Pts',(-7.44374982469739,2.67855027795454,46.5248570059581));
#63868=CARTESIAN_POINT('Ctrl Pts',(-7.44000208008678,2.68894256052886,46.5244171580344));
#63869=CARTESIAN_POINT('Ctrl Pts',(-7.42223573341392,2.73788612550479,46.5223475743764));
#63870=CARTESIAN_POINT('Ctrl Pts',(-7.40793906652687,2.77633617762917,46.5207273565077));
#63871=CARTESIAN_POINT('Ctrl Pts',(-7.297212151716,3.06718415758546,46.5085122452187));
#63872=CARTESIAN_POINT('Ctrl Pts',(-7.18820392417193,3.3146136978331,46.498363355946));
#63873=CARTESIAN_POINT('Ctrl Pts',(-6.98485245377564,3.71872894532755,46.4819508092894));
#63874=CARTESIAN_POINT('Ctrl Pts',(-6.89736631882546,3.87858863735505,46.4755013145465));
#63875=CARTESIAN_POINT('Ctrl Pts',(-6.44059589898921,4.64880988279558,46.4442768187746));
#63876=CARTESIAN_POINT('Ctrl Pts',(-5.99551034410751,5.21021025676115,46.4213247839597));
#63877=CARTESIAN_POINT('Ctrl Pts',(-5.42483124581693,5.75858182976693,46.3907942880829));
#63878=CARTESIAN_POINT('Ctrl Pts',(-5.36753929600187,5.81202029270604,46.3877157275242));
#63879=CARTESIAN_POINT('Ctrl Pts',(-5.30302508156673,5.87042770581425,46.3842217127422));
#63880=CARTESIAN_POINT('Ctrl Pts',(-5.29657560216107,5.87624738710179,46.3838721174856));
#63881=CARTESIAN_POINT('Ctrl Pts',(-5.28692053861367,5.88493081482364,46.3833482935992));
#63882=CARTESIAN_POINT('Ctrl Pts',(-5.28372216886451,5.88780260529554,46.3831746931267));
#63883=CARTESIAN_POINT('Ctrl Pts',(-5.278212903992,5.89274122562593,46.382875527095));
#63884=CARTESIAN_POINT('Ctrl Pts',(-5.27590312885451,5.89480930878551,46.3827500600273));
#63885=CARTESIAN_POINT('Ctrl Pts',(-5.27138136491089,5.89885313447831,46.3825043563886));
#63886=CARTESIAN_POINT('Ctrl Pts',(-5.26916947852634,5.90082899286552,46.3823841288657));
#63887=CARTESIAN_POINT('Ctrl Pts',(-5.2638057828561,5.90561491385036,46.3820924908241));
#63888=CARTESIAN_POINT('Ctrl Pts',(-5.26065284231471,5.90842369019273,46.381920979579));
#63889=CARTESIAN_POINT('Ctrl Pts',(-5.25088495113326,5.91711133482769,46.3813893973857));
#63890=CARTESIAN_POINT('Ctrl Pts',(-5.24426240363179,5.92298161059053,46.3810286546541));
#63891=CARTESIAN_POINT('Ctrl Pts',(-5.1679372087861,5.9904084738627,46.3768673837861));
#63892=CARTESIAN_POINT('Ctrl Pts',(-5.09716683176234,6.05074025532961,46.3729736168872));
#63893=CARTESIAN_POINT('Ctrl Pts',(-4.88192826333345,6.22777521300063,46.3610720092556));
#63894=CARTESIAN_POINT('Ctrl Pts',(-4.73440247048313,6.34064927503365,46.352837676472));
#63895=CARTESIAN_POINT('Ctrl Pts',(-4.46337130879253,6.53328374006013,46.3377777014192));
#63896=CARTESIAN_POINT('Ctrl Pts',(-4.34134906041434,6.61499555204926,46.3310204994258));
#63897=CARTESIAN_POINT('Ctrl Pts',(-3.49298096863515,7.14951456207522,46.2845324041616));
#63898=CARTESIAN_POINT('Ctrl Pts',(-2.69936282276075,7.48535612077804,46.2442984558652));
#63899=CARTESIAN_POINT('Ctrl Pts',(-1.85649704577245,7.69008862549486,46.2087296599851));
#63900=CARTESIAN_POINT('Ctrl Pts',(-1.84569906945247,7.69268739097793,46.2082749694832));
#63901=CARTESIAN_POINT('Ctrl Pts',(-1.78849040537241,7.70632850003853,46.2058711600591));
#63902=CARTESIAN_POINT('Ctrl Pts',(-1.74198552169552,7.71697372224957,46.2039351611053));
#63903=CARTESIAN_POINT('Ctrl Pts',(-1.68456262408075,7.72957259908383,46.2015664568519));
#63904=CARTESIAN_POINT('Ctrl Pts',(-1.67373361219453,7.73192470188996,46.2011207108942));
#63905=CARTESIAN_POINT('Ctrl Pts',(-1.65577123031196,7.73578669538184,46.2003829104312));
#63906=CARTESIAN_POINT('Ctrl Pts',(-1.64864066816913,7.73730948787828,46.2000904342727));
#63907=CARTESIAN_POINT('Ctrl Pts',(-1.63572194474264,7.74004972233167,46.1995612832223));
#63908=CARTESIAN_POINT('Ctrl Pts',(-1.62993450839717,7.74127053417047,46.1993244984206));
#63909=CARTESIAN_POINT('Ctrl Pts',(-1.61751803436322,7.74387514538855,46.1988170702665));
#63910=CARTESIAN_POINT('Ctrl Pts',(-1.61088857549813,7.74525692643482,46.1985464929168));
#63911=CARTESIAN_POINT('Ctrl Pts',(-1.5928618230011,7.74899010451011,46.1978116923082));
#63912=CARTESIAN_POINT('Ctrl Pts',(-1.58146108140003,7.75132487233656,46.1973480111531));
#63913=CARTESIAN_POINT('Ctrl Pts',(-1.52400651907369,7.76295900783842,46.1950164322002));
#63914=CARTESIAN_POINT('Ctrl Pts',(-1.47787519801554,7.77187322495033,46.1931610734125));
#63915=CARTESIAN_POINT('Ctrl Pts',(-0.861703263717836,7.88525499710756,
46.1685949703723));
#63916=CARTESIAN_POINT('Ctrl Pts',(-0.281909987949086,7.92719266148348,
46.1481175039457));
#63917=CARTESIAN_POINT('Ctrl Pts',(0.913190984529806,7.88225130730059,46.1068526519513));
#63918=CARTESIAN_POINT('Ctrl Pts',(1.52422085831935,7.78719430407909,46.0862059904786));
#63919=CARTESIAN_POINT('Ctrl Pts',(2.15698672618239,7.61137118503577,46.0603227078197));
#63920=CARTESIAN_POINT('Ctrl Pts',(2.19594527966792,7.6002228444951,46.0587101162482));
#63921=CARTESIAN_POINT('Ctrl Pts',(2.24301494424486,7.58636131584293,46.056740100674));
#63922=CARTESIAN_POINT('Ctrl Pts',(2.25121006411208,7.58393349793206,46.0563963101428));
#63923=CARTESIAN_POINT('Ctrl Pts',(2.26463828169596,7.57993168279835,46.0558316950643));
#63924=CARTESIAN_POINT('Ctrl Pts',(2.2698737245545,7.57836553203345,46.0556112383551));
#63925=CARTESIAN_POINT('Ctrl Pts',(2.2792517449345,7.57554956463676,46.05521577069));
#63926=CARTESIAN_POINT('Ctrl Pts',(2.28339493388027,7.57430176972607,46.0550408533146));
#63927=CARTESIAN_POINT('Ctrl Pts',(2.29217189898423,7.57165057480612,46.0546698845663));
#63928=CARTESIAN_POINT('Ctrl Pts',(2.29680541333091,7.5702463192816,46.054473794013));
#63929=CARTESIAN_POINT('Ctrl Pts',(2.30914104328809,7.56649545506043,46.0539510896322));
#63930=CARTESIAN_POINT('Ctrl Pts',(2.31684085753181,7.56414134382935,46.0536241356687));
#63931=CARTESIAN_POINT('Ctrl Pts',(2.35264932870897,7.55313359599738,46.0521004647042));
#63932=CARTESIAN_POINT('Ctrl Pts',(2.38071294319059,7.54433508220576,46.0508973021609));
#63933=CARTESIAN_POINT('Ctrl Pts',(2.60197850094645,7.47360630634047,46.041342815864));
#63934=CARTESIAN_POINT('Ctrl Pts',(2.79277414490122,7.4044235575911,46.0326938461278));
#63935=CARTESIAN_POINT('Ctrl Pts',(3.22446827900906,7.22883016791315,46.0124586444502));
#63936=CARTESIAN_POINT('Ctrl Pts',(3.46314286350154,7.11757107945948,46.0007791008091));
#63937=CARTESIAN_POINT('Ctrl Pts',(4.19763249220316,6.72948117965616,45.9639180252363));
#63938=CARTESIAN_POINT('Ctrl Pts',(4.669495826522,6.41108034137121,45.9389874647248));
#63939=CARTESIAN_POINT('Ctrl Pts',(5.20715117939874,5.95717971262762,45.9097967707891));
#63940=CARTESIAN_POINT('Ctrl Pts',(5.30878376596204,5.8667904422558,45.9042300245248));
#63941=CARTESIAN_POINT('Ctrl Pts',(5.42499351155148,5.75794287037197,45.8977967636495));
#63942=CARTESIAN_POINT('Ctrl Pts',(5.4418789296379,5.74198697507092,45.8968602493102));
#63943=CARTESIAN_POINT('Ctrl Pts',(5.46653378574503,5.71848290140706,45.8954901481128));
#63944=CARTESIAN_POINT('Ctrl Pts',(5.47435834592267,5.71099282310811,45.8950549297332));
#63945=CARTESIAN_POINT('Ctrl Pts',(5.48888579158408,5.69702910319105,45.8942461291335));
#63946=CARTESIAN_POINT('Ctrl Pts',(5.4955926655259,5.69055964653082,45.893872430287));
#63947=CARTESIAN_POINT('Ctrl Pts',(5.50947502443996,5.67712127823062,45.8930982893552));
#63948=CARTESIAN_POINT('Ctrl Pts',(5.51664875741477,5.67015057477277,45.8926978988815));
#63949=CARTESIAN_POINT('Ctrl Pts',(5.53469668729099,5.6525467613961,45.8916896910601));
#63950=CARTESIAN_POINT('Ctrl Pts',(5.54555349162488,5.64189585013542,45.8910823805571));
#63951=CARTESIAN_POINT('Ctrl Pts',(5.5877592145323,5.60025100607808,45.8887182447351));
#63952=CARTESIAN_POINT('Ctrl Pts',(5.61887974011862,5.56902638615567,45.8869680838066));
#63953=CARTESIAN_POINT('Ctrl Pts',(6.10597322674262,5.07206401770137,45.8594613266564));
#63954=CARTESIAN_POINT('Ctrl Pts',(6.50293373993015,4.55199442557474,45.8357478942767));
#63955=CARTESIAN_POINT('Ctrl Pts',(7.01167929093169,3.68073219414796,45.7992666486995));
#63956=CARTESIAN_POINT('Ctrl Pts',(7.17064921264867,3.36053635601431,45.7863750327625));
#63957=CARTESIAN_POINT('Ctrl Pts',(7.36571052391028,2.89021870949779,45.7670193450199));
#63958=CARTESIAN_POINT('Ctrl Pts',(7.41991438851238,2.74807614357545,45.7611148644146));
#63959=CARTESIAN_POINT('Ctrl Pts',(7.474518538081,2.59146353117678,45.7544729172857));
#63960=CARTESIAN_POINT('Ctrl Pts',(7.47901789270622,2.57844952766289,45.7539199755146));
#63961=CARTESIAN_POINT('Ctrl Pts',(7.48528323891336,2.56017316670389,45.7531419433922));
#63962=CARTESIAN_POINT('Ctrl Pts',(7.48707772137369,2.55492054752367,45.7529181634396));
#63963=CARTESIAN_POINT('Ctrl Pts',(7.49017971754867,2.54580937952081,45.7525296883565));
#63964=CARTESIAN_POINT('Ctrl Pts',(7.49148978289561,2.5419516971622,45.7523651119298));
#63965=CARTESIAN_POINT('Ctrl Pts',(7.4942069597042,2.53393022048807,45.7520226983557));
#63966=CARTESIAN_POINT('Ctrl Pts',(7.49561358201777,2.5297662631423,45.7518448383831));
#63967=CARTESIAN_POINT('Ctrl Pts',(7.49891342968008,2.51997096620334,45.7514261712736));
#63968=CARTESIAN_POINT('Ctrl Pts',(7.50080378112076,2.51433866716033,45.7511852284825));
#63969=CARTESIAN_POINT('Ctrl Pts',(7.50694333966711,2.4959773195483,45.7503990574407));
#63970=CARTESIAN_POINT('Ctrl Pts',(7.51116648660083,2.48323963640294,45.7498525846053));
#63971=CARTESIAN_POINT('Ctrl Pts',(7.58591865523912,2.25583983112144,45.7400763699094));
#63972=CARTESIAN_POINT('Ctrl Pts',(7.64723913392699,2.03830237605796,45.7303502927874));
#63973=CARTESIAN_POINT('Ctrl Pts',(7.76152100632742,1.55444819737674,45.7082807016921));
#63974=CARTESIAN_POINT('Ctrl Pts',(7.81025641844645,1.28740138768795,45.6958361691029));
#63975=CARTESIAN_POINT('Ctrl Pts',(7.92593911433649,0.396238513383225,45.654435083206));
#63976=CARTESIAN_POINT('Ctrl Pts',(7.93241723087277,-0.233403940133185,
45.6256025219132));
#63977=CARTESIAN_POINT('Ctrl Pts',(7.84898678516317,-0.998801405390404,
45.5932007595034));
#63978=CARTESIAN_POINT('Ctrl Pts',(7.8297368825879,-1.1399214798817,45.5873262442997));
#63979=CARTESIAN_POINT('Ctrl Pts',(7.80413312575725,-1.29602322332292,45.5809365107599));
#63980=CARTESIAN_POINT('Ctrl Pts',(7.80153225977172,-1.31158851912749,45.5803005694811));
#63981=CARTESIAN_POINT('Ctrl Pts',(7.79757372224525,-1.33485060069996,45.579351938966));
#63982=CARTESIAN_POINT('Ctrl Pts',(7.79625119987939,-1.34255327971313,45.5790381137884));
#63983=CARTESIAN_POINT('Ctrl Pts',(7.79395476609153,-1.35581042345275,45.5784984856089));
#63984=CARTESIAN_POINT('Ctrl Pts',(7.79298632719306,-1.36136582320463,45.5782725055903));
#63985=CARTESIAN_POINT('Ctrl Pts',(7.79102944821688,-1.37252084488801,45.5778190488207));
#63986=CARTESIAN_POINT('Ctrl Pts',(7.79004090927039,-1.37812044637269,45.5775915754188));
#63987=CARTESIAN_POINT('Ctrl Pts',(7.78771526711517,-1.39121164097026,45.5770601264804));
#63988=CARTESIAN_POINT('Ctrl Pts',(7.78637338861701,-1.39870238617536,45.5767563060061));
#63989=CARTESIAN_POINT('Ctrl Pts',(7.78222143640404,-1.42168861592112,45.5758248316491));
#63990=CARTESIAN_POINT('Ctrl Pts',(7.77937589209213,-1.43717769922888,45.575198329775));
#63991=CARTESIAN_POINT('Ctrl Pts',(7.77273428597815,-1.47273206631784,45.5737628740745));
#63992=CARTESIAN_POINT('Ctrl Pts',(7.76890673687844,-1.49279139245896,45.5729549464495));
#63993=CARTESIAN_POINT('Ctrl Pts',(7.75605221739652,-1.55877037406356,45.5703037979563));
#63994=CARTESIAN_POINT('Ctrl Pts',(7.74669538087286,-1.60462514319323,45.5684713097729));
#63995=CARTESIAN_POINT('Ctrl Pts',(7.70809557262344,-1.78557827825945,45.5612778532947));
#63996=CARTESIAN_POINT('Ctrl Pts',(7.67572027569065,-1.91998637657885,45.5560191575296));
#63997=CARTESIAN_POINT('Ctrl Pts',(7.5572423811868,-2.36077534942246,45.5389984784802));
#63998=CARTESIAN_POINT('Ctrl Pts',(7.45617839012619,-2.66281700518543,45.5277125431495));
#63999=CARTESIAN_POINT('Ctrl Pts',(7.05081962363052,-3.66830421336438,45.4902524071992));
#64000=CARTESIAN_POINT('Ctrl Pts',(6.66286385744881,-4.33317394317613,45.4659487454483));
#64001=CARTESIAN_POINT('Ctrl Pts',(6.1570504070919,-4.96756882408057,45.4341102630803));
#64002=CARTESIAN_POINT('Ctrl Pts',(6.1282500762851,-5.00305512475781,45.4322959701446));
#64003=CARTESIAN_POINT('Ctrl Pts',(6.09400688259133,-5.04450851810304,45.4301345773901));
#64004=CARTESIAN_POINT('Ctrl Pts',(6.08885983706439,-5.05071994451675,45.4298095908552));
#64005=CARTESIAN_POINT('Ctrl Pts',(6.08106912539896,-5.06009251634561,45.429317497388));
#64006=CARTESIAN_POINT('Ctrl Pts',(6.07843246151705,-5.06325950278151,45.4291509229686));
#64007=CARTESIAN_POINT('Ctrl Pts',(6.07370712396299,-5.06892625550477,45.4288523342598));
#64008=CARTESIAN_POINT('Ctrl Pts',(6.07161938063593,-5.07142679213555,45.4287203911295));
#64009=CARTESIAN_POINT('Ctrl Pts',(6.06717589532666,-5.07674217664295,45.428439524317));
#64010=CARTESIAN_POINT('Ctrl Pts',(6.06481973653262,-5.07955667713375,45.4282905688284));
#64011=CARTESIAN_POINT('Ctrl Pts',(6.05850097178466,-5.08709396236088,45.4278910323727));
#64012=CARTESIAN_POINT('Ctrl Pts',(6.054534809528,-5.09181374824342,45.4276401813974));
#64013=CARTESIAN_POINT('Ctrl Pts',(6.03564059798249,-5.11424482294583,45.426444854311));
#64014=CARTESIAN_POINT('Ctrl Pts',(6.02064046423679,-5.13189496344394,45.4254949642154));
#64015=CARTESIAN_POINT('Ctrl Pts',(5.90179979410298,-5.2704925151697,45.4179640613292));
#64016=CARTESIAN_POINT('Ctrl Pts',(5.79440809085358,-5.38833566026056,45.4111276596962));
#64017=CARTESIAN_POINT('Ctrl Pts',(5.51159632250249,-5.68043374446661,45.3932448792176));
#64018=CARTESIAN_POINT('Ctrl Pts',(5.33143392529485,-5.84985666971853,45.381966115217));
#64019=CARTESIAN_POINT('Ctrl Pts',(4.90968882997884,-6.21077272332795,45.3563698009899));
#64020=CARTESIAN_POINT('Ctrl Pts',(4.66423628909521,-6.39715936237836,45.3420144150289));
#64021=CARTESIAN_POINT('Ctrl Pts',(4.25220900332335,-6.67368628899001,45.3193078912122));
#64022=CARTESIAN_POINT('Ctrl Pts',(4.09217402739796,-6.77299686490314,45.3107950521843));
#64023=CARTESIAN_POINT('Ctrl Pts',(3.62838649368195,-7.03835770825675,45.2871052565214));
#64024=CARTESIAN_POINT('Ctrl Pts',(3.31705913369678,-7.19032873371709,45.2723645640927));
#64025=CARTESIAN_POINT('Ctrl Pts',(2.97634459470573,-7.32978716892991,45.2574746943218));
#64026=CARTESIAN_POINT('Ctrl Pts',(2.95590532800878,-7.33805361050666,45.2565859602549));
#64027=CARTESIAN_POINT('Ctrl Pts',(2.92791593522201,-7.34923770069508,45.2553750337002));
#64028=CARTESIAN_POINT('Ctrl Pts',(2.92039559333514,-7.35222932748834,45.2550502755954));
#64029=CARTESIAN_POINT('Ctrl Pts',(2.90758469989985,-7.35730280310246,45.2544980688529));
#64030=CARTESIAN_POINT('Ctrl Pts',(2.9022964782286,-7.35939049624918,45.2542704178399));
#64031=CARTESIAN_POINT('Ctrl Pts',(2.89162195904045,-7.36359130610247,45.2538114874263));
#64032=CARTESIAN_POINT('Ctrl Pts',(2.88623558428345,-7.36570421816687,45.2535802151997));
#64033=CARTESIAN_POINT('Ctrl Pts',(2.87396777603052,-7.37050098564255,45.2530541697056));
#64034=CARTESIAN_POINT('Ctrl Pts',(2.86708488741413,-7.37318111847072,45.2527595252431));
#64035=CARTESIAN_POINT('Ctrl Pts',(2.85268227748764,-7.37876614400655,45.2521440059178));
#64036=CARTESIAN_POINT('Ctrl Pts',(2.84516184709727,-7.38166919121668,45.251823194944));
#64037=CARTESIAN_POINT('Ctrl Pts',(2.82542251125756,-7.38925435047484,45.2509826764563));
#64038=CARTESIAN_POINT('Ctrl Pts',(2.81319638024109,-7.39391765923138,45.2504636166194));
#64039=CARTESIAN_POINT('Ctrl Pts',(2.77684453014169,-7.40767981830832,45.2489248429259));
#64040=CARTESIAN_POINT('Ctrl Pts',(2.75268573096859,-7.41669111653112,45.2479081335978));
#64041=CARTESIAN_POINT('Ctrl Pts',(2.66827793293182,-7.44770621905748,45.2443762648857));
#64042=CARTESIAN_POINT('Ctrl Pts',(2.60780505751807,-7.46909553284978,45.2418820329771));
#64043=CARTESIAN_POINT('Ctrl Pts',(2.4419024015777,-7.52551492229622,45.2351336541947));
#64044=CARTESIAN_POINT('Ctrl Pts',(2.3359830622578,-7.55906386269258,45.2309285433124));
#64045=CARTESIAN_POINT('Ctrl Pts',(2.05200853661971,-7.64247082593702,45.2199011537339));
#64046=CARTESIAN_POINT('Ctrl Pts',(1.87285108944981,-7.68833742397841,45.2132001200689));
#64047=CARTESIAN_POINT('Ctrl Pts',(1.28506628606805,-7.81704999288738,45.1918267063637));
#64048=CARTESIAN_POINT('Ctrl Pts',(0.871470791927446,-7.87389405945192,
45.1777695756254));
#64049=CARTESIAN_POINT('Ctrl Pts',(0.0127080435581117,-7.92340366721502,
45.1481782554769));
#64050=CARTESIAN_POINT('Ctrl Pts',(-0.431233234309826,-7.91166491045866,
45.1326436203546));
#64051=CARTESIAN_POINT('Ctrl Pts',(-0.899818011444226,-7.85971013223619,
45.1139671089807));
#64052=CARTESIAN_POINT('Ctrl Pts',(-0.927821650962073,-7.85645357414792,
45.1128421240603));
#64053=CARTESIAN_POINT('Ctrl Pts',(-0.962050147412785,-7.85228756915941,
45.1114556154184));
#64054=CARTESIAN_POINT('Ctrl Pts',(-0.968292429254012,-7.85152025574219,
45.1112022900556));
#64055=CARTESIAN_POINT('Ctrl Pts',(-0.978625524780857,-7.85023758127673,
45.1107821692991));
#64056=CARTESIAN_POINT('Ctrl Pts',(-0.982716850587435,-7.84972646604264,
45.1106156226619));
#64057=CARTESIAN_POINT('Ctrl Pts',(-0.989803761351205,-7.84883549527352,
45.1103267856339));
#64058=CARTESIAN_POINT('Ctrl Pts',(-0.992799535337517,-7.84845712229003,
45.1102045807844));
#64059=CARTESIAN_POINT('Ctrl Pts',(-0.99950588677319,-7.84760619386737,
45.1099307722018));
#64060=CARTESIAN_POINT('Ctrl Pts',(-1.00321634597973,-7.84713272187991,
45.1097791159097));
#64061=CARTESIAN_POINT('Ctrl Pts',(-1.01302232219203,-7.84587436466876,
45.109377886866));
#64062=CARTESIAN_POINT('Ctrl Pts',(-1.01911725193471,-7.84508500896157,
45.1091280597903));
#64063=CARTESIAN_POINT('Ctrl Pts',(-1.04669353182927,-7.84148092021652,
45.107995745496));
#64064=CARTESIAN_POINT('Ctrl Pts',(-1.06816400425993,-7.83858507732715,
45.1071087016272));
#64065=CARTESIAN_POINT('Ctrl Pts',(-1.22762586692925,-7.81641024104995,
45.1004815696595));
#64066=CARTESIAN_POINT('Ctrl Pts',(-1.36509184669648,-7.7935777830643,45.0945514412104));
#64067=CARTESIAN_POINT('Ctrl Pts',(-1.64282285221011,-7.73987486413295,
45.0822285833282));
#64068=CARTESIAN_POINT('Ctrl Pts',(-1.78299715113025,-7.70879031179902,
45.0758295594722));
#64069=CARTESIAN_POINT('Ctrl Pts',(-2.2850066613363,-7.58304163453388,45.0524424394893));
#64070=CARTESIAN_POINT('Ctrl Pts',(-2.64086672672486,-7.46656523303081,
45.0349969617625));
#64071=CARTESIAN_POINT('Ctrl Pts',(-3.17638800541315,-7.24818914115788,
45.0084324763907));
#64072=CARTESIAN_POINT('Ctrl Pts',(-3.36256915990343,-7.16371553180975,
44.9991296066186));
#64073=CARTESIAN_POINT('Ctrl Pts',(-3.89622209013668,-6.89619383659496,
44.9724562400596));
#64074=CARTESIAN_POINT('Ctrl Pts',(-4.23361160688387,-6.69437270348464,
44.9556128660747));
#64075=CARTESIAN_POINT('Ctrl Pts',(-4.57622662745964,-6.45312071604315,
44.9386252568006));
#64076=CARTESIAN_POINT('Ctrl Pts',(-4.59772321238927,-6.43782248911711,
44.9375597377885));
#64077=CARTESIAN_POINT('Ctrl Pts',(-4.62719905411467,-6.41662281773909,
44.9360990903914));
#64078=CARTESIAN_POINT('Ctrl Pts',(-4.63524421934644,-6.41081355987418,
44.9357004588083));
#64079=CARTESIAN_POINT('Ctrl Pts',(-4.64803139755435,-6.40154353185536,
44.935066921038));
#64080=CARTESIAN_POINT('Ctrl Pts',(-4.65278051294209,-6.3980926033829,44.934831639726));
#64081=CARTESIAN_POINT('Ctrl Pts',(-4.66240442312029,-6.39108303987759,
44.9343548745983));
#64082=CARTESIAN_POINT('Ctrl Pts',(-4.66727899598378,-6.3875241057237,44.9341134024499));
#64083=CARTESIAN_POINT('Ctrl Pts',(-4.67844563869341,-6.37935171312257,
44.9335602662545));
#64084=CARTESIAN_POINT('Ctrl Pts',(-4.68473497043451,-6.37473451456304,
44.9332487456852));
#64085=CARTESIAN_POINT('Ctrl Pts',(-4.69790243907058,-6.36503784610155,
44.9325965772672));
#64086=CARTESIAN_POINT('Ctrl Pts',(-4.70477919435659,-6.35995651260747,
44.9322560014181));
#64087=CARTESIAN_POINT('Ctrl Pts',(-4.72289860424831,-6.34652235009006,
44.9313586753923));
#64088=CARTESIAN_POINT('Ctrl Pts',(-4.73412736029245,-6.33815077962664,
44.9308026453174));
#64089=CARTESIAN_POINT('Ctrl Pts',(-4.76764816537428,-6.31302065184092,
44.9291428655593));
#64090=CARTESIAN_POINT('Ctrl Pts',(-4.78987399083888,-6.29617391366351,
44.9280425119272));
#64091=CARTESIAN_POINT('Ctrl Pts',(-4.86784613495153,-6.23642073199929,
44.924182470146));
#64092=CARTESIAN_POINT('Ctrl Pts',(-4.9231094534904,-6.19288811105501,44.9214470261026));
#64093=CARTESIAN_POINT('Ctrl Pts',(-5.23434407602938,-5.9409196417508,44.9060323172904));
#64094=CARTESIAN_POINT('Ctrl Pts',(-5.47766144267767,-5.71735353500339,
44.8939648016532));
#64095=CARTESIAN_POINT('Ctrl Pts',(-6.24443266890608,-4.91880369379686,
44.8546951624153));
#64096=CARTESIAN_POINT('Ctrl Pts',(-6.6969699804357,-4.2822659340079,44.8296507195791));
#64097=CARTESIAN_POINT('Ctrl Pts',(-7.06877571347331,-3.55220259280201,
44.7974216999255));
#64098=CARTESIAN_POINT('Ctrl Pts',(-7.08778856981776,-3.51411246498051,
44.7957299784945));
#64099=CARTESIAN_POINT('Ctrl Pts',(-7.10978015125898,-3.46915021033776,
44.7937190273155));
#64100=CARTESIAN_POINT('Ctrl Pts',(-7.11305800903638,-3.46242440214129,
44.793417846661));
#64101=CARTESIAN_POINT('Ctrl Pts',(-7.1182939215366,-3.45164206373017,44.7929344128781));
#64102=CARTESIAN_POINT('Ctrl Pts',(-7.12025806742463,-3.44758848219771,
44.792752531502));
#64103=CARTESIAN_POINT('Ctrl Pts',(-7.12373126898598,-3.44040490080144,
44.7924299644162));
#64104=CARTESIAN_POINT('Ctrl Pts',(-7.12524172834748,-3.43727557620928,
44.7922893648894));
#64105=CARTESIAN_POINT('Ctrl Pts',(-7.12838853690268,-3.43074512492742,
44.7919957807693));
#64106=CARTESIAN_POINT('Ctrl Pts',(-7.13002451025928,-3.4273438298877,44.7918427739743));
#64107=CARTESIAN_POINT('Ctrl Pts',(-7.13427970521626,-3.41848077060412,
44.791443819028));
#64108=CARTESIAN_POINT('Ctrl Pts',(-7.13689508495794,-3.41301717504889,
44.7911976364068));
#64109=CARTESIAN_POINT('Ctrl Pts',(-7.14812995048461,-3.38947787103691,
44.7901359340581));
#64110=CARTESIAN_POINT('Ctrl Pts',(-7.15668699532723,-3.37137260843522,
44.7893166580578));
#64111=CARTESIAN_POINT('Ctrl Pts',(-7.21660884791525,-3.24333191274209,
44.7835049994685));
#64112=CARTESIAN_POINT('Ctrl Pts',(-7.26550494932593,-3.13226442378221,
44.778371841829));
#64113=CARTESIAN_POINT('Ctrl Pts',(-7.70724254340192,-2.06280148467221,
44.7283908523604));
#64114=CARTESIAN_POINT('Ctrl Pts',(-7.91088113128406,-1.03708363487558,
44.6779412040058));
#64115=CARTESIAN_POINT('Ctrl Pts',(-7.91099994798975,-0.000907141745418172,
44.6351174622069));
#64116=CARTESIAN_POINT('',(-7.90852312217059,0.00709379171421498,42.6423315082371));
#64117=CARTESIAN_POINT('Ctrl Pts',(-7.89861493486562,-0.000610740782857052,
44.6422669711751));
#64118=CARTESIAN_POINT('Ctrl Pts',(-7.8954795751415,1.45177507856196,44.5840303434289));
#64119=CARTESIAN_POINT('Ctrl Pts',(-6.81619969976293,5.55073973453917,44.4198593358802));
#64120=CARTESIAN_POINT('Ctrl Pts',(-0.210945049882454,9.354012036458,44.1497539485288));
#64121=CARTESIAN_POINT('Ctrl Pts',(6.40488750778627,5.92654785945168,43.8849179990226));
#64122=CARTESIAN_POINT('Ctrl Pts',(8.18512056268212,0.79234657492906,43.6730492394173));
#64123=CARTESIAN_POINT('Ctrl Pts',(7.4227292473118,-4.58798910622404,43.4611804798124));
#64124=CARTESIAN_POINT('Ctrl Pts',(1.58715686282455,-9.22079020936372,43.1963445303059));
#64125=CARTESIAN_POINT('Ctrl Pts',(-6.17232811875731,-6.56794650215052,
42.9057391431469));
#64126=CARTESIAN_POINT('Ctrl Pts',(-7.89172359999745,-1.9501472650058,42.7210681357908));
#64127=CARTESIAN_POINT('Ctrl Pts',(-7.90852312217059,0.00709379171421498,
42.6423315082371));
#64128=CARTESIAN_POINT('',(-7.92071738904598,-0.000648184374720526,40.6423303528761));
#64129=CARTESIAN_POINT('Ctrl Pts',(-7.91099681685684,0.00709673735080949,
42.6423314790088));
#64130=CARTESIAN_POINT('Ctrl Pts',(-7.9107752173155,0.254121980005545,42.6323970776905));
#64131=CARTESIAN_POINT('Ctrl Pts',(-7.89897987247902,0.500645992443577,
42.6224626763721));
#64132=CARTESIAN_POINT('Ctrl Pts',(-7.87577275734792,0.745737537352352,
42.6125282750538));
#64133=CARTESIAN_POINT('Ctrl Pts',(-7.85215362603152,0.995180406534389,
42.6024174996316));
#64134=CARTESIAN_POINT('Ctrl Pts',(-7.81671393357025,1.24313964973455,42.5923067242094));
#64135=CARTESIAN_POINT('Ctrl Pts',(-7.76967306550624,1.488657601716,42.5821959487873));
#64136=CARTESIAN_POINT('Ctrl Pts',(-7.73639540989157,1.66234193598769,42.5750433830217));
#64137=CARTESIAN_POINT('Ctrl Pts',(-7.69731303644139,1.8348050543254,42.5678908172562));
#64138=CARTESIAN_POINT('Ctrl Pts',(-7.6525179617014,2.00571429815851,42.5607382514906));
#64139=CARTESIAN_POINT('Ctrl Pts',(-7.60297192480338,2.19475016315747,42.5528270851539));
#64140=CARTESIAN_POINT('Ctrl Pts',(-7.54635066681069,2.38220313786713,42.5449159188171));
#64141=CARTESIAN_POINT('Ctrl Pts',(-7.48276962060389,2.5675045871366,42.5370047524803));
#64142=CARTESIAN_POINT('Ctrl Pts',(-7.41925749423832,2.75260517550139,42.5291021615975));
#64143=CARTESIAN_POINT('Ctrl Pts',(-7.3488007174694,2.93555856057317,42.5211995707145));
#64144=CARTESIAN_POINT('Ctrl Pts',(-7.2715653994801,3.11580770284107,42.5132969798316));
#64145=CARTESIAN_POINT('Ctrl Pts',(-7.19439946509978,3.29589492001654,42.5054014881656));
#64146=CARTESIAN_POINT('Ctrl Pts',(-7.1104672551568,3.47328241886557,42.4975059964996));
#64147=CARTESIAN_POINT('Ctrl Pts',(-7.01998429752439,3.64742943214957,42.4896105048336));
#64148=CARTESIAN_POINT('Ctrl Pts',(-6.92956583344602,3.82145231863552,42.4817206408387));
#64149=CARTESIAN_POINT('Ctrl Pts',(-6.83260608261984,3.99223901657015,42.4738307768437));
#64150=CARTESIAN_POINT('Ctrl Pts',(-6.72936829589034,4.15926956787679,42.4659409128487));
#64151=CARTESIAN_POINT('Ctrl Pts',(-6.62618494040187,4.32621205375229,42.4580552087171));
#64152=CARTESIAN_POINT('Ctrl Pts',(-6.51673032558461,4.48940204658587,42.4501695045855));
#64153=CARTESIAN_POINT('Ctrl Pts',(-6.4013133068748,4.64834475348243,42.442283800454));
#64154=CARTESIAN_POINT('Ctrl Pts',(-6.28593573112009,4.80723314282581,42.4344007912063));
#64155=CARTESIAN_POINT('Ctrl Pts',(-6.16460001487929,4.9618768604002,42.4265177819587));
#64156=CARTESIAN_POINT('Ctrl Pts',(-6.03765809640805,5.11181041421513,42.4186347727111));
#64157=CARTESIAN_POINT('Ctrl Pts',(-5.91071425287239,5.26174624176087,42.4107516439183));
#64158=CARTESIAN_POINT('Ctrl Pts',(-5.77816425357656,5.40697149421105,42.4028685151254));
#64159=CARTESIAN_POINT('Ctrl Pts',(-5.64040042235492,5.54705363914019,42.3949853863326));
#64160=CARTESIAN_POINT('Ctrl Pts',(-5.50262805231716,5.68714446657814,42.3871017689311));
#64161=CARTESIAN_POINT('Ctrl Pts',(-5.35964144792159,5.82209130486687,42.3792181515297));
#64162=CARTESIAN_POINT('Ctrl Pts',(-5.21186992463021,5.95149837341279,42.3713345341283));
#64163=CARTESIAN_POINT('Ctrl Pts',(-5.06406440262239,6.08093521545046,42.3634491028939));
#64164=CARTESIAN_POINT('Ctrl Pts',(-4.91147202751804,6.2048295207068,42.3555636716594));
#64165=CARTESIAN_POINT('Ctrl Pts',(-4.75455550521427,6.32282555095716,42.347678240425));
#64166=CARTESIAN_POINT('Ctrl Pts',(-4.59757650297498,6.44086856405071,42.3397896694241));
#64167=CARTESIAN_POINT('Ctrl Pts',(-4.43627019823336,6.55300841532703,42.3319010984231));
#64168=CARTESIAN_POINT('Ctrl Pts',(-4.27112878713447,6.65893233812383,42.3240125274222));
#64169=CARTESIAN_POINT('Ctrl Pts',(-4.10581159260935,6.76496901077509,42.3161155594963));
#64170=CARTESIAN_POINT('Ctrl Pts',(-3.93665142823722,6.86477635285342,42.3082185915704));
#64171=CARTESIAN_POINT('Ctrl Pts',(-3.76416659665973,6.95808672212348,42.3003216236445));
#64172=CARTESIAN_POINT('Ctrl Pts',(-3.59157655001415,7.05145401035138,42.2924198385993));
#64173=CARTESIAN_POINT('Ctrl Pts',(-3.41565810142144,7.13831627243318,42.284518053554));
#64174=CARTESIAN_POINT('Ctrl Pts',(-3.23695033211913,7.21845368118365,42.2766162685088));
#64175=CARTESIAN_POINT('Ctrl Pts',(-3.05801139796657,7.29869475052016,42.2687042622238));
#64176=CARTESIAN_POINT('Ctrl Pts',(-2.8762762550339,7.37219346255176,42.2607922559388));
#64177=CARTESIAN_POINT('Ctrl Pts',(-2.69230103212412,7.4387792111625,42.2528802496538));
#64178=CARTESIAN_POINT('Ctrl Pts',(-2.6152173850023,7.46667792637031,42.2495652037968));
#64179=CARTESIAN_POINT('Ctrl Pts',(-2.53774063856249,7.4933636683486,42.2462501579398));
#64180=CARTESIAN_POINT('Ctrl Pts',(-2.45991226034516,7.51882654883085,42.2429351120828));
#64181=CARTESIAN_POINT('Ctrl Pts',(-2.27584207891438,7.5790482460764,42.2350947702136));
#64182=CARTESIAN_POINT('Ctrl Pts',(-2.08928226693087,7.63259703827931,42.2272544283444));
#64183=CARTESIAN_POINT('Ctrl Pts',(-1.90076281645489,7.67925919054582,42.2194140864752));
#64184=CARTESIAN_POINT('Ctrl Pts',(-1.71245413633543,7.7258691731373,42.2115825103416));
#64185=CARTESIAN_POINT('Ctrl Pts',(-1.52219051807484,7.76560776355152,42.203750934208));
#64186=CARTESIAN_POINT('Ctrl Pts',(-1.33052027264029,7.7983098684326,42.1959193580743));
#64187=CARTESIAN_POINT('Ctrl Pts',(-1.13902705125604,7.83098177009122,42.1880950150786));
#64188=CARTESIAN_POINT('Ctrl Pts',(-0.946130133980474,7.85663006967012,
42.180270672083));
#64189=CARTESIAN_POINT('Ctrl Pts',(-0.752391472052713,7.87513987639473,
42.1724463290873));
#64190=CARTESIAN_POINT('Ctrl Pts',(-0.558794093171459,7.89363618492616,
42.1646276919585));
#64191=CARTESIAN_POINT('Ctrl Pts',(-0.364356540635688,7.90500433570941,
42.1568090548297));
#64192=CARTESIAN_POINT('Ctrl Pts',(-0.169649596957392,7.90918074229261,
42.1489904177009));
#64193=CARTESIAN_POINT('Ctrl Pts',(0.0249531835348763,7.91335491460615,
42.141175963341));
#64194=CARTESIAN_POINT('Ctrl Pts',(0.219824717474835,7.91034499936617,42.1333615089811));
#64195=CARTESIAN_POINT('Ctrl Pts',(0.414390284975091,7.90013934634816,42.1255470546213));
#64196=CARTESIAN_POINT('Ctrl Pts',(0.608889554322827,7.88993717090302,42.1177352630341));
#64197=CARTESIAN_POINT('Ctrl Pts',(0.80308271426759,7.87254416148577,42.109923471447));
#64198=CARTESIAN_POINT('Ctrl Pts',(0.996396040113872,7.84800076014557,42.1021116798598));
#64199=CARTESIAN_POINT('Ctrl Pts',(1.18971841333569,7.82345621013458,42.0942995226683));
#64200=CARTESIAN_POINT('Ctrl Pts',(1.38216052021535,7.79176063483256,42.0864873654767));
#64201=CARTESIAN_POINT('Ctrl Pts',(1.57315422730095,7.75300630575812,42.0786752082851));
#64202=CARTESIAN_POINT('Ctrl Pts',(1.76416354829495,7.7142488084822,42.0708624124426));
#64203=CARTESIAN_POINT('Ctrl Pts',(1.95372388860504,7.66843147708458,42.0630496166001));
#64204=CARTESIAN_POINT('Ctrl Pts',(2.14127785751969,7.6156976132785,42.0552368207576));
#64205=CARTESIAN_POINT('Ctrl Pts',(2.32888016087265,7.5629501594551,42.0474220114834));
#64206=CARTESIAN_POINT('Ctrl Pts',(2.5144747241418,7.50328271750232,42.0396072022092));
#64207=CARTESIAN_POINT('Ctrl Pts',(2.69751970754075,7.43688835652582,42.031792392935));
#64208=CARTESIAN_POINT('Ctrl Pts',(2.88064407445718,7.37046520143643,42.0239741945101));
#64209=CARTESIAN_POINT('Ctrl Pts',(3.06121632856204,7.29730943561723,42.0161559960851));
#64210=CARTESIAN_POINT('Ctrl Pts',(3.23871484176716,7.21766216816201,42.0083377976602));
#64211=CARTESIAN_POINT('Ctrl Pts',(3.41641996227953,7.13792219171919,42.0005104988946));
#64212=CARTESIAN_POINT('Ctrl Pts',(3.59104387509404,7.051675766105,41.9926832001291));
#64213=CARTESIAN_POINT('Ctrl Pts',(3.7620888131397,6.95921035477799,41.9848559013636));
#64214=CARTESIAN_POINT('Ctrl Pts',(3.93324541001745,6.86668458165392,41.9770234929055));
#64215=CARTESIAN_POINT('Ctrl Pts',(4.10081807426051,6.76793191029551,41.9691910844475));
#64216=CARTESIAN_POINT('Ctrl Pts',(4.26433820122678,6.66328302757417,41.9613586759894));
#64217=CARTESIAN_POINT('Ctrl Pts',(4.42809300261807,6.55848395895928,41.9535150269215));
#64218=CARTESIAN_POINT('Ctrl Pts',(4.58778336278074,6.44777197775258,41.9456713778536));
#64219=CARTESIAN_POINT('Ctrl Pts',(4.74297299130483,6.3315186332943,41.9378277287857));
#64220=CARTESIAN_POINT('Ctrl Pts',(4.826703138568,6.26879595173432,41.9335958100822));
#64221=CARTESIAN_POINT('Ctrl Pts',(4.90912374903964,6.20446085109633,41.9293638913787));
#64222=CARTESIAN_POINT('Ctrl Pts',(4.99017083595707,6.1385760586608,41.9251319726753));
#64223=CARTESIAN_POINT('Ctrl Pts',(5.14180674225222,6.01530820793337,41.9172142195224));
#64224=CARTESIAN_POINT('Ctrl Pts',(5.28908562653389,5.88624514946329,41.9092964663696));
#64225=CARTESIAN_POINT('Ctrl Pts',(5.43153577643814,5.75172496815282,41.9013787132167));
#64226=CARTESIAN_POINT('Ctrl Pts',(5.57382226136985,5.61735934085155,41.8934700569926));
#64227=CARTESIAN_POINT('Ctrl Pts',(5.71129081437693,5.47754931330097,41.8855614007684));
#64228=CARTESIAN_POINT('Ctrl Pts',(5.84350099013029,5.3326744864417,41.8776527445442));
#64229=CARTESIAN_POINT('Ctrl Pts',(5.97558373985316,5.18793929198214,41.8697517107943));
#64230=CARTESIAN_POINT('Ctrl Pts',(6.10241797775633,5.03814927516368,41.8618506770445));
#64231=CARTESIAN_POINT('Ctrl Pts',(6.22359827888221,4.88372250062332,41.8539496432946));
#64232=CARTESIAN_POINT('Ctrl Pts',(6.3446842090389,4.72941598823981,41.8460547625928));
#64233=CARTESIAN_POINT('Ctrl Pts',(6.4601247631334,4.57048018198781,41.8381598818909));
#64234=CARTESIAN_POINT('Ctrl Pts',(6.56955298426317,4.40736821549538,41.8302650011891));
#64235=CARTESIAN_POINT('Ctrl Pts',(6.67891623099291,4.24435309881052,41.8223748081732));
#64236=CARTESIAN_POINT('Ctrl Pts',(6.78227406681057,4.07716704806391,41.8144846151574));
#64237=CARTESIAN_POINT('Ctrl Pts',(6.87930111374699,3.90629455960497,41.8065944221415));
#64238=CARTESIAN_POINT('Ctrl Pts',(6.97628849652655,3.73549192293891,41.7987074545959));
#64239=CARTESIAN_POINT('Ctrl Pts',(7.06695007841203,3.56100615102911,41.7908204870503));
#64240=CARTESIAN_POINT('Ctrl Pts',(7.15100480639265,3.3833491186913,41.7829335195047));
#64241=CARTESIAN_POINT('Ctrl Pts',(7.2350522347939,3.20570751465408,41.7750472368884));
#64242=CARTESIAN_POINT('Ctrl Pts',(7.31249379934101,3.02489550735143,41.767160954272));
#64243=CARTESIAN_POINT('Ctrl Pts',(7.38309503535332,2.84144834528823,41.7592746716557));
#64244=CARTESIAN_POINT('Ctrl Pts',(7.45369614727388,2.65800150565959,41.7513884029007));
#64245=CARTESIAN_POINT('Ctrl Pts',(7.51745683033518,2.4719198418899,41.7435021341456));
#64246=CARTESIAN_POINT('Ctrl Pts',(7.57419125410534,2.28375739653628,41.7356158653906));
#64247=CARTESIAN_POINT('Ctrl Pts',(7.63093508714138,2.09556374489981,41.7277282887171));
#64248=CARTESIAN_POINT('Ctrl Pts',(7.68065023952765,1.90528895396002,41.7198407120436));
#64249=CARTESIAN_POINT('Ctrl Pts',(7.72320105331794,1.71350123724164,41.7119531353701));
#64250=CARTESIAN_POINT('Ctrl Pts',(7.76576605582388,1.52164956824752,41.7040629285569));
#64251=CARTESIAN_POINT('Ctrl Pts',(7.80116188516549,1.32828430444575,41.6961727217438));
#64252=CARTESIAN_POINT('Ctrl Pts',(7.82930414348475,1.13398308136079,41.6882825149306));
#64253=CARTESIAN_POINT('Ctrl Pts',(7.85747357769407,0.939494229102066,41.68038468885));
#64254=CARTESIAN_POINT('Ctrl Pts',(7.87837540062114,0.744067953381702,41.6724868627694));
#64255=CARTESIAN_POINT('Ctrl Pts',(7.8919770681622,0.548287292942333,41.6645890366888));
#64256=CARTESIAN_POINT('Ctrl Pts',(7.90558626720361,0.352398225051473,41.6566868374326));
#64257=CARTESIAN_POINT('Ctrl Pts',(7.91188724033619,0.15615472481144,41.6487846381765));
#64258=CARTESIAN_POINT('Ctrl Pts',(7.91089957771789,-0.0398606480500094,
41.6408824389203));
#64259=CARTESIAN_POINT('Ctrl Pts',(7.90991072291592,-0.236112626328689,
41.6329707011105));
#64260=CARTESIAN_POINT('Ctrl Pts',(7.90161567342775,-0.432135583878224,
41.6250589633007));
#64261=CARTESIAN_POINT('Ctrl Pts',(7.88608592012398,-0.627351464828427,
41.6171472254909));
#64262=CARTESIAN_POINT('Ctrl Pts',(7.87966182751903,-0.708105155672722,
41.6138744280831));
#64263=CARTESIAN_POINT('Ctrl Pts',(7.87200035814089,-0.78872084903206,41.6106016306753));
#64264=CARTESIAN_POINT('Ctrl Pts',(7.86310912297639,-0.869158167519254,
41.6073288332675));
#64265=CARTESIAN_POINT('Ctrl Pts',(7.84052008578004,-1.07351690347274,41.5990139770059));
#64266=CARTESIAN_POINT('Ctrl Pts',(7.80994062011707,-1.27716956920081,41.5906991207443));
#64267=CARTESIAN_POINT('Ctrl Pts',(7.77142554366926,-1.47948167248024,41.5823842644827));
#64268=CARTESIAN_POINT('Ctrl Pts',(7.73295789719928,-1.68154463543707,41.5740796476776));
#64269=CARTESIAN_POINT('Ctrl Pts',(7.68657418514291,-1.88227004180361,41.5657750308724));
#64270=CARTESIAN_POINT('Ctrl Pts',(7.63238085311091,-2.0810294358961,41.5574704140673));
#64271=CARTESIAN_POINT('Ctrl Pts',(7.57825068363204,-2.27955717509084,41.5491754763274));
#64272=CARTESIAN_POINT('Ctrl Pts',(7.51632912558697,-2.47612319039856,41.5408805385876));
#64273=CARTESIAN_POINT('Ctrl Pts',(7.44677361945884,-2.670109297488,41.5325856008478));
#64274=CARTESIAN_POINT('Ctrl Pts',(7.3773223641015,-2.86380465547201,41.5243030956773));
#64275=CARTESIAN_POINT('Ctrl Pts',(7.30026009332459,-3.05492754681884,41.5160205905068));
#64276=CARTESIAN_POINT('Ctrl Pts',(7.21579400125396,-3.24287494847817,41.5077380853363));
#64277=CARTESIAN_POINT('Ctrl Pts',(7.13140550331944,-3.43064969367965,41.4994631888265));
#64278=CARTESIAN_POINT('Ctrl Pts',(7.03962686708011,-3.61525449989592,41.4911882923166));
#64279=CARTESIAN_POINT('Ctrl Pts',(6.94071398715704,-3.79610462823177,41.4829133958068));
#64280=CARTESIAN_POINT('Ctrl Pts',(6.84191425059518,-3.97674788774112,41.4746479646933));
#64281=CARTESIAN_POINT('Ctrl Pts',(6.73599669479649,-4.15364478284566,41.4663825335797));
#64282=CARTESIAN_POINT('Ctrl Pts',(6.62326402536842,-4.32623330973498,41.4581171024662));
#64283=CARTESIAN_POINT('Ctrl Pts',(6.57921061017469,-4.39367706025826,41.4548871561654));
#64284=CARTESIAN_POINT('Ctrl Pts',(6.53411698324595,-4.46046313740019,41.4516572098646));
#64285=CARTESIAN_POINT('Ctrl Pts',(6.48800312905023,-4.52655900187266,41.4484272635638));
#64286=CARTESIAN_POINT('Ctrl Pts',(6.36998153523263,-4.69572159749272,41.4401606934187));
#64287=CARTESIAN_POINT('Ctrl Pts',(6.24540708208217,-4.86017049045324,41.4318941232737));
#64288=CARTESIAN_POINT('Ctrl Pts',(6.11468798505374,-5.01941349616062,41.4236275531286));
#64289=CARTESIAN_POINT('Ctrl Pts',(5.98385176220058,-5.17879918544523,41.415353576041));
#64290=CARTESIAN_POINT('Ctrl Pts',(5.84686009039699,-5.3329694483423,41.4070795989534));
#64291=CARTESIAN_POINT('Ctrl Pts',(5.70415960291809,-5.48146734227591,41.3988056218657));
#64292=CARTESIAN_POINT('Ctrl Pts',(5.56132199162359,-5.6301079308715,41.3905236941444));
#64293=CARTESIAN_POINT('Ctrl Pts',(5.41276481606496,-5.77306505704043,41.382241766423));
#64294=CARTESIAN_POINT('Ctrl Pts',(5.25897007300826,-5.90992003086366,41.3739598387017));
#64295=CARTESIAN_POINT('Ctrl Pts',(5.1049203970669,-6.04700185791062,41.3656641827106));
#64296=CARTESIAN_POINT('Ctrl Pts',(4.94561601610714,-6.17796111457056,41.3573685267194));
#64297=CARTESIAN_POINT('Ctrl Pts',(4.78157198150445,-6.30241940731427,41.3490728707283));
#64298=CARTESIAN_POINT('Ctrl Pts',(4.6173796828416,-6.42699018626846,41.3407697170696));
#64299=CARTESIAN_POINT('Ctrl Pts',(4.44843941738418,-6.54504810111771,41.3324665634109));
#64300=CARTESIAN_POINT('Ctrl Pts',(4.27529456373084,-6.65625851310881,41.3241634097521));
#64301=CARTESIAN_POINT('Ctrl Pts',(4.10188572706688,-6.76763848058337,41.3158475968));
#64302=CARTESIAN_POINT('Ctrl Pts',(3.92425973916612,-6.87214992416895,41.3075317838479));
#64303=CARTESIAN_POINT('Ctrl Pts',(3.74298551908125,-6.96950359810138,41.2992159708959));
#64304=CARTESIAN_POINT('Ctrl Pts',(3.67257358532567,-7.00731846464215,41.2959858785505));
#64305=CARTESIAN_POINT('Ctrl Pts',(3.60161144474516,-7.0440539050805,41.2927557862051));
#64306=CARTESIAN_POINT('Ctrl Pts',(3.53013323911411,-7.07969493086402,41.2895256938598));
#64307=CARTESIAN_POINT('Ctrl Pts',(3.35507271984093,-7.16698498558781,41.2816147280166));
#64308=CARTESIAN_POINT('Ctrl Pts',(3.17655169375813,-7.24788823486347,41.2737037621734));
#64309=CARTESIAN_POINT('Ctrl Pts',(2.99507658703413,-7.32211972299006,41.2657927963303));
#64310=CARTESIAN_POINT('Ctrl Pts',(2.81378511634647,-7.39627609571102,41.2578898356534));
#64311=CARTESIAN_POINT('Ctrl Pts',(2.6295458357032,-7.46377402594048,41.2499868749765));
#64312=CARTESIAN_POINT('Ctrl Pts',(2.44288948778114,-7.52437452221036,41.2420839142997));
#64313=CARTESIAN_POINT('Ctrl Pts',(2.25638747591343,-7.58492491120241,41.2341874881542));
#64314=CARTESIAN_POINT('Ctrl Pts',(2.06747270404295,-7.63858912207468,41.2262910620088));
#64315=CARTESIAN_POINT('Ctrl Pts',(1.87669587182935,-7.68517622469769,41.2183946358633));
#64316=CARTESIAN_POINT('Ctrl Pts',(1.68604148681759,-7.73173342609899,41.2105032779186));
#64317=CARTESIAN_POINT('Ctrl Pts',(1.49352775615284,-7.77122248811454,41.2026119199739));
#64318=CARTESIAN_POINT('Ctrl Pts',(1.29972079733459,-7.803502216888,41.1947205620293));
#64319=CARTESIAN_POINT('Ctrl Pts',(1.10600238117861,-7.83576719834207,41.186832809331));
#64320=CARTESIAN_POINT('Ctrl Pts',(0.910992253337599,-7.86082935345353,
41.1789450566327));
#64321=CARTESIAN_POINT('Ctrl Pts',(0.715267271467289,-7.87859846231344,
41.1710573039344));
#64322=CARTESIAN_POINT('Ctrl Pts',(0.519595509620023,-7.89636273953472,
41.1631716960128));
#64323=CARTESIAN_POINT('Ctrl Pts',(0.323209623895253,-7.90683789200927,
41.1552860880912));
#64324=CARTESIAN_POINT('Ctrl Pts',(0.126692438162148,-7.90998546307846,
41.1474004801696));
#64325=CARTESIAN_POINT('Ctrl Pts',(-0.0698479250685975,-7.91313340537636,
41.139513942209));
#64326=CARTESIAN_POINT('Ctrl Pts',(-0.266519274877356,-7.90895202712437,
41.1316274042483));
#64327=CARTESIAN_POINT('Ctrl Pts',(-0.462737289344198,-7.89745498252762,
41.1237408662877));
#64328=CARTESIAN_POINT('Ctrl Pts',(-0.65898002357199,-7.88595648952058,
41.1158533347723));
#64329=CARTESIAN_POINT('Ctrl Pts',(-0.854768964509576,-7.86714051314872,
41.107965803257));
#64330=CARTESIAN_POINT('Ctrl Pts',(-1.0495234431412,-7.8410727290529,41.1000782717416));
#64331=CARTESIAN_POINT('Ctrl Pts',(-1.24433510025892,-7.81499729164691,
41.0921884245049));
#64332=CARTESIAN_POINT('Ctrl Pts',(-1.43811134833977,-7.78166584941576,
41.0842985772681));
#64333=CARTESIAN_POINT('Ctrl Pts',(-1.63028001038072,-7.74119552057388,
41.0764087300314));
#64334=CARTESIAN_POINT('Ctrl Pts',(-1.82253730213947,-7.70070652649393,
41.0685152439342));
#64335=CARTESIAN_POINT('Ctrl Pts',(-2.0131851935778,-7.65307215560085,41.0606217578371));
#64336=CARTESIAN_POINT('Ctrl Pts',(-2.20166476039912,-7.598459928355,41.0527282717399));
#64337=CARTESIAN_POINT('Ctrl Pts',(-2.39036220933888,-7.54378456945003,
41.0448256607838));
#64338=CARTESIAN_POINT('Ctrl Pts',(-2.57688599598329,-7.48211533802818,
41.0369230498276));
#64339=CARTESIAN_POINT('Ctrl Pts',(-2.76069423665923,-7.41366901956626,
41.0290204388715));
#64340=CARTESIAN_POINT('Ctrl Pts',(-2.94462438897629,-7.34517730377622,
41.0211125864731));
#64341=CARTESIAN_POINT('Ctrl Pts',(-3.12583508758474,-7.26989967170283,
41.0132047340748));
#64342=CARTESIAN_POINT('Ctrl Pts',(-3.30380706649977,-7.18809987878203,
41.0052968816764));
#64343=CARTESIAN_POINT('Ctrl Pts',(-3.48202256156049,-7.10618816054347,
40.997378209093));
#64344=CARTESIAN_POINT('Ctrl Pts',(-3.65699017924273,-7.01773661133071,
40.9894595365097));
#64345=CARTESIAN_POINT('Ctrl Pts',(-3.82821673433037,-6.92305406847245,
40.9815408639263));
#64346=CARTESIAN_POINT('Ctrl Pts',(-3.89898428997597,-6.88392198339978,
40.9782680941016));
#64347=CARTESIAN_POINT('Ctrl Pts',(-3.96911317311707,-6.84372605308623,
40.9749953242769));
#64348=CARTESIAN_POINT('Ctrl Pts',(-4.03857014346165,-6.80249014672863,
40.9717225544521));
#64349=CARTESIAN_POINT('Ctrl Pts',(-4.20502250025122,-6.70366905269699,
40.9638794215333));
#64350=CARTESIAN_POINT('Ctrl Pts',(-4.36810660132914,-6.59857981631457,
40.9560362886144));
#64351=CARTESIAN_POINT('Ctrl Pts',(-4.52731165393276,-6.4874779528076,40.9481931556955));
#64352=CARTESIAN_POINT('Ctrl Pts',(-4.68632973714723,-6.37650656661408,
40.9403592337015));
#64353=CARTESIAN_POINT('Ctrl Pts',(-4.8414775577109,-6.25953681227435,40.9325253117074));
#64354=CARTESIAN_POINT('Ctrl Pts',(-4.99226859464812,-6.13687015333469,
40.9246913897133));
#64355=CARTESIAN_POINT('Ctrl Pts',(-5.14291186982358,-6.01432369677576,
40.9168651442639));
#64356=CARTESIAN_POINT('Ctrl Pts',(-5.28920659270855,-5.88609167275004,
40.9090388988143));
#64357=CARTESIAN_POINT('Ctrl Pts',(-5.4306947850553,-5.75251902661548,40.9012126533649));
#64358=CARTESIAN_POINT('Ctrl Pts',(-5.57207183242556,-5.61905130746013,
40.8933925557631));
#64359=CARTESIAN_POINT('Ctrl Pts',(-5.70864961500615,-5.48025156199503,
40.8855724581614));
#64360=CARTESIAN_POINT('Ctrl Pts',(-5.84000271093576,-5.33650534865871,
40.8777523605597));
#64361=CARTESIAN_POINT('Ctrl Pts',(-5.97127814402506,-5.19284412562377,
40.8699368866099));
#64362=CARTESIAN_POINT('Ctrl Pts',(-6.0973348074805,-5.0442425192713,40.86212141266));
#64363=CARTESIAN_POINT('Ctrl Pts',(-6.21778355414878,-4.8911234572189,40.8543059387102));
#64364=CARTESIAN_POINT('Ctrl Pts',(-6.33818448079993,-4.73806518580462,
40.8464935676245));
#64365=CARTESIAN_POINT('Ctrl Pts',(-6.45298170951549,-4.58049330795824,
40.8386811965388));
#64366=CARTESIAN_POINT('Ctrl Pts',(-6.56182575565952,-4.41886453202216,
40.8308688254532));
#64367=CARTESIAN_POINT('Ctrl Pts',(-6.67066568166833,-4.25724187431152,
40.8230567500936));
#64368=CARTESIAN_POINT('Ctrl Pts',(-6.77355267021599,-4.09156291097583,
40.815244674734));
#64369=CARTESIAN_POINT('Ctrl Pts',(-6.87017977626858,-3.92231447512183,
40.8074325993744));
#64370=CARTESIAN_POINT('Ctrl Pts',(-6.96680970836285,-3.7530610892786,40.799620295536));
#64371=CARTESIAN_POINT('Ctrl Pts',(-7.0571792181417,-3.58023832811498,40.7918079916975));
#64372=CARTESIAN_POINT('Ctrl Pts',(-7.14102668421596,-3.40435880825092,
40.7839956878591));
#64373=CARTESIAN_POINT('Ctrl Pts',(-7.22489135579719,-3.22844319789484,
40.7761817809353));
#64374=CARTESIAN_POINT('Ctrl Pts',(-7.30223116625825,-3.04946989684581,
40.7683678740114));
#64375=CARTESIAN_POINT('Ctrl Pts',(-7.37283206215466,-2.86797287003629,
40.7605539670876));
#64376=CARTESIAN_POINT('Ctrl Pts',(-7.44345986869196,-2.68640666278299,
40.7527370817704));
#64377=CARTESIAN_POINT('Ctrl Pts',(-7.50734351665096,-2.50231514113536,
40.7449201964531));
#64378=CARTESIAN_POINT('Ctrl Pts',(-7.56431831949938,-2.31624898516677,
40.7371033111359));
#64379=CARTESIAN_POINT('Ctrl Pts',(-7.62135492795542,-2.12998098678269,
40.7292779461518));
#64380=CARTESIAN_POINT('Ctrl Pts',(-7.67146761948069,-1.94173441219844,
40.7214525811677));
#64381=CARTESIAN_POINT('Ctrl Pts',(-7.71454224380687,-1.75207276347737,
40.7136272161836));
#64382=CARTESIAN_POINT('Ctrl Pts',(-7.75764304698127,-1.56229584680925,
40.7057970952894));
#64383=CARTESIAN_POINT('Ctrl Pts',(-7.7936971934392,-1.37110248660038,40.6979669743952));
#64384=CARTESIAN_POINT('Ctrl Pts',(-7.82264222598379,-1.17906301962849,
40.690136853501));
#64385=CARTESIAN_POINT('Ctrl Pts',(-7.85162682446981,-0.986761047430777,
40.6822960293504));
#64386=CARTESIAN_POINT('Ctrl Pts',(-7.87348286043591,-0.793611006666677,
40.6744552051998));
#64387=CARTESIAN_POINT('Ctrl Pts',(-7.88819989848087,-0.600186105809256,
40.6666143810492));
#64388=CARTESIAN_POINT('Ctrl Pts',(-7.8961426136037,-0.49579561089576,40.6623827257143));
#64389=CARTESIAN_POINT('Ctrl Pts',(-7.90200684590501,-0.391325034556162,
40.6581510703794));
#64390=CARTESIAN_POINT('Ctrl Pts',(-7.90579724297386,-0.286863997369564,
40.6539194150445));
#64391=CARTESIAN_POINT('Ctrl Pts',(-7.90925710005275,-0.191512441210014,
40.650056779442));
#64392=CARTESIAN_POINT('Ctrl Pts',(-7.91099181751041,-0.0961026461293392,
40.6461941438395));
#64393=CARTESIAN_POINT('Ctrl Pts',(-7.91099997112236,-0.000675945236853683,
40.642331508237));
#64394=CARTESIAN_POINT('',(-7.90652959962495,-0.00529323366394208,38.6423315082371));
#64395=CARTESIAN_POINT('Ctrl Pts',(-7.92426962316665,-0.000638036300153408,
40.6423299305302));
#64396=CARTESIAN_POINT('Ctrl Pts',(-7.91681046214448,2.5252695445412,40.5402587122325));
#64397=CARTESIAN_POINT('Ctrl Pts',(-5.23832781156842,7.68132265384459,40.332253114132));
#64398=CARTESIAN_POINT('Ctrl Pts',(3.54974568342456,8.65605708304547,40.0183131362292));
#64399=CARTESIAN_POINT('Ctrl Pts',(9.20185311915298,1.69349879413918,39.7005099968215));
#64400=CARTESIAN_POINT('Ctrl Pts',(6.86833150499802,-5.3826179369575,39.435674047315));
#64401=CARTESIAN_POINT('Ctrl Pts',(2.08192809636596,-7.95547529202212,39.2238052877101));
#64402=CARTESIAN_POINT('Ctrl Pts',(-3.35120507934021,-8.05704524214747,
39.0119365281047));
#64403=CARTESIAN_POINT('Ctrl Pts',(-7.37691166608612,-4.37872292798657,
38.8181119349473));
#64404=CARTESIAN_POINT('Ctrl Pts',(-7.91046959319798,-0.878292219197368,
38.6772545316909));
#64405=CARTESIAN_POINT('Ctrl Pts',(-7.90405025860222,-0.00822892851515322,
38.6423315082371));
#64406=CARTESIAN_POINT('',(-7.91214355523022,0.00146147383487005,36.6443103639743));
#64407=CARTESIAN_POINT('Ctrl Pts',(-7.911,-8.17679257636428E-13,38.6423315082371));
#64408=CARTESIAN_POINT('Ctrl Pts',(-7.91100000000023,2.2016758966659,38.5537440725043));
#64409=CARTESIAN_POINT('Ctrl Pts',(-6.94214576672421,4.38610418338602,38.4651566367716));
#64410=CARTESIAN_POINT('Ctrl Pts',(-3.67820201488378,7.34180684107585,38.2879817653062));
#64411=CARTESIAN_POINT('Ctrl Pts',(-1.40868175871851,8.08992666571317,38.1993943295734));
#64412=CARTESIAN_POINT('Ctrl Pts',(2.97309270521164,7.65454228025298,38.022219458108));
#64413=CARTESIAN_POINT('Ctrl Pts',(5.05102072675505,6.474448808343,37.9336320223753));
#64414=CARTESIAN_POINT('Ctrl Pts',(7.66951518847823,2.9342519536783,37.7564571509098));
#64415=CARTESIAN_POINT('Ctrl Pts',(8.1895687224706,0.60188196010054,37.6678697151771));
#64416=CARTESIAN_POINT('Ctrl Pts',(7.32306689761408,-3.71537198232318,37.4906948437117));
#64417=CARTESIAN_POINT('Ctrl Pts',(5.94329958850306,-5.666435189364,37.4021074079789));
#64418=CARTESIAN_POINT('Ctrl Pts',(2.16154501638003,-7.92205913232954,37.2249325365135));
#64419=CARTESIAN_POINT('Ctrl Pts',(-0.210816529298698,-8.20894963713006,
37.1363451007808));
#64420=CARTESIAN_POINT('Ctrl Pts',(-4.42123908576288,-6.91982244717925,
36.9591702293153));
#64421=CARTESIAN_POINT('Ctrl Pts',(-6.22631625634069,-5.35390358803658,
36.8705827935826));
#64422=CARTESIAN_POINT('Ctrl Pts',(-7.65317280859451,-2.31334857514661,
36.7354407413123));
#64423=CARTESIAN_POINT('Ctrl Pts',(-7.91099999999989,-1.1570283783663,36.6888861247747));
#64424=CARTESIAN_POINT('Ctrl Pts',(-7.911,-7.63833440942108E-13,36.6423315082371));
#64425=CARTESIAN_POINT('',(-7.91099997583771,0.000602220688781498,34.642307277048));
#64426=CARTESIAN_POINT('Ctrl Pts',(-7.91099771853781,0.00600810199810929,
36.6423315082371));
#64427=CARTESIAN_POINT('Ctrl Pts',(-7.91082701748352,0.230773868533368,
36.6333181043834));
#64428=CARTESIAN_POINT('Ctrl Pts',(-7.90107349095901,0.455147217331988,
36.6243047005298));
#64429=CARTESIAN_POINT('Ctrl Pts',(-7.88186061629211,0.678376168024303,
36.6152912966761));
#64430=CARTESIAN_POINT('Ctrl Pts',(-7.86249103411946,0.903425858854828,
36.606204376076));
#64431=CARTESIAN_POINT('Ctrl Pts',(-7.83350723763257,1.12731227582692,36.5971174554758));
#64432=CARTESIAN_POINT('Ctrl Pts',(-7.79508525974753,1.34928380753155,36.5880305348757));
#64433=CARTESIAN_POINT('Ctrl Pts',(-7.75650928789974,1.57214499348267,36.5789071942111));
#64434=CARTESIAN_POINT('Ctrl Pts',(-7.70841942193409,1.79307580146918,36.5697838535464));
#64435=CARTESIAN_POINT('Ctrl Pts',(-7.65104221992903,2.01133635895725,36.5606605128818));
#64436=CARTESIAN_POINT('Ctrl Pts',(-7.59339181638938,2.23063616404131,36.5514937314327));
#64437=CARTESIAN_POINT('Ctrl Pts',(-7.52636550019852,2.44724011743129,36.5423269499835));
#64438=CARTESIAN_POINT('Ctrl Pts',(-7.45024055696212,2.66042038847185,36.5331601685343));
#64439=CARTESIAN_POINT('Ctrl Pts',(-7.42067243304598,2.74322295491882,36.5295996466045));
#64440=CARTESIAN_POINT('Ctrl Pts',(-7.38973212761027,2.82550925150776,36.5260391246746));
#64441=CARTESIAN_POINT('Ctrl Pts',(-7.35743777047115,2.90723759841616,36.5224786027448));
#64442=CARTESIAN_POINT('Ctrl Pts',(-7.28629962259197,3.08726915015888,36.5146354698259));
#64443=CARTESIAN_POINT('Ctrl Pts',(-7.20843803850659,3.26497043139147,36.506792336907));
#64444=CARTESIAN_POINT('Ctrl Pts',(-7.12402418831121,3.439796558571,36.4989492039881));
#64445=CARTESIAN_POINT('Ctrl Pts',(-7.03970947319829,3.61441737107176,36.491115281994));
#64446=CARTESIAN_POINT('Ctrl Pts',(-6.94885796507703,3.78616943984571,36.48328136));
#64447=CARTESIAN_POINT('Ctrl Pts',(-6.85169005333668,3.95452454955171,36.4754474380059));
#64448=CARTESIAN_POINT('Ctrl Pts',(-6.75461735747975,4.12271468627217,36.4676211925564));
#64449=CARTESIAN_POINT('Ctrl Pts',(-6.65124075828519,4.28751419072813,36.4597949471069));
#64450=CARTESIAN_POINT('Ctrl Pts',(-6.54182810735693,4.44841612417216,36.4519687016574));
#64451=CARTESIAN_POINT('Ctrl Pts',(-6.43250140470697,4.60919166232245,36.4441486040556));
#64452=CARTESIAN_POINT('Ctrl Pts',(-6.31714829073141,4.76607543819526,36.4363285064539));
#64453=CARTESIAN_POINT('Ctrl Pts',(-6.19608188419913,4.91858620787512,36.4285084088522));
#64454=CARTESIAN_POINT('Ctrl Pts',(-6.07508705847705,5.07100680518784,36.4206929349023));
#64455=CARTESIAN_POINT('Ctrl Pts',(-5.94838588706709,5.21905927215613,36.4128774609525));
#64456=CARTESIAN_POINT('Ctrl Pts',(-5.81633414354872,5.362292245914,36.4050619870027));
#64457=CARTESIAN_POINT('Ctrl Pts',(-5.6843348266164,5.50546835396435,36.397249615917));
#64458=CARTESIAN_POINT('Ctrl Pts',(-5.54698940788077,5.6438285229488,36.3894372448313));
#64459=CARTESIAN_POINT('Ctrl Pts',(-5.40469331071708,5.77695518565706,36.3816248737456));
#64460=CARTESIAN_POINT('Ctrl Pts',(-5.26240259996817,5.91007680904635,36.373812798386));
#64461=CARTESIAN_POINT('Ctrl Pts',(-5.11516183465845,6.03796507408886,36.3660007230264));
#64462=CARTESIAN_POINT('Ctrl Pts',(-4.96340293520149,6.1602396303093,36.3581886476668));
#64463=CARTESIAN_POINT('Ctrl Pts',(-4.81163959726983,6.28251776267932,36.3503763438283));
#64464=CARTESIAN_POINT('Ctrl Pts',(-4.65535813544312,6.39918163782201,36.3425640399899));
#64465=CARTESIAN_POINT('Ctrl Pts',(-4.49502312304542,6.50989156002518,36.3347517361514));
#64466=CARTESIAN_POINT('Ctrl Pts',(-4.33465520989007,6.62062419991343,36.3269378292276));
#64467=CARTESIAN_POINT('Ctrl Pts',(-4.17023237864531,6.7254002531701,36.3191239223037));
#64468=CARTESIAN_POINT('Ctrl Pts',(-4.00224783295993,6.82392359889584,36.3113100153799));
#64469=CARTESIAN_POINT('Ctrl Pts',(-3.83419925732518,6.92248449834304,36.3034931300627));
#64470=CARTESIAN_POINT('Ctrl Pts',(-3.66258656612503,7.0147877650145,36.2956762447454));
#64471=CARTESIAN_POINT('Ctrl Pts',(-3.48792730457781,7.10058336462439,36.2878593594282));
#64472=CARTESIAN_POINT('Ctrl Pts',(-3.31307857468228,7.18647203430915,36.2800339944441));
#64473=CARTESIAN_POINT('Ctrl Pts',(-3.13517698946395,7.26583878220487,36.27220862946));
#64474=CARTESIAN_POINT('Ctrl Pts',(-2.95476077761802,7.33848143331099,36.2643832644759));
#64475=CARTESIAN_POINT('Ctrl Pts',(-2.77423491679197,7.41116823340198,36.2565531435816));
#64476=CARTESIAN_POINT('Ctrl Pts',(-2.59119171346333,7.47712267358661,36.2487230226874));
#64477=CARTESIAN_POINT('Ctrl Pts',(-2.40618435216095,7.53619253094132,36.2408929017932));
#64478=CARTESIAN_POINT('Ctrl Pts',(-2.22092409805519,7.59534313287678,36.2330520776425));
#64479=CARTESIAN_POINT('Ctrl Pts',(-2.03369466101054,7.647590261596,36.2252112534919));
#64480=CARTESIAN_POINT('Ctrl Pts',(-1.84506032084028,7.69283260005447,36.2173704293413));
#64481=CARTESIAN_POINT('Ctrl Pts',(-1.74325526864717,7.71724967397614,36.2131387740066));
#64482=CARTESIAN_POINT('Ctrl Pts',(-1.64104112949169,7.73962734805209,36.2089071186719));
#64483=CARTESIAN_POINT('Ctrl Pts',(-1.53850712496967,7.75995598095876,36.2046754633371));
#64484=CARTESIAN_POINT('Ctrl Pts',(-1.34681750920186,7.79796081505384,36.1967642890008));
#64485=CARTESIAN_POINT('Ctrl Pts',(-1.15346117883056,7.82890972097021,36.1888531146645));
#64486=CARTESIAN_POINT('Ctrl Pts',(-0.959000070226024,7.85265814010176,
36.1809419403282));
#64487=CARTESIAN_POINT('Ctrl Pts',(-0.764749782710718,7.87638081286365,
36.173039342732));
#64488=CARTESIAN_POINT('Ctrl Pts',(-0.569397441845241,7.8929185063317,36.1651367451358));
#64489=CARTESIAN_POINT('Ctrl Pts',(-0.373516690169528,7.90217731275152,
36.1572341475396));
#64490=CARTESIAN_POINT('Ctrl Pts',(-0.177811937714245,7.91142780011651,
36.1493386504421));
#64491=CARTESIAN_POINT('Ctrl Pts',(0.0184199374734158,7.91341241269837,
36.1414431533446));
#64492=CARTESIAN_POINT('Ctrl Pts',(0.214598342881783,7.90808880521915,36.1335476562471));
#64493=CARTESIAN_POINT('Ctrl Pts',(0.410636886512517,7.90276899310774,36.1256577880986));
#64494=CARTESIAN_POINT('Ctrl Pts',(0.606621693015979,7.89015135087714,36.1177679199502));
#64495=CARTESIAN_POINT('Ctrl Pts',(0.801970041781192,7.87024555221027,36.1098780518018));
#64496=CARTESIAN_POINT('Ctrl Pts',(0.997215363279053,7.85035025191748,36.101992344792));
#64497=CARTESIAN_POINT('Ctrl Pts',(1.19182455367119,7.82317448934777,36.0941066377822));
#64498=CARTESIAN_POINT('Ctrl Pts',(1.38521760805087,7.78877995441814,36.0862209307724));
#64499=CARTESIAN_POINT('Ctrl Pts',(1.57854454051247,7.75439717912811,36.0783379199197));
#64500=CARTESIAN_POINT('Ctrl Pts',(1.77065582657825,7.7128006108626,36.0704549090671));
#64501=CARTESIAN_POINT('Ctrl Pts',(1.96097899889779,7.66410349394382,36.0625718982145));
#64502=CARTESIAN_POINT('Ctrl Pts',(2.15130501150619,7.61540565029336,36.0546887697197));
#64503=CARTESIAN_POINT('Ctrl Pts',(2.33984252091461,7.55960712353441,36.0468056412249));
#64504=CARTESIAN_POINT('Ctrl Pts',(2.52603106682682,7.49687188428786,36.0389225127301));
#64505=CARTESIAN_POINT('Ctrl Pts',(2.71223112496288,7.43413276605877,36.0310388968136));
#64506=CARTESIAN_POINT('Ctrl Pts',(2.89608160303152,7.36445619030373,36.0231552808971));
#64507=CARTESIAN_POINT('Ctrl Pts',(3.07703894152665,7.28805545755029,36.0152716649806));
#64508=CARTESIAN_POINT('Ctrl Pts',(3.25803788676078,7.21163715830646,36.0073862364184));
#64509=CARTESIAN_POINT('Ctrl Pts',(3.43614204910383,7.12849175547434,35.9995008078561));
#64510=CARTESIAN_POINT('Ctrl Pts',(3.61082930293514,7.03888007747432,35.9916153792939));
#64511=CARTESIAN_POINT('Ctrl Pts',(3.78558608622667,6.9492327320088,35.9837268121535));
#64512=CARTESIAN_POINT('Ctrl Pts',(3.95692294440953,6.85311414030414,35.9758382450131));
#64513=CARTESIAN_POINT('Ctrl Pts',(4.12434352441048,6.75083042985479,35.9679496778728));
#64514=CARTESIAN_POINT('Ctrl Pts',(4.29194227630253,6.64843786730302,35.9600527155822));
#64515=CARTESIAN_POINT('Ctrl Pts',(4.45561613086508,6.53986726085201,35.9521557532915));
#64516=CARTESIAN_POINT('Ctrl Pts',(4.61489792240152,6.42546793360718,35.9442587910009));
#64517=CARTESIAN_POINT('Ctrl Pts',(4.77427685464063,6.31099883799192,35.9363570126139));
#64518=CARTESIAN_POINT('Ctrl Pts',(4.92925811202304,6.19069414562624,35.9284552342268));
#64519=CARTESIAN_POINT('Ctrl Pts',(5.07940846381662,6.06494275799105,35.9205534558398));
#64520=CARTESIAN_POINT('Ctrl Pts',(5.22975301186175,5.93902873038989,35.9126414577248));
#64521=CARTESIAN_POINT('Ctrl Pts',(5.37525391931462,5.80765416731018,35.9047294596099));
#64522=CARTESIAN_POINT('Ctrl Pts',(5.51551478509475,5.67124480651305,35.8968174614949));
#64523=CARTESIAN_POINT('Ctrl Pts',(5.57428264562653,5.61409068696611,35.8935024156397));
#64524=CARTESIAN_POINT('Ctrl Pts',(5.63213108832611,5.55605309984752,35.8901873697846));
#64525=CARTESIAN_POINT('Ctrl Pts',(5.68903310393153,5.49716502775487,35.8868723239294));
#64526=CARTESIAN_POINT('Ctrl Pts',(5.82482649262485,5.35663202944195,35.8789611575927));
#64527=CARTESIAN_POINT('Ctrl Pts',(5.95559203093924,5.21087552504861,35.871049991256));
#64528=CARTESIAN_POINT('Ctrl Pts',(6.08090378471279,5.06028953332373,35.8631388249193));
#64529=CARTESIAN_POINT('Ctrl Pts',(6.20607970451243,4.90986677204655,35.8552362340364));
#64530=CARTESIAN_POINT('Ctrl Pts',(6.32581339647896,4.75462521346952,35.8473336431536));
#64531=CARTESIAN_POINT('Ctrl Pts',(6.43971515906603,4.59499615561266,35.8394310522707));
#64532=CARTESIAN_POINT('Ctrl Pts',(6.55351459909433,4.43551049899284,35.8315355606048));
#64533=CARTESIAN_POINT('Ctrl Pts',(6.66149234738,4.27164547377879,35.8236400689388));
#64534=CARTESIAN_POINT('Ctrl Pts',(6.76329827788125,4.10386615332524,35.8157445772729));
#64535=CARTESIAN_POINT('Ctrl Pts',(6.86503164415108,3.93620642096816,35.807854713278));
#64536=CARTESIAN_POINT('Ctrl Pts',(6.96060177897564,3.76463824559535,35.7999648492831));
#64537=CARTESIAN_POINT('Ctrl Pts',(7.04970112771916,3.5896566701894,35.7920749852881));
#64538=CARTESIAN_POINT('Ctrl Pts',(7.13875349959255,3.41476735232358,35.7841892811566));
#64539=CARTESIAN_POINT('Ctrl Pts',(7.22134172750293,3.2364685270999,35.776303577025));
#64540=CARTESIAN_POINT('Ctrl Pts',(7.29720345001519,3.05528113421439,35.7684178728935));
#64541=CARTESIAN_POINT('Ctrl Pts',(7.37303924731667,2.87415566084767,35.7605348636459));
#64542=CARTESIAN_POINT('Ctrl Pts',(7.44215298767534,2.69014390493507,35.7526518543984));
#64543=CARTESIAN_POINT('Ctrl Pts',(7.50432972686331,2.50378839970865,35.7447688451508));
#64544=CARTESIAN_POINT('Ctrl Pts',(7.56650740895673,2.31743006841541,35.736885716358));
#64545=CARTESIAN_POINT('Ctrl Pts',(7.62174776253362,2.12872824118862,35.7290025875652));
#64546=CARTESIAN_POINT('Ctrl Pts',(7.66988498578327,1.9382428394957,35.7211194587724));
#64547=CARTESIAN_POINT('Ctrl Pts',(7.71802519265272,1.74774563122195,35.7132358413711));
#64548=CARTESIAN_POINT('Ctrl Pts',(7.75906130680061,1.55546496257375,35.7053522239697));
#64549=CARTESIAN_POINT('Ctrl Pts',(7.79287814629815,1.36197327321381,35.6974686065684));
#64550=CARTESIAN_POINT('Ctrl Pts',(7.82670276624695,1.16843706601361,35.689583175334));
#64551=CARTESIAN_POINT('Ctrl Pts',(7.85330474238622,0.973689622693154,35.6816977440996));
#64552=CARTESIAN_POINT('Ctrl Pts',(7.87262045375448,0.778311114610711,35.6738123128652));
#64553=CARTESIAN_POINT('Ctrl Pts',(7.89194385611916,0.582854812064674,35.6659237418643));
#64554=CARTESIAN_POINT('Ctrl Pts',(7.90397517890498,0.386767287052605,35.6580351708634));
#64555=CARTESIAN_POINT('Ctrl Pts',(7.90870283912137,0.190631588341385,35.6501465998625));
#64556=CARTESIAN_POINT('Ctrl Pts',(7.91343553165706,-0.00571288541193959,
35.6422496319367));
#64557=CARTESIAN_POINT('Ctrl Pts',(7.91084902483556,-0.202105290369741,
35.6343526640108));
#64558=CARTESIAN_POINT('Ctrl Pts',(7.90098385553714,-0.397963710081122,
35.626455696085));
#64559=CARTESIAN_POINT('Ctrl Pts',(7.89111266852429,-0.593941602657351,
35.6185539110398));
#64560=CARTESIAN_POINT('Ctrl Pts',(7.87395399744757,-0.789384517943676,
35.6106521259946));
#64561=CARTESIAN_POINT('Ctrl Pts',(7.84960003056775,-0.983717622140998,
35.6027503409495));
#64562=CARTESIAN_POINT('Ctrl Pts',(7.82521456096634,-1.17830210311438,35.5948383346645));
#64563=CARTESIAN_POINT('Ctrl Pts',(7.79361526042141,-1.37177356625965,35.5869263283796));
#64564=CARTESIAN_POINT('Ctrl Pts',(7.75494523190075,-1.56356817894833,35.5790143220947));
#64565=CARTESIAN_POINT('Ctrl Pts',(7.73874290429313,-1.64392806661943,35.5756992762371));
#64566=CARTESIAN_POINT('Ctrl Pts',(7.72129989716543,-1.7239937681947,35.5723842303794));
#64567=CARTESIAN_POINT('Ctrl Pts',(7.70262930165425,-1.80372471328009,35.5690691845218));
#64568=CARTESIAN_POINT('Ctrl Pts',(7.65847188785192,-1.99229461362846,35.5612288426526));
#64569=CARTESIAN_POINT('Ctrl Pts',(7.60731924415892,-2.17952560368335,35.5533885007834));
#64570=CARTESIAN_POINT('Ctrl Pts',(7.54926404323549,-2.36485378100038,35.5455481589142));
#64571=CARTESIAN_POINT('Ctrl Pts',(7.49127374975459,-2.54997475589924,35.5377165827805));
#64572=CARTESIAN_POINT('Ctrl Pts',(7.42639636982972,-2.73319682218983,35.5298850066469));
#64573=CARTESIAN_POINT('Ctrl Pts',(7.35477565602851,-2.91396569119994,35.5220534305132));
#64574=CARTESIAN_POINT('Ctrl Pts',(7.28322109015136,-3.09456760452386,35.5142290875176));
#64575=CARTESIAN_POINT('Ctrl Pts',(7.20493572193786,-3.27272050820327,35.5064047445219));
#64576=CARTESIAN_POINT('Ctrl Pts',(7.12011328741707,-3.44788453611005,35.4985804015262));
#64577=CARTESIAN_POINT('Ctrl Pts',(7.03535270927447,-3.62292082643872,35.4907617643974));
#64578=CARTESIAN_POINT('Ctrl Pts',(6.94406471220099,-3.79497226723115,35.4829431272686));
#64579=CARTESIAN_POINT('Ctrl Pts',(6.84649145905047,-3.96351809648309,35.4751244901398));
#64580=CARTESIAN_POINT('Ctrl Pts',(6.74897040507044,-4.13197375806928,35.4673100357799));
#64581=CARTESIAN_POINT('Ctrl Pts',(6.64517096884488,-4.29692724050937,35.45949558142));
#64582=CARTESIAN_POINT('Ctrl Pts',(6.53538173784099,-4.45788139598784,35.4516811270601));
#64583=CARTESIAN_POINT('Ctrl Pts',(6.42562991748111,-4.61878070639128,35.443869335473));
#64584=CARTESIAN_POINT('Ctrl Pts',(6.30989256689027,-4.77568311499015,35.4360575438859));
#64585=CARTESIAN_POINT('Ctrl Pts',(6.1885022692311,-4.92811938407762,35.4282457522987));
#64586=CARTESIAN_POINT('Ctrl Pts',(6.06710629031017,-5.08056278742839,35.4204335951071));
#64587=CARTESIAN_POINT('Ctrl Pts',(5.94005704764244,-5.22853935290935,35.4126214379155));
#64588=CARTESIAN_POINT('Ctrl Pts',(5.8077285080673,-5.37161154371595,35.4048092807239));
#64589=CARTESIAN_POINT('Ctrl Pts',(5.67538915051427,-5.51469543080364,35.3969964848814));
#64590=CARTESIAN_POINT('Ctrl Pts',(5.53776987464694,-5.65287388565324,35.3891836890389));
#64591=CARTESIAN_POINT('Ctrl Pts',(5.39528267202063,-5.78574505910811,35.3813708931964));
#64592=CARTESIAN_POINT('Ctrl Pts',(5.25275874908957,-5.91865047472573,35.3735560839222));
#64593=CARTESIAN_POINT('Ctrl Pts',(5.10536465747417,-6.04624564430942,35.3657412746481));
#64594=CARTESIAN_POINT('Ctrl Pts',(4.9535468367383,-6.16816785895455,35.3579264653739));
#64595=CARTESIAN_POINT('Ctrl Pts',(4.80166317517817,-6.2901429492046,35.350108266949));
#64596=CARTESIAN_POINT('Ctrl Pts',(4.6453522367111,-6.40643996352781,35.342290068524));
#64597=CARTESIAN_POINT('Ctrl Pts',(4.48509101177552,-6.51673841857186,35.3344718700991));
#64598=CARTESIAN_POINT('Ctrl Pts',(4.32464324364248,-6.62716526041994,35.3266445713336));
#64599=CARTESIAN_POINT('Ctrl Pts',(4.16023629511131,-6.73157939802848,35.318817272568));
#64600=CARTESIAN_POINT('Ctrl Pts',(3.99237437147008,-6.82970481631739,35.3109899738025));
#64601=CARTESIAN_POINT('Ctrl Pts',(3.82440286688135,-6.92789429127904,35.3031575653444));
#64602=CARTESIAN_POINT('Ctrl Pts',(3.65297220136262,-7.01978670022458,35.2953251568864));
#64603=CARTESIAN_POINT('Ctrl Pts',(3.47860836580684,-7.10515339998643,35.2874927484283));
#64604=CARTESIAN_POINT('Ctrl Pts',(3.30399429357627,-7.19064261299202,35.2796490993604));
#64605=CARTESIAN_POINT('Ctrl Pts',(3.12643896376706,-7.26958726935294,35.2718054502925));
#64606=CARTESIAN_POINT('Ctrl Pts',(2.94648649823127,-7.34180756460838,35.2639618012246));
#64607=CARTESIAN_POINT('Ctrl Pts',(2.84939594789554,-7.38077290020899,35.2597298825211));
#64608=CARTESIAN_POINT('Ctrl Pts',(2.75160784009182,-7.4177816583206,35.2554979638176));
#64609=CARTESIAN_POINT('Ctrl Pts',(2.65320901345151,-7.45281174664567,35.2512660451141));
#64610=CARTESIAN_POINT('Ctrl Pts',(2.46910868581014,-7.51835166168475,35.2433482919612));
#64611=CARTESIAN_POINT('Ctrl Pts',(2.28231966222409,-7.57715815354364,35.2354305388084));
#64612=CARTESIAN_POINT('Ctrl Pts',(2.09337586950565,-7.62900376648036,35.2275127856555));
#64613=CARTESIAN_POINT('Ctrl Pts',(1.90464915961008,-7.68078981253822,35.2196041294313));
#64614=CARTESIAN_POINT('Ctrl Pts',(1.71377294057433,-7.72563081917493,35.2116954732072));
#64615=CARTESIAN_POINT('Ctrl Pts',(1.52130037261706,-7.76334761403064,35.203786816983));
#64616=CARTESIAN_POINT('Ctrl Pts',(1.32901331243296,-7.80102805690799,35.1958857832331));
#64617=CARTESIAN_POINT('Ctrl Pts',(1.13513330392061,-7.83159790058237,35.1879847494832));
#64618=CARTESIAN_POINT('Ctrl Pts',(0.940228182791328,-7.8549278777265,35.1800837157334));
#64619=CARTESIAN_POINT('Ctrl Pts',(0.745474846935986,-7.87823968630249,
35.1721888350316));
#64620=CARTESIAN_POINT('Ctrl Pts',(0.549698329371412,-7.89432282060209,
35.1642939543297));
#64621=CARTESIAN_POINT('Ctrl Pts',(0.353476449613453,-7.90309910095835,
35.1563990736279));
#64622=CARTESIAN_POINT('Ctrl Pts',(0.157371079095513,-7.91187017028638,
35.148508880612));
#64623=CARTESIAN_POINT('Ctrl Pts',(-0.0391787835774433,-7.91334301531703,
35.1406186875962));
#64624=CARTESIAN_POINT('Ctrl Pts',(-0.235590118047823,-7.90749127702827,
35.1327284945803));
#64625=CARTESIAN_POINT('Ctrl Pts',(-0.431921160576763,-7.90164193089997,
35.1248415270347));
#64626=CARTESIAN_POINT('Ctrl Pts',(-0.628113444003138,-7.88847397916084,
35.116954559489));
#64627=CARTESIAN_POINT('Ctrl Pts',(-0.823583578101995,-7.86801316025086,
35.1090675919434));
#64628=CARTESIAN_POINT('Ctrl Pts',(-1.01903673695377,-7.84755411822336,
35.1011813093271));
#64629=CARTESIAN_POINT('Ctrl Pts',(-1.21376752832503,-7.81980350027923,
35.0932950267108));
#64630=CARTESIAN_POINT('Ctrl Pts',(-1.40719678991613,-7.78483899605186,
35.0854087440944));
#64631=CARTESIAN_POINT('Ctrl Pts',(-1.60062571152781,-7.74987455327958,
35.0775224753394));
#64632=CARTESIAN_POINT('Ctrl Pts',(-1.7927527687319,-7.70769631023993,35.0696362065843));
#64633=CARTESIAN_POINT('Ctrl Pts',(-1.98300800320462,-7.65843327706303,
35.0617499378293));
#64634=CARTESIAN_POINT('Ctrl Pts',(-2.17329479104399,-7.60916207373223,
35.0538623611558));
#64635=CARTESIAN_POINT('Ctrl Pts',(-2.36170880402906,-7.55280382540219,
35.0459747844823));
#64636=CARTESIAN_POINT('Ctrl Pts',(-2.54769403726926,-7.48953777562158,
35.0380872078088));
#64637=CARTESIAN_POINT('Ctrl Pts',(-2.73374128792723,-7.42625062955838,
35.0301970009956));
#64638=CARTESIAN_POINT('Ctrl Pts',(-2.91735781917053,-7.35605120339168,
35.0223067941825));
#64639=CARTESIAN_POINT('Ctrl Pts',(-3.09800620248061,-7.27916743655424,
35.0144165873693));
#64640=CARTESIAN_POINT('Ctrl Pts',(-3.27882903094525,-7.20220942603777,
35.0065187612887));
#64641=CARTESIAN_POINT('Ctrl Pts',(-3.4566776692938,-7.11855431692191,34.9986209352081));
#64642=CARTESIAN_POINT('Ctrl Pts',(-3.63103700779795,-7.02847716422282,
34.9907231091275));
#64643=CARTESIAN_POINT('Ctrl Pts',(-3.80549289236293,-6.93835013410198,
34.9828209098713));
#64644=CARTESIAN_POINT('Ctrl Pts',(-3.97645532548991,-6.84179413942413,
34.9749187106152));
#64645=CARTESIAN_POINT('Ctrl Pts',(-4.14343668829894,-6.73912853491149,
34.967016511359));
#64646=CARTESIAN_POINT('Ctrl Pts',(-4.31061961027366,-6.63633900522994,
34.9591047735492));
#64647=CARTESIAN_POINT('Ctrl Pts',(-4.47381157744548,-6.52742532572589,
34.9511930357394));
#64648=CARTESIAN_POINT('Ctrl Pts',(-4.63255577967717,-6.41274886052617,
34.9432812979295));
#64649=CARTESIAN_POINT('Ctrl Pts',(-4.69822246707736,-6.36531138887956,
34.9400085005218));
#64650=CARTESIAN_POINT('Ctrl Pts',(-4.7631284715238,-6.31688826717927,34.9367357031141));
#64651=CARTESIAN_POINT('Ctrl Pts',(-4.82724324427238,-6.26750697332094,
34.9334629057065));
#64652=CARTESIAN_POINT('Ctrl Pts',(-4.9901329845309,-6.14204905176277,34.9251480494447));
#64653=CARTESIAN_POINT('Ctrl Pts',(-5.14826870260402,-6.01013011207214,
34.916833193183));
#64654=CARTESIAN_POINT('Ctrl Pts',(-5.30113670268692,-5.87212658748308,
34.9085183369213));
#64655=CARTESIAN_POINT('Ctrl Pts',(-5.45381645114158,-5.73429300943739,
34.900213720116));
#64656=CARTESIAN_POINT('Ctrl Pts',(-5.60124120300028,-5.59038998637751,
34.8919091033107));
#64657=CARTESIAN_POINT('Ctrl Pts',(-5.7429292391724,-5.44083493168638,34.8836044865055));
#64658=CARTESIAN_POINT('Ctrl Pts',(-5.88445213735088,-5.29145418403159,
34.8753095487655));
#64659=CARTESIAN_POINT('Ctrl Pts',(-6.02025145469556,-5.13643475578282,
34.8670146110256));
#64660=CARTESIAN_POINT('Ctrl Pts',(-6.14988073861615,-4.97623229972216,
34.8587196732856));
#64661=CARTESIAN_POINT('Ctrl Pts',(-6.27931573234284,-4.8162699573558,34.850437168115));
#64662=CARTESIAN_POINT('Ctrl Pts',(-6.40259896399246,-4.65114031746882,
34.8421546629444));
#64663=CARTESIAN_POINT('Ctrl Pts',(-6.51932278113482,-4.48133367150635,
34.8338721577738));
#64664=CARTESIAN_POINT('Ctrl Pts',(-6.63593937082608,-4.31168301713387,
34.8255972612639));
#64665=CARTESIAN_POINT('Ctrl Pts',(-6.74600839679552,-4.13736416539555,
34.8173223647539));
#64666=CARTESIAN_POINT('Ctrl Pts',(-6.84916312819214,-3.95889952428869,
34.809047468244));
#64667=CARTESIAN_POINT('Ctrl Pts',(-6.95219986410578,-3.7806390233239,34.8007820371304));
#64668=CARTESIAN_POINT('Ctrl Pts',(-7.04833794108248,-3.5982424491227,34.7925166060167));
#64669=CARTESIAN_POINT('Ctrl Pts',(-7.13725437163391,-3.41226039958745,
34.7842511749031));
#64670=CARTESIAN_POINT('Ctrl Pts',(-7.17200093136426,-3.33958275887612,
34.7810212286029));
#64671=CARTESIAN_POINT('Ctrl Pts',(-7.20564516586145,-3.26635789443598,
34.7777912823027));
#64672=CARTESIAN_POINT('Ctrl Pts',(-7.23816965150534,-3.1926197856975,34.7745613360024));
#64673=CARTESIAN_POINT('Ctrl Pts',(-7.31840746268982,-3.01070808659052,
34.7665930679041));
#64674=CARTESIAN_POINT('Ctrl Pts',(-7.39175938613969,-2.82582452526994,
34.7586247998057));
#64675=CARTESIAN_POINT('Ctrl Pts',(-7.45802138349776,-2.63852952291427,
34.7506565317073));
#64676=CARTESIAN_POINT('Ctrl Pts',(-7.52431377894204,-2.45114859785996,
34.7426846081184));
#64677=CARTESIAN_POINT('Ctrl Pts',(-7.58350965261639,-2.26135434108176,
34.7347126845296));
#64678=CARTESIAN_POINT('Ctrl Pts',(-7.63545481655088,-2.06972238341522,
34.7267407609407));
#64679=CARTESIAN_POINT('Ctrl Pts',(-7.68745901341395,-1.87787264617471,
34.7187597776828));
#64680=CARTESIAN_POINT('Ctrl Pts',(-7.73219595004951,-1.68418135819225,
34.7107787944248));
#64681=CARTESIAN_POINT('Ctrl Pts',(-7.76956228279999,-1.48923568775792,
34.7027978111669));
#64682=CARTESIAN_POINT('Ctrl Pts',(-7.80695234487526,-1.29416621793553,
34.6948117596207));
#64683=CARTESIAN_POINT('Ctrl Pts',(-7.83696241662768,-1.09784110643337,
34.6868257080745));
#64684=CARTESIAN_POINT('Ctrl Pts',(-7.85954098251039,-0.900853231242278,
34.6788396565284));
#64685=CARTESIAN_POINT('Ctrl Pts',(-7.882149948988,-0.70360012447599,34.6708428522745));
#64686=CARTESIAN_POINT('Ctrl Pts',(-7.89730739062614,-0.505682803529445,
34.6628460480207));
#64687=CARTESIAN_POINT('Ctrl Pts',(-7.90501385848876,-0.307696111611117,
34.6548492437669));
#64688=CARTESIAN_POINT('Ctrl Pts',(-7.90901433267791,-0.204920019511226,
34.6506980541969));
#64689=CARTESIAN_POINT('Ctrl Pts',(-7.91100784171156,-0.102125195674259,
34.6465468646269));
#64690=CARTESIAN_POINT('Ctrl Pts',(-7.91099997681615,0.000605652426356633,
34.6423956750568));
#64691=CARTESIAN_POINT('',(-7.91099996767813,-0.000709561171833796,32.6423600584031));
#64692=CARTESIAN_POINT('Ctrl Pts',(-7.9109999758377,0.000602220688781498,
34.642307277048));
#64693=CARTESIAN_POINT('Ctrl Pts',(-7.91082332165325,2.20207422639699,34.5537279183783));
#64694=CARTESIAN_POINT('Ctrl Pts',(-6.94199696978074,4.38623892820854,34.4651485597086));
#64695=CARTESIAN_POINT('Ctrl Pts',(-3.67820201488358,7.34180684107595,34.2879817653062));
#64696=CARTESIAN_POINT('Ctrl Pts',(-1.40868175871828,8.08992666571321,34.1993943295734));
#64697=CARTESIAN_POINT('Ctrl Pts',(2.97309270521185,7.6545422802529,34.022219458108));
#64698=CARTESIAN_POINT('Ctrl Pts',(5.05102072675523,6.47444880834286,33.9336320223753));
#64699=CARTESIAN_POINT('Ctrl Pts',(7.66951518847832,2.93425195367808,33.7564571509098));
#64700=CARTESIAN_POINT('Ctrl Pts',(8.18956872247062,0.601881960100311,33.6678697151771));
#64701=CARTESIAN_POINT('Ctrl Pts',(7.32306689761398,-3.71537198232339,33.4906948437116));
#64702=CARTESIAN_POINT('Ctrl Pts',(5.9432995885029,-5.66643518936416,33.4021074079789));
#64703=CARTESIAN_POINT('Ctrl Pts',(2.16154501637981,-7.9220591323296,33.2249325365135));
#64704=CARTESIAN_POINT('Ctrl Pts',(-0.210816529298928,-8.20894963713005,
33.1363451007807));
#64705=CARTESIAN_POINT('Ctrl Pts',(-4.42123908576307,-6.91982244717912,
32.9591702293153));
#64706=CARTESIAN_POINT('Ctrl Pts',(-6.22631625634084,-5.3539035880364,32.8705827935826));
#64707=CARTESIAN_POINT('Ctrl Pts',(-7.6530723291585,-2.31356269145162,32.7354502580342));
#64708=CARTESIAN_POINT('Ctrl Pts',(-7.91089457986223,-1.15750112512268,
32.6889051582187));
#64709=CARTESIAN_POINT('Ctrl Pts',(-7.91099996767813,-0.000709561171833796,
32.6423600584031));
#64710=CARTESIAN_POINT('',(-7.89985414996542,-0.000443308007164689,30.6422883933054));
#64711=CARTESIAN_POINT('Ctrl Pts',(-7.91099996745743,-0.000717557340472534,
32.6421607581184));
#64712=CARTESIAN_POINT('Ctrl Pts',(-7.91101730405701,0.190416768768663,
32.6344617805176));
#64713=CARTESIAN_POINT('Ctrl Pts',(-7.90410346812666,0.381778287241483,
32.6267628029168));
#64714=CARTESIAN_POINT('Ctrl Pts',(-7.89023511416832,0.572809604620282,
32.619063825316));
#64715=CARTESIAN_POINT('Ctrl Pts',(-7.87637563695231,0.763718648239245,
32.6113697756137));
#64716=CARTESIAN_POINT('Ctrl Pts',(-7.85557052456921,0.95429755069337,32.6036757259114));
#64717=CARTESIAN_POINT('Ctrl Pts',(-7.82784848039218,1.14398827267673,32.595981676209));
#64718=CARTESIAN_POINT('Ctrl Pts',(-7.80013838581885,1.33359722836102,32.5882909430314));
#64719=CARTESIAN_POINT('Ctrl Pts',(-7.76551734357096,1.52231840649562,32.5806002098538));
#64720=CARTESIAN_POINT('Ctrl Pts',(-7.72406595920795,1.70959821531406,32.5729094766762));
#64721=CARTESIAN_POINT('Ctrl Pts',(-7.68279797660037,1.89604940414253,32.5652527711671));
#64722=CARTESIAN_POINT('Ctrl Pts',(-7.63476005599379,2.08107160339361,32.557596065658));
#64723=CARTESIAN_POINT('Ctrl Pts',(-7.58008228976945,2.2641275318152,32.5499393601489));
#64724=CARTESIAN_POINT('Ctrl Pts',(-7.52104938203463,2.46176405720806,32.5416727900037));
#64725=CARTESIAN_POINT('Ctrl Pts',(-7.45431613058651,2.65697908205414,32.5334062198586));
#64726=CARTESIAN_POINT('Ctrl Pts',(-7.38011585245908,2.84917725041498,32.5251396497135));
#64727=CARTESIAN_POINT('Ctrl Pts',(-7.3058490900229,3.04154763056111,32.5168656726258));
#64728=CARTESIAN_POINT('Ctrl Pts',(-7.22410204983201,3.23089548380066,32.508591695538));
#64729=CARTESIAN_POINT('Ctrl Pts',(-7.13515557910966,3.41664687404191,32.5003177184503));
#64730=CARTESIAN_POINT('Ctrl Pts',(-7.04612363790539,3.60257675659107,32.4920357907289));
#64731=CARTESIAN_POINT('Ctrl Pts',(-6.94987858139909,3.78490301205503,32.4837538630074));
#64732=CARTESIAN_POINT('Ctrl Pts',(-6.84674683060963,3.96307694065318,32.475471935286));
#64733=CARTESIAN_POINT('Ctrl Pts',(-6.7434441268069,4.14154621350514,32.4671762792947));
#64734=CARTESIAN_POINT('Ctrl Pts',(-6.63323205361478,4.31584914412215,32.4588806233035));
#64735=CARTESIAN_POINT('Ctrl Pts',(-6.51648105415954,4.48546493362503,32.4505849673123));
#64736=CARTESIAN_POINT('Ctrl Pts',(-6.39962453439545,4.6552340229761,32.4422818136535));
#64737=CARTESIAN_POINT('Ctrl Pts',(-6.27621746330108,4.82030727749149,32.4339786599947));
#64738=CARTESIAN_POINT('Ctrl Pts',(-6.14667090140141,4.98019656538426,32.4256755063359));
#64739=CARTESIAN_POINT('Ctrl Pts',(-6.01692682805005,5.14032962636446,32.4173596933837));
#64740=CARTESIAN_POINT('Ctrl Pts',(-5.88102474355538,5.29526269852458,32.4090438804315));
#64741=CARTESIAN_POINT('Ctrl Pts',(-5.73941419321809,5.44454274652029,32.4007280674793));
#64742=CARTESIAN_POINT('Ctrl Pts',(-5.6844087286637,5.50252725663729,32.3974979751346));
#64743=CARTESIAN_POINT('Ctrl Pts',(-5.62854236594452,5.55965927475457,32.3942678827898));
#64744=CARTESIAN_POINT('Ctrl Pts',(-5.57184282595133,5.61591386355726,32.391037790445));
#64745=CARTESIAN_POINT('Ctrl Pts',(-5.43297740777338,5.75368953156892,32.3831268246019));
#64746=CARTESIAN_POINT('Ctrl Pts',(-5.28882350508073,5.88648540814427,32.3752158587587));
#64747=CARTESIAN_POINT('Ctrl Pts',(-5.13977266638553,6.0138721251683,32.3673048929155));
#64748=CARTESIAN_POINT('Ctrl Pts',(-4.99087265336391,6.14112993860767,32.3594019322387));
#64749=CARTESIAN_POINT('Ctrl Pts',(-4.83708583466091,6.26298927354107,32.3514989715618));
#64750=CARTESIAN_POINT('Ctrl Pts',(-4.67884126043563,6.37905678448194,32.343596010885));
#64751=CARTESIAN_POINT('Ctrl Pts',(-4.5207275301032,6.49502832546594,32.3356995847395));
#64752=CARTESIAN_POINT('Ctrl Pts',(-4.35816366340133,6.60521738028724,32.3278031585941));
#64753=CARTESIAN_POINT('Ctrl Pts',(-4.19161272993564,6.70926998430094,32.3199067324486));
#64754=CARTESIAN_POINT('Ctrl Pts',(-4.02516869464782,6.81325580373685,32.3120153745039));
#64755=CARTESIAN_POINT('Ctrl Pts',(-3.85474298242594,6.91111283785862,32.3041240165592));
#64756=CARTESIAN_POINT('Ctrl Pts',(-3.68082889719706,7.00252951650752,32.2962326586145));
#64757=CARTESIAN_POINT('Ctrl Pts',(-3.50699426637195,7.09390443052485,32.2883449059163));
#64758=CARTESIAN_POINT('Ctrl Pts',(-3.32967474266194,7.1788446924165,32.280457153218));
#64759=CARTESIAN_POINT('Ctrl Pts',(-3.14938981054062,7.25708376837851,32.2725694005198));
#64760=CARTESIAN_POINT('Ctrl Pts',(-2.9691539001017,7.33530157017697,32.2646837925982));
#64761=CARTESIAN_POINT('Ctrl Pts',(-2.7859545041022,7.40682168089425,32.2567981846765));
#64762=CARTESIAN_POINT('Ctrl Pts',(-2.60033300180316,7.47142484936664,32.2489125767549));
#64763=CARTESIAN_POINT('Ctrl Pts',(-2.41468960705884,7.5360356372221,32.2410260387943));
#64764=CARTESIAN_POINT('Ctrl Pts',(-2.22662385836511,7.59372773310941,32.2331395008336));
#64765=CARTESIAN_POINT('Ctrl Pts',(-2.03669489588992,7.64433089950036,32.225252962873));
#64766=CARTESIAN_POINT('Ctrl Pts',(-1.84674200595547,7.69494044093378,32.2173654313576));
#64767=CARTESIAN_POINT('Ctrl Pts',(-1.6549257674043,7.73845918388771,32.2094778998423));
#64768=CARTESIAN_POINT('Ctrl Pts',(-1.46181816204011,7.77476743453653,32.2015903683269));
#64769=CARTESIAN_POINT('Ctrl Pts',(-1.26865386169985,7.81108634502134,32.1937005210902));
#64770=CARTESIAN_POINT('Ctrl Pts',(-1.07419777761833,7.84019048089693,32.1858106738534));
#64771=CARTESIAN_POINT('Ctrl Pts',(-0.879029956633336,7.86201165957805,
32.1779208266167));
#64772=CARTESIAN_POINT('Ctrl Pts',(-0.683772122693678,7.8838429023607,32.1700273405195));
#64773=CARTESIAN_POINT('Ctrl Pts',(-0.487802239768998,7.89838445616257,
32.1621338544224));
#64774=CARTESIAN_POINT('Ctrl Pts',(-0.291703572906515,7.90562015439356,
32.1542403683252));
#64775=CARTESIAN_POINT('Ctrl Pts',(-0.0953782162571706,7.91286421708166,
32.146337757369));
#64776=CARTESIAN_POINT('Ctrl Pts',(0.101075877358963,7.91278554207477,32.1384351464129));
#64777=CARTESIAN_POINT('Ctrl Pts',(0.297076178164408,7.90542008652084,32.1305325354567));
#64778=CARTESIAN_POINT('Ctrl Pts',(0.493206477049126,7.89804974579546,32.1226246830584));
#64779=CARTESIAN_POINT('Ctrl Pts',(0.688882040664565,7.88338301527019,32.11471683066));
#64780=CARTESIAN_POINT('Ctrl Pts',(0.883527089932634,7.86150754508034,32.1068089782617));
#64781=CARTESIAN_POINT('Ctrl Pts',(1.07843846883588,7.83960214304268,32.0988903056783));
#64782=CARTESIAN_POINT('Ctrl Pts',(1.27231617759625,7.81046835095796,32.090971633095));
#64783=CARTESIAN_POINT('Ctrl Pts',(1.46459506826753,7.77424480486732,32.0830529605116));
#64784=CARTESIAN_POINT('Ctrl Pts',(1.54406350754329,7.75927369356743,32.0797801906868));
#64785=CARTESIAN_POINT('Ctrl Pts',(1.62325902643033,7.74309213452968,32.0765074208621));
#64786=CARTESIAN_POINT('Ctrl Pts',(1.70214257694173,7.72571237153974,32.0732346510373));
#64787=CARTESIAN_POINT('Ctrl Pts',(1.89118556037584,7.68406208798004,32.0653915181184));
#64788=CARTESIAN_POINT('Ctrl Pts',(2.0789953821601,7.63540366148418,32.0575483851995));
#64789=CARTESIAN_POINT('Ctrl Pts',(2.26500689276479,7.57981957408803,32.0497052522807));
#64790=CARTESIAN_POINT('Ctrl Pts',(2.45079995264848,7.5243007642864,32.0418713302866));
#64791=CARTESIAN_POINT('Ctrl Pts',(2.63479857353871,7.46187258822571,32.0340374082926));
#64792=CARTESIAN_POINT('Ctrl Pts',(2.81644624761652,7.3926687694152,32.0262034862985));
#64793=CARTESIAN_POINT('Ctrl Pts',(2.99791592318182,7.3235327641722,32.0183772408491));
#64794=CARTESIAN_POINT('Ctrl Pts',(3.17703891368189,7.24763446245187,32.0105509953995));
#64795=CARTESIAN_POINT('Ctrl Pts',(3.3532721819272,7.16515782616916,32.0027247499501));
#64796=CARTESIAN_POINT('Ctrl Pts',(3.52936701146528,7.08274597878255,31.9949046523483));
#64797=CARTESIAN_POINT('Ctrl Pts',(3.70257632308965,6.99376623725406,31.9870845547466));
#64798=CARTESIAN_POINT('Ctrl Pts',(3.87237526095857,6.89845133622874,31.9792644571449));
#64799=CARTESIAN_POINT('Ctrl Pts',(4.04207380478795,6.80319279037302,31.9714489831951));
#64800=CARTESIAN_POINT('Ctrl Pts',(4.20836568583172,6.70160671794843,31.9636335092453));
#64801=CARTESIAN_POINT('Ctrl Pts',(4.37074877749668,6.59397271180366,31.9558180352955));
#64802=CARTESIAN_POINT('Ctrl Pts',(4.53306740055944,6.48638143802624,31.9480056642099));
#64803=CARTESIAN_POINT('Ctrl Pts',(4.69148003350514,6.37274720845049,31.9401932931243));
#64804=CARTESIAN_POINT('Ctrl Pts',(4.84551162107078,6.25339412879662,31.9323809220387));
#64805=CARTESIAN_POINT('Ctrl Pts',(4.99953737799311,6.13404556708123,31.9245688466791));
#64806=CARTESIAN_POINT('Ctrl Pts',(5.14918213653042,6.0089787947287,31.9167567713195));
#64807=CARTESIAN_POINT('Ctrl Pts',(5.2940017910241,5.87855986076808,31.9089446959599));
#64808=CARTESIAN_POINT('Ctrl Pts',(5.4388256810409,5.7481371124605,31.9011323921215));
#64809=CARTESIAN_POINT('Ctrl Pts',(5.57882392393806,5.61236212559122,31.8933200882831));
#64810=CARTESIAN_POINT('Ctrl Pts',(5.71358736844511,5.47163964302699,31.8855077844447));
#64811=CARTESIAN_POINT('Ctrl Pts',(5.8483784664225,5.33088828419729,31.8776938775209));
#64812=CARTESIAN_POINT('Ctrl Pts',(5.97793238286326,5.18518766132498,31.8698799705971));
#64813=CARTESIAN_POINT('Ctrl Pts',(6.10187844259713,5.03497770320469,31.8620660636732));
#64814=CARTESIAN_POINT('Ctrl Pts',(6.22587174632039,4.88471049019722,31.8542491783559));
#64815=CARTESIAN_POINT('Ctrl Pts',(6.34425271182407,4.72993078924735,31.8464322930386));
#64816=CARTESIAN_POINT('Ctrl Pts',(6.4566923009425,4.57110987955331,31.8386154077213));
#64817=CARTESIAN_POINT('Ctrl Pts',(6.5692538632265,4.41211668277367,31.8307900427373));
#64818=CARTESIAN_POINT('Ctrl Pts',(6.67586097316177,4.24907380864018,31.8229646777532));
#64819=CARTESIAN_POINT('Ctrl Pts',(6.77622856060272,4.08248055653324,31.8151393127691));
#64820=CARTESIAN_POINT('Ctrl Pts',(6.87665714701675,3.91578605642824,31.8073091918749));
#64821=CARTESIAN_POINT('Ctrl Pts',(6.97083848387219,3.74553718491091,31.7994790709807));
#64822=CARTESIAN_POINT('Ctrl Pts',(7.05853444472115,3.57225593885505,31.7916489500865));
#64823=CARTESIAN_POINT('Ctrl Pts',(7.14635028013734,3.39873782881844,31.7838081259359));
#64824=CARTESIAN_POINT('Ctrl Pts',(7.22766288666815,3.22217938360985,31.7759673017853));
#64825=CARTESIAN_POINT('Ctrl Pts',(7.30228263624338,3.04312163746677,31.7681264776346));
#64826=CARTESIAN_POINT('Ctrl Pts',(7.34255455859735,2.94648502731197,31.7638948222997));
#64827=CARTESIAN_POINT('Ctrl Pts',(7.38087790776481,2.84912070401904,31.7596631669647));
#64828=CARTESIAN_POINT('Ctrl Pts',(7.41722899812936,2.75111522646889,31.7554315116297));
#64829=CARTESIAN_POINT('Ctrl Pts',(7.48518817495826,2.5678917932173,31.7475203372934));
#64830=CARTESIAN_POINT('Ctrl Pts',(7.54644557606945,2.38190244921842,31.7396091629571));
#64831=CARTESIAN_POINT('Ctrl Pts',(7.60076925248574,2.19367904910163,31.7316979886208));
#64832=CARTESIAN_POINT('Ctrl Pts',(7.6550340349838,2.00565970758809,31.7237953910246));
#64833=CARTESIAN_POINT('Ctrl Pts',(7.70237997089292,1.81541146255084,31.7158927934285));
#64834=CARTESIAN_POINT('Ctrl Pts',(7.74262326082517,1.62348576862533,31.7079901958323));
#64835=CARTESIAN_POINT('Ctrl Pts',(7.7828303920864,1.43173252029361,31.7000946987347));
#64836=CARTESIAN_POINT('Ctrl Pts',(7.81594752004121,1.23830516089803,31.6921992016372));
#64837=CARTESIAN_POINT('Ctrl Pts',(7.84184065013985,1.04377019396713,31.6843037045397));
#64838=CARTESIAN_POINT('Ctrl Pts',(7.86771532020873,0.849373917154589,31.6764138363913));
#64839=CARTESIAN_POINT('Ctrl Pts',(7.88637620810694,0.653871946477836,31.6685239682429));
#64840=CARTESIAN_POINT('Ctrl Pts',(7.89774034043308,0.457841146136858,31.6606341000945));
#64841=CARTESIAN_POINT('Ctrl Pts',(7.90909847928391,0.261913732990894,31.6527483930847));
#64842=CARTESIAN_POINT('Ctrl Pts',(7.91316751097663,0.0654583893702774,
31.6448626860749));
#64843=CARTESIAN_POINT('Ctrl Pts',(7.90991624966504,-0.130942442641423,
31.6369769790651));
#64844=CARTESIAN_POINT('Ctrl Pts',(7.90666609997367,-0.327276124364865,
31.6290939682124));
#64845=CARTESIAN_POINT('Ctrl Pts',(7.89610065123511,-0.523554987258206,
31.6212109573598));
#64846=CARTESIAN_POINT('Ctrl Pts',(7.8782408148018,-0.719195845365574,31.6133279465071));
#64847=CARTESIAN_POINT('Ctrl Pts',(7.86038071183727,-0.914839623118703,
31.6054448180123));
#64848=CARTESIAN_POINT('Ctrl Pts',(7.83522602659116,-1.10984503292152,31.5975616895176));
#64849=CARTESIAN_POINT('Ctrl Pts',(7.80284965968011,-1.30363268923034,31.5896785610228));
#64850=CARTESIAN_POINT('Ctrl Pts',(7.77047129090595,-1.4974323276236,31.5817949451063));
#64851=CARTESIAN_POINT('Ctrl Pts',(7.73087040698091,-1.69001372207064,31.5739113291898));
#64852=CARTESIAN_POINT('Ctrl Pts',(7.68417129613581,-1.88080634081302,31.5660277132734));
#64853=CARTESIAN_POINT('Ctrl Pts',(7.63746144796589,-2.07164282767804,31.5581422847111));
#64854=CARTESIAN_POINT('Ctrl Pts',(7.58365020274053,-2.26068938422741,31.5502568561489));
#64855=CARTESIAN_POINT('Ctrl Pts',(7.52291217691596,-2.44738909420009,31.5423714275867));
#64856=CARTESIAN_POINT('Ctrl Pts',(7.46214997598967,-2.63416311486068,31.5344828604464));
#64857=CARTESIAN_POINT('Ctrl Pts',(7.39445560748082,-2.81858809992278,31.526594293306));
#64858=CARTESIAN_POINT('Ctrl Pts',(7.32005250441971,-3.00012538613618,31.5187057261657));
#64859=CARTESIAN_POINT('Ctrl Pts',(7.24557022028299,-3.18185586748518,31.5108087638751));
#64860=CARTESIAN_POINT('Ctrl Pts',(7.16436507186001,-3.36069219243615,31.5029118015845));
#64861=CARTESIAN_POINT('Ctrl Pts',(7.07670777418312,-3.53611765624621,31.4950148392939));
#64862=CARTESIAN_POINT('Ctrl Pts',(6.98899701721613,-3.71165010625147,31.4871130609069));
#64863=CARTESIAN_POINT('Ctrl Pts',(6.89482643122074,-3.88376724624117,31.4792112825198));
#64864=CARTESIAN_POINT('Ctrl Pts',(6.79451119570603,-4.05197959168422,31.4713095041328));
#64865=CARTESIAN_POINT('Ctrl Pts',(6.69406621795305,-4.22040949377348,31.4633975060178));
#64866=CARTESIAN_POINT('Ctrl Pts',(6.58746090398517,-4.38492422541705,31.4554855079029));
#64867=CARTESIAN_POINT('Ctrl Pts',(6.47505265009752,-4.5450648156506,31.4475735097879));
#64868=CARTESIAN_POINT('Ctrl Pts',(6.42795474755298,-4.61216207631781,31.4442584639326));
#64869=CARTESIAN_POINT('Ctrl Pts',(6.37983859997287,-4.67849185985307,31.4409434180773));
#64870=CARTESIAN_POINT('Ctrl Pts',(6.33073248300737,-4.74402226265807,31.4376283722221));
#64871=CARTESIAN_POINT('Ctrl Pts',(6.2135435582011,-4.90040680131411,31.4297172058853));
#64872=CARTESIAN_POINT('Ctrl Pts',(6.09039907079601,-5.05265666110265,31.4218060395486));
#64873=CARTESIAN_POINT('Ctrl Pts',(5.96162041120069,-5.20028874897879,31.4138948732119));
#64874=CARTESIAN_POINT('Ctrl Pts',(5.83298134359543,-5.34776080834547,31.405992282329));
#64875=CARTESIAN_POINT('Ctrl Pts',(5.69872049319156,-5.49062480853605,31.3980896914461));
#64876=CARTESIAN_POINT('Ctrl Pts',(5.55920180975748,-5.62842751027222,31.3901871005632));
#64877=CARTESIAN_POINT('Ctrl Pts',(5.41980846159799,-5.76610641826955,31.3822916088972));
#64878=CARTESIAN_POINT('Ctrl Pts',(5.27516693347967,-5.89873284458451,31.3743961172313));
#64879=CARTESIAN_POINT('Ctrl Pts',(5.12568080582907,-6.02588726054142,31.3665006255653));
#64880=CARTESIAN_POINT('Ctrl Pts',(4.97630122743358,-6.15295104462155,31.3586107615704));
#64881=CARTESIAN_POINT('Ctrl Pts',(4.82208419082698,-6.27455036654056,31.3507208975755));
#64882=CARTESIAN_POINT('Ctrl Pts',(4.66346962535559,-6.39030297039082,31.3428310335807));
#64883=CARTESIAN_POINT('Ctrl Pts',(4.50493868805716,-6.50599454467078,31.3349453294491));
#64884=CARTESIAN_POINT('Ctrl Pts',(4.34201511982195,-6.61584534065912,31.3270596253175));
#64885=CARTESIAN_POINT('Ctrl Pts',(4.17517159395903,-6.71951361044813,31.3191739211859));
#64886=CARTESIAN_POINT('Ctrl Pts',(4.00838508569865,-6.82314645233442,31.3112909119383));
#64887=CARTESIAN_POINT('Ctrl Pts',(3.8376815822631,-6.92060079721286,31.3034079026907));
#64888=CARTESIAN_POINT('Ctrl Pts',(3.66356260546471,-7.01157828422679,31.2955248934431));
#64889=CARTESIAN_POINT('Ctrl Pts',(3.48944098816572,-7.10255715090715,31.2876417646503));
#64890=CARTESIAN_POINT('Ctrl Pts',(3.31190409569383,-7.18705879629818,31.2797586358574));
#64891=CARTESIAN_POINT('Ctrl Pts',(3.13147842034112,-7.26483061763575,31.2718755070646));
#64892=CARTESIAN_POINT('Ctrl Pts',(2.95104156192538,-7.34260725939136,31.2639918896632));
#64893=CARTESIAN_POINT('Ctrl Pts',(2.76771588046419,-7.41365310879269,31.2561082722619));
#64894=CARTESIAN_POINT('Ctrl Pts',(2.58204826506268,-7.47776355315457,31.2482246548605));
#64895=CARTESIAN_POINT('Ctrl Pts',(2.39633793195291,-7.54188874780692,31.240339223626));
#64896=CARTESIAN_POINT('Ctrl Pts',(2.20828491727192,-7.59907524520427,31.2324537923915));
#64897=CARTESIAN_POINT('Ctrl Pts',(2.01845193058505,-7.64916811188756,31.2245683611571));
#64898=CARTESIAN_POINT('Ctrl Pts',(1.8285433575136,-7.69928092420175,31.2166797901562));
#64899=CARTESIAN_POINT('Ctrl Pts',(1.63685373345786,-7.74229438980108,31.2087912191553));
#64900=CARTESIAN_POINT('Ctrl Pts',(1.44395687147668,-7.77810449616841,31.2009026481544));
#64901=CARTESIAN_POINT('Ctrl Pts',(1.25085468200666,-7.81395272031091,31.1930056802285));
#64902=CARTESIAN_POINT('Ctrl Pts',(1.05654302709883,-7.84258220703017,31.1851087123026));
#64903=CARTESIAN_POINT('Ctrl Pts',(0.861602877452391,-7.8639405822759,31.1772117443768));
#64904=CARTESIAN_POINT('Ctrl Pts',(0.666543815081898,-7.88531198604647,
31.1693099593316));
#64905=CARTESIAN_POINT('Ctrl Pts',(0.470855836739858,-7.89940341115062,
31.1614081742864));
#64906=CARTESIAN_POINT('Ctrl Pts',(0.275121121529162,-7.90621460425206,
31.1535063892411));
#64907=CARTESIAN_POINT('Ctrl Pts',(0.0791332165088265,-7.91303460787381,
31.1455943829562));
#64908=CARTESIAN_POINT('Ctrl Pts',(-0.116901202330898,-7.91255557032341,
31.1376823766712));
#64909=CARTESIAN_POINT('Ctrl Pts',(-0.312402733260923,-7.90482925383282,
31.1297703703863));
#64910=CARTESIAN_POINT('Ctrl Pts',(-0.394315779947933,-7.9015920100097,
31.1264553245289));
#64911=CARTESIAN_POINT('Ctrl Pts',(-0.47613536764902,-7.89708311507568,
31.1231402786716));
#64912=CARTESIAN_POINT('Ctrl Pts',(-0.557819362036135,-7.89130905232697,
31.1198252328143));
#64913=CARTESIAN_POINT('Ctrl Pts',(-0.751008376246334,-7.87765294382273,
31.1119848909451));
#64914=CARTESIAN_POINT('Ctrl Pts',(-0.943986168014457,-7.8568777548247,
31.1041445490759));
#64915=CARTESIAN_POINT('Ctrl Pts',(-1.13618127400415,-7.82898544593118,
31.0963042072067));
#64916=CARTESIAN_POINT('Ctrl Pts',(-1.32816150014477,-7.80112432146921,
31.0884726310731));
#64917=CARTESIAN_POINT('Ctrl Pts',(-1.51936043865765,-7.76616197153333,
31.0806410549395));
#64918=CARTESIAN_POINT('Ctrl Pts',(-1.70920800755183,-7.72415231510363,
31.0728094788059));
#64919=CARTESIAN_POINT('Ctrl Pts',(-1.89888023579474,-7.68218145822538,
31.0649851358102));
#64920=CARTESIAN_POINT('Ctrl Pts',(-2.08720323917296,-7.63317633233087,
31.0571607928146));
#64921=CARTESIAN_POINT('Ctrl Pts',(-2.27361323890234,-7.57724249578222,
31.049336449819));
#64922=CARTESIAN_POINT('Ctrl Pts',(-2.4598872999808,-7.52134944873142,31.0415178126901));
#64923=CARTESIAN_POINT('Ctrl Pts',(-2.64425080075974,-7.45853785530182,
31.0336991755613));
#64924=CARTESIAN_POINT('Ctrl Pts',(-2.82615113501385,-7.38896411968958,
31.0258805384325));
#64925=CARTESIAN_POINT('Ctrl Pts',(-3.00795415728584,-7.31942760422947,
31.0180660840726));
#64926=CARTESIAN_POINT('Ctrl Pts',(-3.18729631045722,-7.24313627821234,
31.0102516297128));
#64927=CARTESIAN_POINT('Ctrl Pts',(-3.3636409316227,-7.160296130965,31.0024371753529));
#64928=CARTESIAN_POINT('Ctrl Pts',(-3.53992546341619,-7.07748421147075,
30.9946253837659));
#64929=CARTESIAN_POINT('Ctrl Pts',(-3.71321418047056,-6.98812806626,30.9868135921788));
#64930=CARTESIAN_POINT('Ctrl Pts',(-3.88299099028596,-6.89248155379164,
30.9790018005917));
#64931=CARTESIAN_POINT('Ctrl Pts',(-4.05277574593132,-6.79683056491143,
30.9711896434001));
#64932=CARTESIAN_POINT('Ctrl Pts',(-4.21904795512081,-6.69488878522707,
30.9633774862085));
#64933=CARTESIAN_POINT('Ctrl Pts',(-4.3813162531998,-6.58695596534904,30.9555653290169));
#64934=CARTESIAN_POINT('Ctrl Pts',(-4.54359781685918,-6.47901432186519,
30.9477525331744));
#64935=CARTESIAN_POINT('Ctrl Pts',(-4.70187452392754,-6.36508085674399,
30.9399397373319));
#64936=CARTESIAN_POINT('Ctrl Pts',(-4.85568420710096,-6.24549852941383,
30.9321269414894));
#64937=CARTESIAN_POINT('Ctrl Pts',(-5.00953352848999,-6.12588538458261,
30.9243121322152));
#64938=CARTESIAN_POINT('Ctrl Pts',(-5.15891325492716,-6.00062069333281,
30.916497322941));
#64939=CARTESIAN_POINT('Ctrl Pts',(-5.30339439317307,-5.8700876407819,30.9086825136668));
#64940=CARTESIAN_POINT('Ctrl Pts',(-5.44793819044681,-5.73949797825219,
30.9008643152419));
#64941=CARTESIAN_POINT('Ctrl Pts',(-5.58757890682345,-5.60363563853184,
30.893046116817));
#64942=CARTESIAN_POINT('Ctrl Pts',(-5.72192438807513,-5.46292067461637,
30.8852279183922));
#64943=CARTESIAN_POINT('Ctrl Pts',(-5.85642624673967,-5.32204191924472,
30.8774006196266));
#64944=CARTESIAN_POINT('Ctrl Pts',(-5.98562031693983,-5.17629951264028,
30.8695733208611));
#64945=CARTESIAN_POINT('Ctrl Pts',(-6.10915402742201,-5.02614743807157,
30.8617460220956));
#64946=CARTESIAN_POINT('Ctrl Pts',(-6.23276838121355,-4.87589734361702,
30.8539136136375));
#64947=CARTESIAN_POINT('Ctrl Pts',(-6.35071479910128,-4.72123212319134,
30.8460812051795));
#64948=CARTESIAN_POINT('Ctrl Pts',(-6.46268402166588,-4.56263479100667,
30.8382487967214));
#64949=CARTESIAN_POINT('Ctrl Pts',(-6.57481393584329,-4.40380984930117,
30.8304051476535));
#64950=CARTESIAN_POINT('Ctrl Pts',(-6.68094933047527,-4.24104181829432,
30.8225614985856));
#64951=CARTESIAN_POINT('Ctrl Pts',(-6.78082628644783,-4.07483936775649,
30.8147178495177));
#64952=CARTESIAN_POINT('Ctrl Pts',(-6.8347133426367,-3.98516742387666,30.810485930814));
#64953=CARTESIAN_POINT('Ctrl Pts',(-6.88677940065042,-3.89449610642381,
30.8062540121104));
#64954=CARTESIAN_POINT('Ctrl Pts',(-6.93698886021879,-3.8029076445794,30.8020220934067));
#64955=CARTESIAN_POINT('Ctrl Pts',(-7.03702128819584,-3.62043573008878,
30.7935908315175));
#64956=CARTESIAN_POINT('Ctrl Pts',(-7.12994872693167,-3.43383525325003,
30.7851595696284));
#64957=CARTESIAN_POINT('Ctrl Pts',(-7.2154380065385,-3.24366696407009,30.7767283077393));
#64958=CARTESIAN_POINT('Ctrl Pts',(-7.30078206904377,-3.05382170589345,
30.7683113676859));
#64959=CARTESIAN_POINT('Ctrl Pts',(-7.37871306135141,-2.86042097340825,
30.7598944276324));
#64960=CARTESIAN_POINT('Ctrl Pts',(-7.44894322862298,-2.66405063329356,
30.751477487579));
#64961=CARTESIAN_POINT('Ctrl Pts',(-7.5190551931533,-2.46801079947557,30.7430747138792));
#64962=CARTESIAN_POINT('Ctrl Pts',(-7.58149209220624,-2.26901158538908,
30.7346719401795));
#64963=CARTESIAN_POINT('Ctrl Pts',(-7.63601347913692,-2.06766030731337,
30.7262691664797));
#64964=CARTESIAN_POINT('Ctrl Pts',(-7.69040594310445,-1.86678515071707,
30.7178862622393));
#64965=CARTESIAN_POINT('Ctrl Pts',(-7.73692016983713,-1.66356929268312,
30.7095033579989));
#64966=CARTESIAN_POINT('Ctrl Pts',(-7.77536500274913,-1.45863637484604,
30.7011204537585));
#64967=CARTESIAN_POINT('Ctrl Pts',(-7.81375381875048,-1.25400205913772,
30.6927497640178));
#64968=CARTESIAN_POINT('Ctrl Pts',(-7.84409663700915,-1.04765594202256,
30.6843790742771));
#64969=CARTESIAN_POINT('Ctrl Pts',(-7.86625228079528,-0.840235713882164,
30.6760083845363));
#64970=CARTESIAN_POINT('Ctrl Pts',(-7.88836370980692,-0.633229422646547,
30.6676543997112));
#64971=CARTESIAN_POINT('Ctrl Pts',(-7.90232053262437,-0.425153570025834,
30.6593004148861));
#64972=CARTESIAN_POINT('Ctrl Pts',(-7.90803273194084,-0.216654818899259,
30.6509464300609));
#64973=CARTESIAN_POINT('Ctrl Pts',(-7.90999627195931,-0.144984413341794,
30.648074789453));
#64974=CARTESIAN_POINT('Ctrl Pts',(-7.91098606472354,-0.0732641305949829,
30.645203148845));
#64975=CARTESIAN_POINT('Ctrl Pts',(-7.91099985387987,-0.00152049748538701,
30.6423315082371));
#64976=CARTESIAN_POINT('',(-7.91184153648199,4.99451412439681E-5,28.6437895940631));
#64977=CARTESIAN_POINT('Ctrl Pts',(-7.89546650976364,-1.92594324088665E-5,
30.6422714205947));
#64978=CARTESIAN_POINT('Ctrl Pts',(-7.89546412269911,0.00218135211731857,
30.6421831647693));
#64979=CARTESIAN_POINT('Ctrl Pts',(-7.89546128372232,0.00411991532010145,
30.6421054184775));
#64980=CARTESIAN_POINT('Ctrl Pts',(-7.89545723413254,0.00631726536019909,
30.6420172935349));
#64981=CARTESIAN_POINT('Ctrl Pts',(-7.89502030649362,0.243398801313106,
30.632509114881));
#64982=CARTESIAN_POINT('Ctrl Pts',(-7.88409107758035,0.480852628331748,
30.6232175521955));
#64983=CARTESIAN_POINT('Ctrl Pts',(-7.86274775425919,0.717537746077602,
30.6140618702597));
#64984=CARTESIAN_POINT('Ctrl Pts',(-7.84133330654603,0.955011592216039,
30.6048756779718));
#64985=CARTESIAN_POINT('Ctrl Pts',(-7.80943596256734,1.1917110943165,30.5958262735592));
#64986=CARTESIAN_POINT('Ctrl Pts',(-7.76716639284816,1.42652545074094,30.5868321119856));
#64987=CARTESIAN_POINT('Ctrl Pts',(-7.72491866505277,1.66121847171497,30.5778425979586));
#64988=CARTESIAN_POINT('Ctrl Pts',(-7.67231018451083,1.8940279712867,30.568908269694));
#64989=CARTESIAN_POINT('Ctrl Pts',(-7.60947191037755,2.12389257139215,30.5599477085005));
#64990=CARTESIAN_POINT('Ctrl Pts',(-7.54678661352194,2.35319757527631,30.5510089614365));
#64991=CARTESIAN_POINT('Ctrl Pts',(-7.4739220288526,2.57957185345583,30.5420441090141));
#64992=CARTESIAN_POINT('Ctrl Pts',(-7.39101717471166,2.80201274063794,30.5329723257269));
#64993=CARTESIAN_POINT('Ctrl Pts',(-7.30838812292402,3.02371362627498,30.5239307218448));
#64994=CARTESIAN_POINT('Ctrl Pts',(-7.21578623579024,3.24150726677263,30.5147828973754));
#64995=CARTESIAN_POINT('Ctrl Pts',(-7.11334689049767,3.45445261467261,30.5054488307867));
#64996=CARTESIAN_POINT('Ctrl Pts',(-7.06218249042566,3.56081039099685,30.5007868338178));
#64997=CARTESIAN_POINT('Ctrl Pts',(-7.00856392603403,3.66595951555365,30.4960783767544));
#64998=CARTESIAN_POINT('Ctrl Pts',(-6.95250697360272,3.76978749396466,30.4913134892526));
#64999=CARTESIAN_POINT('Ctrl Pts',(-6.84121380227646,3.97592329850941,30.4818534772809));
#65000=CARTESIAN_POINT('Ctrl Pts',(-6.72031101138611,4.17684884004786,30.4721710362662));
#65001=CARTESIAN_POINT('Ctrl Pts',(-6.59068832436126,4.37211674975882,30.4621881423824));
#65002=CARTESIAN_POINT('Ctrl Pts',(-6.47029688634264,4.55347840016564,30.452916193329));
#65003=CARTESIAN_POINT('Ctrl Pts',(-6.34238358593672,4.72996025928655,30.4433850618682));
#65004=CARTESIAN_POINT('Ctrl Pts',(-6.20763774264494,4.90123666969266,30.433532234907));
#65005=CARTESIAN_POINT('Ctrl Pts',(-6.09888078764801,5.03947841729326,30.4255797561349));
#65006=CARTESIAN_POINT('Ctrl Pts',(-5.98543685338641,5.17396077302761,30.4176635528211));
#65007=CARTESIAN_POINT('Ctrl Pts',(-5.86747184415262,5.30437293182994,30.4098965082411));
#65008=CARTESIAN_POINT('Ctrl Pts',(-5.74963212763683,5.43464657757706,30.4021377131763));
#65009=CARTESIAN_POINT('Ctrl Pts',(-5.62728033527176,5.56085838282157,30.3945277601652));
#65010=CARTESIAN_POINT('Ctrl Pts',(-5.50060359947352,5.68265147185828,30.3871791731794));
#65011=CARTESIAN_POINT('Ctrl Pts',(-5.43746134417914,5.74335946431315,30.3835162562863));
#65012=CARTESIAN_POINT('Ctrl Pts',(-5.3732449336438,5.80296890158039,30.3799182768963));
#65013=CARTESIAN_POINT('Ctrl Pts',(-5.30798024592445,5.86143156577821,30.3763991702581));
#65014=CARTESIAN_POINT('Ctrl Pts',(-5.08331837819765,6.06267869941112,30.3642852829831));
#65015=CARTESIAN_POINT('Ctrl Pts',(-4.84690886434787,6.2514706121673,30.3523459441257));
#65016=CARTESIAN_POINT('Ctrl Pts',(-4.60054071673013,6.42659030156861,30.3405140373188));
#65017=CARTESIAN_POINT('Ctrl Pts',(-4.50088145039366,6.49742859757221,30.3357278701005));
#65018=CARTESIAN_POINT('Ctrl Pts',(-4.39959251112845,6.56603028009268,30.3309592821233));
#65019=CARTESIAN_POINT('Ctrl Pts',(-4.29679155596662,6.63231708308071,30.326203830883));
#65020=CARTESIAN_POINT('Ctrl Pts',(-4.04082351634497,6.79736713526092,30.3143630505171));
#65021=CARTESIAN_POINT('Ctrl Pts',(-3.77548350392549,6.94806249708131,30.3026037152006));
#65022=CARTESIAN_POINT('Ctrl Pts',(-3.5026855417861,7.08340682054121,30.2908572455461));
#65023=CARTESIAN_POINT('Ctrl Pts',(-3.22956687612411,7.21891025589828,30.2790969666455));
#65024=CARTESIAN_POINT('Ctrl Pts',(-2.94897345341156,7.33902731325784,30.2673495836747));
#65025=CARTESIAN_POINT('Ctrl Pts',(-2.66278861089816,7.44279415657953,30.2555462750944));
#65026=CARTESIAN_POINT('Ctrl Pts',(-2.37764267387871,7.54618430649331,30.2437858147727));
#65027=CARTESIAN_POINT('Ctrl Pts',(-2.08694631195099,7.63334365571279,30.2319698341457));
#65028=CARTESIAN_POINT('Ctrl Pts',(-1.79251626616018,7.70334184067585,30.2200302584625));
#65029=CARTESIAN_POINT('Ctrl Pts',(-1.5006846181593,7.7727222791429,30.2081960516692));
#65030=CARTESIAN_POINT('Ctrl Pts',(-1.20518508910376,7.82524412846403,30.1962404216906));
#65031=CARTESIAN_POINT('Ctrl Pts',(-0.907736453985132,7.86000968883437,
30.1840970802323));
#65032=CARTESIAN_POINT('Ctrl Pts',(-0.805063307239477,7.87201004472833,
30.1799054486956));
#65033=CARTESIAN_POINT('Ctrl Pts',(-0.702157472595626,7.8818947616983,30.1756914515555));
#65034=CARTESIAN_POINT('Ctrl Pts',(-0.599088191656171,7.88962680232436,
30.1714523625255));
#65035=CARTESIAN_POINT('Ctrl Pts',(-0.306040219117324,7.91161064473019,
30.1593997273045));
#65036=CARTESIAN_POINT('Ctrl Pts',(-0.0116744980615128,7.9161938128868,
30.1471442526803));
#65037=CARTESIAN_POINT('Ctrl Pts',(0.28236443491014,7.90424368096634,30.1346232772743));
#65038=CARTESIAN_POINT('Ctrl Pts',(0.449042743781442,7.89746965359806,30.127525662734));
#65039=CARTESIAN_POINT('Ctrl Pts',(0.615616935621651,7.88538273710484,30.1203427353734));
#65040=CARTESIAN_POINT('Ctrl Pts',(0.781794208160822,7.86813767748803,30.1130630815916));
#65041=CARTESIAN_POINT('Ctrl Pts',(0.990485363128304,7.84648073635568,30.1039210410931));
#65042=CARTESIAN_POINT('Ctrl Pts',(1.19810556530782,7.81614683836484,30.0949825327481));
#65043=CARTESIAN_POINT('Ctrl Pts',(1.40410903431245,7.77756160137206,30.0861910988723));
#65044=CARTESIAN_POINT('Ctrl Pts',(1.61232268313516,7.7385623892531,30.0773053430425));
#65045=CARTESIAN_POINT('Ctrl Pts',(1.81888521446852,7.69113406978758,30.0685698344904));
#65046=CARTESIAN_POINT('Ctrl Pts',(2.02326640029138,7.63567381629991,30.059926278788));
#65047=CARTESIAN_POINT('Ctrl Pts',(2.23031076776408,7.57949088998504,30.0511700935456));
#65048=CARTESIAN_POINT('Ctrl Pts',(2.43511714741324,7.51506559391288,30.0425082731425));
#65049=CARTESIAN_POINT('Ctrl Pts',(2.63716020931853,7.44276395616095,30.0338802145172));
#65050=CARTESIAN_POINT('Ctrl Pts',(2.7593900790063,7.39902367783961,30.0286605030781));
#65051=CARTESIAN_POINT('Ctrl Pts',(2.88060907249666,7.35239983002036,30.0234531480436));
#65052=CARTESIAN_POINT('Ctrl Pts',(3.00070395312335,7.30296474165692,30.0182447311977));
#65053=CARTESIAN_POINT('Ctrl Pts',(3.25343976420335,7.19893018924178,30.0072837855759));
#65054=CARTESIAN_POINT('Ctrl Pts',(3.50117487065036,7.08200517932002,29.9965506364678));
#65055=CARTESIAN_POINT('Ctrl Pts',(3.74248687266088,6.95291237079717,29.9859497658109));
#65056=CARTESIAN_POINT('Ctrl Pts',(3.99168009790156,6.81960340546115,29.9750026718937));
#65057=CARTESIAN_POINT('Ctrl Pts',(4.23402402383837,6.67332010383523,29.964196637924));
#65058=CARTESIAN_POINT('Ctrl Pts',(4.46800670144774,6.51483954969744,29.9534264780255));
#65059=CARTESIAN_POINT('Ctrl Pts',(4.69448803737438,6.36143978529503,29.9430016028729));
#65060=CARTESIAN_POINT('Ctrl Pts',(4.91313658488023,6.19661310307585,29.9326103384614));
#65061=CARTESIAN_POINT('Ctrl Pts',(5.12262184026173,6.02103222294843,29.9221572946339));
#65062=CARTESIAN_POINT('Ctrl Pts',(5.32917845457106,5.84790599470614,29.9118503862153));
#65063=CARTESIAN_POINT('Ctrl Pts',(5.52682713705019,5.66432485566542,29.9014834136807));
#65064=CARTESIAN_POINT('Ctrl Pts',(5.71431895097915,5.4708910518928,29.8909649319167));
#65065=CARTESIAN_POINT('Ctrl Pts',(5.89586083992772,5.28359573810009,29.8807802470055));
#65066=CARTESIAN_POINT('Ctrl Pts',(6.06788130357792,5.08706353728799,29.8704535163693));
#65067=CARTESIAN_POINT('Ctrl Pts',(6.22925714558252,4.88179344435557,29.8599017273886));
#65068=CARTESIAN_POINT('Ctrl Pts',(6.25606745649414,4.84769072523719,29.8581486970729));
#65069=CARTESIAN_POINT('Ctrl Pts',(6.28258396788685,4.81334671390474,29.8563894548956));
#65070=CARTESIAN_POINT('Ctrl Pts',(6.30880152702889,4.77876355552774,29.8546236201992));
#65071=CARTESIAN_POINT('Ctrl Pts',(6.32705822238815,4.75468144385483,29.8533939746044));
#65072=CARTESIAN_POINT('Ctrl Pts',(6.34516995295352,4.73048336668523,29.852161132241));
#65073=CARTESIAN_POINT('Ctrl Pts',(6.36313657566678,4.70617129738668,29.8509249645731));
#65074=CARTESIAN_POINT('Ctrl Pts',(6.50761186100613,4.51067027278374,29.8409845500948));
#65075=CARTESIAN_POINT('Ctrl Pts',(6.6423066129919,4.30831997422948,29.8308633426248));
#65076=CARTESIAN_POINT('Ctrl Pts',(6.76708109523822,4.10009238934386,29.8206455720084));
#65077=CARTESIAN_POINT('Ctrl Pts',(6.89684698153664,3.8835349922062,29.8100190557835));
#65078=CARTESIAN_POINT('Ctrl Pts',(7.01588253952261,3.66061966769824,29.7992880961758));
#65079=CARTESIAN_POINT('Ctrl Pts',(7.12397765144178,3.43245841341115,29.7885474412361));
#65080=CARTESIAN_POINT('Ctrl Pts',(7.23329173525428,3.20172421987469,29.7776856655885));
#65081=CARTESIAN_POINT('Ctrl Pts',(7.33141638311738,2.96562429015909,29.7668139747105));
#65082=CARTESIAN_POINT('Ctrl Pts',(7.41809190885471,2.72534141341218,29.7560303583132));
#65083=CARTESIAN_POINT('Ctrl Pts',(7.50509960111561,2.48413770085651,29.7452054158744));
#65084=CARTESIAN_POINT('Ctrl Pts',(7.58056929512689,2.23871832786616,29.7344692242652));
#65085=CARTESIAN_POINT('Ctrl Pts',(7.64420956899104,1.99032320316301,29.7239209040971));
#65086=CARTESIAN_POINT('Ctrl Pts',(7.66729558128016,1.9002159086266,29.7200944175934));
#65087=CARTESIAN_POINT('Ctrl Pts',(7.68882471931851,1.80971747965483,29.7162926537119));
#65088=CARTESIAN_POINT('Ctrl Pts',(7.70878252342339,1.71888871380841,29.7125203441244));
#65089=CARTESIAN_POINT('Ctrl Pts',(7.75911040891409,1.48984449116967,29.7030076560574));
#65090=CARTESIAN_POINT('Ctrl Pts',(7.79971784227922,1.25872499840184,29.6935267004336));
#65091=CARTESIAN_POINT('Ctrl Pts',(7.83045312881348,1.026338145523,29.6841043965909));
#65092=CARTESIAN_POINT('Ctrl Pts',(7.86091227707832,0.796039150303125,29.6747667465443));
#65093=CARTESIAN_POINT('Ctrl Pts',(7.88167563920507,0.564494664909313,29.6654866991103));
#65094=CARTESIAN_POINT('Ctrl Pts',(7.8925465890629,0.33250349080512,29.6562904545633));
#65095=CARTESIAN_POINT('Ctrl Pts',(7.90327280642752,0.10360097606082,29.6472166459965));
#65096=CARTESIAN_POINT('Ctrl Pts',(7.90436801653756,-0.125737091559307,
29.6382244237192));
#65097=CARTESIAN_POINT('Ctrl Pts',(7.89559906329219,-0.354720295755568,
29.629338955409));
#65098=CARTESIAN_POINT('Ctrl Pts',(7.88705954372156,-0.57771231075014,29.6206859693107));
#65099=CARTESIAN_POINT('Ctrl Pts',(7.86916497631032,-0.800368274466062,
29.6121342239709));
#65100=CARTESIAN_POINT('Ctrl Pts',(7.84166199009046,-1.02192777059955,29.6037069628183));
#65101=CARTESIAN_POINT('Ctrl Pts',(7.81942455580808,-1.20106885351757,29.5968931330558));
#65102=CARTESIAN_POINT('Ctrl Pts',(7.79090490783725,-1.37949267680095,29.5901606844468));
#65103=CARTESIAN_POINT('Ctrl Pts',(7.75595211371944,-1.55677895632439,29.5835219031088));
#65104=CARTESIAN_POINT('Ctrl Pts',(7.70384921105463,-1.82105338699455,29.5736257049194));
#65105=CARTESIAN_POINT('Ctrl Pts',(7.63855814103414,-2.08232461837313,29.5633880391846));
#65106=CARTESIAN_POINT('Ctrl Pts',(7.55971905996207,-2.33919985628434,29.552885756511));
#65107=CARTESIAN_POINT('Ctrl Pts',(7.52069221803405,-2.46635797594862,29.5476869271968));
#65108=CARTESIAN_POINT('Ctrl Pts',(7.47834551663021,-2.59243806069412,29.5424232551434));
#65109=CARTESIAN_POINT('Ctrl Pts',(7.43263583996337,-2.71726648701272,29.5371040624316));
#65110=CARTESIAN_POINT('Ctrl Pts',(7.33891971869409,-2.97319557668874,29.5261984042521));
#65111=CARTESIAN_POINT('Ctrl Pts',(7.23106599937438,-3.22386638812884,29.5150593643078));
#65112=CARTESIAN_POINT('Ctrl Pts',(7.11010579502649,-3.46826954382605,29.5037672825078));
#65113=CARTESIAN_POINT('Ctrl Pts',(6.98844648158592,-3.71408526714707,29.492409936292));
#65114=CARTESIAN_POINT('Ctrl Pts',(6.85352793073787,-3.95356014371426,29.480897774048));
#65115=CARTESIAN_POINT('Ctrl Pts',(6.70642559643767,-4.18562160434378,29.4693125367638));
#65116=CARTESIAN_POINT('Ctrl Pts',(6.55852595528369,-4.41894085733898,29.4576645065327));
#65117=CARTESIAN_POINT('Ctrl Pts',(6.39830942902776,-4.64476540451055,29.4459426069692));
#65118=CARTESIAN_POINT('Ctrl Pts',(6.22690683037516,-4.86196855604495,29.4342299154074));
#65119=CARTESIAN_POINT('Ctrl Pts',(6.05573084914591,-5.07888453562902,29.4225327096085));
#65120=CARTESIAN_POINT('Ctrl Pts',(5.87339790505756,-5.28720100457781,29.410844687479));
#65121=CARTESIAN_POINT('Ctrl Pts',(5.68108025345432,-5.48577147790493,29.3992485972701));
#65122=CARTESIAN_POINT('Ctrl Pts',(5.49060621566564,-5.6824383960215,29.3877636706071));
#65123=CARTESIAN_POINT('Ctrl Pts',(5.29033779390495,-5.86954426748541,29.37636892174));
#65124=CARTESIAN_POINT('Ctrl Pts',(5.0814635797187,-6.04596572059475,29.3651447419124));
#65125=CARTESIAN_POINT('Ctrl Pts',(4.93417895129952,-6.17036675433466,29.3572301739909));
#65126=CARTESIAN_POINT('Ctrl Pts',(4.78261643501547,-6.28945508417574,29.3494004157432));
#65127=CARTESIAN_POINT('Ctrl Pts',(4.62720834647535,-6.4028382635155,29.3416836527204));
#65128=CARTESIAN_POINT('Ctrl Pts',(4.49779169203943,-6.49725852102785,29.3352574900742));
#65129=CARTESIAN_POINT('Ctrl Pts',(4.36561329795816,-6.58795204972318,29.328827803173));
#65130=CARTESIAN_POINT('Ctrl Pts',(4.23071911293456,-6.67459997598174,29.3224932309414));
#65131=CARTESIAN_POINT('Ctrl Pts',(4.17061489451043,-6.7132073176172,29.3196707629977));
#65132=CARTESIAN_POINT('Ctrl Pts',(4.10997185339344,-6.75101089244237,29.3168671780523));
#65133=CARTESIAN_POINT('Ctrl Pts',(4.04879584613982,-6.78797967381976,29.3140912014682));
#65134=CARTESIAN_POINT('Ctrl Pts',(3.85886069759447,-6.90275785725601,29.3054725362673));
#65135=CARTESIAN_POINT('Ctrl Pts',(3.66390030777603,-7.00972981581459,29.2969636370112));
#65136=CARTESIAN_POINT('Ctrl Pts',(3.46469529601492,-7.10828847885071,29.2885038963771));
#65137=CARTESIAN_POINT('Ctrl Pts',(3.26624601390199,-7.20647323711867,29.2800762496986));
#65138=CARTESIAN_POINT('Ctrl Pts',(3.06358500976317,-7.29630844349399,29.2716973893607));
#65139=CARTESIAN_POINT('Ctrl Pts',(2.85748136980523,-7.377245344131,29.2633073952103));
#65140=CARTESIAN_POINT('Ctrl Pts',(2.65321619915542,-7.45746027785976,29.2549922408188));
#65141=CARTESIAN_POINT('Ctrl Pts',(2.44557017836928,-7.52893509243917,29.2466661503588));
#65142=CARTESIAN_POINT('Ctrl Pts',(2.23527897503751,-7.59118481739772,29.2382707929012));
#65143=CARTESIAN_POINT('Ctrl Pts',(2.07251993239705,-7.63936422518255,29.2317730396867));
#65144=CARTESIAN_POINT('Ctrl Pts',(1.90817615877255,-7.68201854366409,29.2252337935135));
#65145=CARTESIAN_POINT('Ctrl Pts',(1.74257982759338,-7.71894247785003,29.2186260103798));
#65146=CARTESIAN_POINT('Ctrl Pts',(1.52726421289925,-7.76695259697258,29.2100342808586));
#65147=CARTESIAN_POINT('Ctrl Pts',(1.30983244520213,-7.80527365789384,29.2013266804133));
#65148=CARTESIAN_POINT('Ctrl Pts',(1.09115861770332,-7.83424991552118,29.192443759928));
#65149=CARTESIAN_POINT('Ctrl Pts',(0.872125635103007,-7.86327376444405,
29.1835462499225));
#65150=CARTESIAN_POINT('Ctrl Pts',(0.651847066314613,-7.88292277445575,
29.1744728435044));
#65151=CARTESIAN_POINT('Ctrl Pts',(0.4311625345861,-7.89357782348103,29.1651637981544));
#65152=CARTESIAN_POINT('Ctrl Pts',(0.211743315076415,-7.90417178093991,
29.1559081269524));
#65153=CARTESIAN_POINT('Ctrl Pts',(-0.00807683931881509,-7.90587528930512,
29.146419511181));
#65154=CARTESIAN_POINT('Ctrl Pts',(-0.227517940637586,-7.89908699077107,
29.1366392300558));
#65155=CARTESIAN_POINT('Ctrl Pts',(-0.268085759595382,-7.89783204598495,
29.1348311609582));
#65156=CARTESIAN_POINT('Ctrl Pts',(-0.308640757788562,-7.89628693235663,
29.1330131237645));
#65157=CARTESIAN_POINT('Ctrl Pts',(-0.34917819275588,-7.89445423238116,
29.1311847474671));
#65158=CARTESIAN_POINT('Ctrl Pts',(-0.538828059795782,-7.88588015000639,
29.1226308929378));
#65159=CARTESIAN_POINT('Ctrl Pts',(-0.728031810797408,-7.87015139420761,
29.1143509327306));
#65160=CARTESIAN_POINT('Ctrl Pts',(-0.916358502593095,-7.84757804624816,
29.1062655195673));
#65161=CARTESIAN_POINT('Ctrl Pts',(-1.10611378864828,-7.8248334631069,29.0981187726934));
#65162=CARTESIAN_POINT('Ctrl Pts',(-1.29497906805076,-7.79514041704204,
29.0901695356186));
#65163=CARTESIAN_POINT('Ctrl Pts',(-1.48255483525554,-7.75878252323287,
29.082336641613));
#65164=CARTESIAN_POINT('Ctrl Pts',(-1.67162478348115,-7.72213501165647,
29.074441352759));
#65165=CARTESIAN_POINT('Ctrl Pts',(-1.85938507411905,-7.67871641847901,
29.0666642678754));
#65166=CARTESIAN_POINT('Ctrl Pts',(-2.04546167796984,-7.62877763964518,
29.0589222650794));
#65167=CARTESIAN_POINT('Ctrl Pts',(-2.13475364070083,-7.60481368347776,
29.0552071358756));
#65168=CARTESIAN_POINT('Ctrl Pts',(-2.22365836859117,-7.57934769442297,
29.0515000850955));
#65169=CARTESIAN_POINT('Ctrl Pts',(-2.31213684239565,-7.55240382264388,
29.0477919277812));
#65170=CARTESIAN_POINT('Ctrl Pts',(-2.52253784614527,-7.48833154129159,
29.0389739635077));
#65171=CARTESIAN_POINT('Ctrl Pts',(-2.7306355300909,-7.41541124061954,29.0303909052055));
#65172=CARTESIAN_POINT('Ctrl Pts',(-2.93552934277737,-7.33397728379057,
29.0219582481968));
#65173=CARTESIAN_POINT('Ctrl Pts',(-3.14073584780823,-7.25241904905129,
29.0135127219499));
#65174=CARTESIAN_POINT('Ctrl Pts',(-3.34272841978637,-7.16232190482128,
29.0052180564073));
#65175=CARTESIAN_POINT('Ctrl Pts',(-3.54065085396848,-7.0640410666409,28.9969893594079));
#65176=CARTESIAN_POINT('Ctrl Pts',(-3.73824838897254,-6.9659215611749,28.9887741702097));
#65177=CARTESIAN_POINT('Ctrl Pts',(-3.93178901997251,-6.85964594418846,
28.9806247331514));
#65178=CARTESIAN_POINT('Ctrl Pts',(-4.12047194257944,-6.74557574391328,
28.9724565734496));
#65179=CARTESIAN_POINT('Ctrl Pts',(-4.30869741496518,-6.63178209987131,
28.9643082169521));
#65180=CARTESIAN_POINT('Ctrl Pts',(-4.49208872615072,-6.51023231954899,
28.9561412284849));
#65181=CARTESIAN_POINT('Ctrl Pts',(-4.66990257513552,-6.38128259761895,
28.947871746188));
#65182=CARTESIAN_POINT('Ctrl Pts',(-4.84722625193836,-6.25268834612568,
28.9396250600356));
#65183=CARTESIAN_POINT('Ctrl Pts',(-5.01900332658137,-6.11673554487985,
28.9312764443558));
#65184=CARTESIAN_POINT('Ctrl Pts',(-5.18454679116245,-5.97376467352253,
28.9227427289143));
#65185=CARTESIAN_POINT('Ctrl Pts',(-5.30722346042526,-5.86781551784852,
28.9164187837833));
#65186=CARTESIAN_POINT('Ctrl Pts',(-5.42647794164635,-5.75801208869698,
28.9099931890388));
#65187=CARTESIAN_POINT('Ctrl Pts',(-5.54204749344127,-5.64448530799503,
28.9034320978716));
#65188=CARTESIAN_POINT('Ctrl Pts',(-5.7020121852652,-5.4873481018131,28.8943506148142));
#65189=CARTESIAN_POINT('Ctrl Pts',(-5.85491566406144,-5.3230794649538,28.8850095409915));
#65190=CARTESIAN_POINT('Ctrl Pts',(-6.00067576598747,-5.15259419213927,
28.8753191211564));
#65191=CARTESIAN_POINT('Ctrl Pts',(-6.14643586791348,-4.98210891932477,
28.8656287013213));
#65192=CARTESIAN_POINT('Ctrl Pts',(-6.28505318089336,-4.80540767793714,
28.8555889354738));
#65193=CARTESIAN_POINT('Ctrl Pts',(-6.41648389579647,-4.62336032226345,
28.8451100683667));
#65194=CARTESIAN_POINT('Ctrl Pts',(-6.53962515289976,-4.45279486314295,
28.8352921131838));
#65195=CARTESIAN_POINT('Ctrl Pts',(-6.65528280494462,-4.27697500599435,
28.8258401557342));
#65196=CARTESIAN_POINT('Ctrl Pts',(-6.7633938673275,-4.09665303851573,28.8166951548517));
#65197=CARTESIAN_POINT('Ctrl Pts',(-6.87365135597915,-3.91275097664805,
28.8073685900322));
#65198=CARTESIAN_POINT('Ctrl Pts',(-6.97606016824697,-3.72416611941421,
28.7983612913453));
#65199=CARTESIAN_POINT('Ctrl Pts',(-7.07054837617649,-3.53164260475705,
28.7896106307524));
#65200=CARTESIAN_POINT('Ctrl Pts',(-7.09892101577191,-3.47383221323089,
28.7869830082726));
#65201=CARTESIAN_POINT('Ctrl Pts',(-7.12657941808578,-3.41566633441897,
28.7843785259008));
#65202=CARTESIAN_POINT('Ctrl Pts',(-7.15352143167685,-3.3571642301761,28.7817954879908));
#65203=CARTESIAN_POINT('Ctrl Pts',(-7.25230039082061,-3.14267480661102,
28.7723251566322));
#65204=CARTESIAN_POINT('Ctrl Pts',(-7.3418497446533,-2.92397966063852,28.762864035899));
#65205=CARTESIAN_POINT('Ctrl Pts',(-7.42196251902932,-2.70188901454886,
28.7534152726674));
#65206=CARTESIAN_POINT('Ctrl Pts',(-7.5024061150049,-2.47888125650843,28.7439274912519));
#65207=CARTESIAN_POINT('Ctrl Pts',(-7.57333523304903,-2.25244906459848,
28.734452169608));
#65208=CARTESIAN_POINT('Ctrl Pts',(-7.63449089954376,-2.02339652599593,
28.7249924937579));
#65209=CARTESIAN_POINT('Ctrl Pts',(-7.69505982794055,-1.79654155727583,
28.7156235756826));
#65210=CARTESIAN_POINT('Ctrl Pts',(-7.74604202587532,-1.56711546990253,
28.7062700046243));
#65211=CARTESIAN_POINT('Ctrl Pts',(-7.78713558864553,-1.33589585848278,
28.6969348757802));
#65212=CARTESIAN_POINT('Ctrl Pts',(-7.8270789797213,-1.11114787508277,28.6878610287582));
#65213=CARTESIAN_POINT('Ctrl Pts',(-7.85767946192405,-0.884704685624519,
28.678804606036));
#65214=CARTESIAN_POINT('Ctrl Pts',(-7.87861219250326,-0.657287840938538,
28.6697684501219));
#65215=CARTESIAN_POINT('Ctrl Pts',(-7.89871791238911,-0.438855785011747,
28.661089294817));
#65216=CARTESIAN_POINT('Ctrl Pts',(-7.90990453771594,-0.219525002565944,
28.6524288365514));
#65217=CARTESIAN_POINT('Ctrl Pts',(-7.91184153648199,4.99451412436924E-5,
28.6437895940631));
#65218=CARTESIAN_POINT('',(-7.91808516897138,-0.00159779970073705,26.6422647402301));
#65219=CARTESIAN_POINT('Ctrl Pts',(-7.911,-5.4678483962789E-13,28.642331508237));
#65220=CARTESIAN_POINT('Ctrl Pts',(-7.91100000000015,2.20167589666618,28.5537440725043));
#65221=CARTESIAN_POINT('Ctrl Pts',(-6.94214576672406,4.38610418338626,28.4651566367716));
#65222=CARTESIAN_POINT('Ctrl Pts',(-3.67820201488353,7.34180684107597,28.2879817653062));
#65223=CARTESIAN_POINT('Ctrl Pts',(-1.40868175871823,8.08992666571321,28.1993943295734));
#65224=CARTESIAN_POINT('Ctrl Pts',(2.9730927052119,7.65454228025288,28.022219458108));
#65225=CARTESIAN_POINT('Ctrl Pts',(5.05102072675527,6.47444880834283,27.9336320223753));
#65226=CARTESIAN_POINT('Ctrl Pts',(7.66951518847833,2.93425195367804,27.7564571509098));
#65227=CARTESIAN_POINT('Ctrl Pts',(8.18956872247062,0.601881960100259,27.6678697151771));
#65228=CARTESIAN_POINT('Ctrl Pts',(7.32306689761395,-3.71537198232343,27.4906948437116));
#65229=CARTESIAN_POINT('Ctrl Pts',(5.94329958850286,-5.6664351893642,27.4021074079789));
#65230=CARTESIAN_POINT('Ctrl Pts',(2.16154501637976,-7.92205913232961,27.2249325365135));
#65231=CARTESIAN_POINT('Ctrl Pts',(-0.210816529298981,-8.20894963713005,
27.1363451007807));
#65232=CARTESIAN_POINT('Ctrl Pts',(-4.42123908576312,-6.9198224471791,26.9591702293153));
#65233=CARTESIAN_POINT('Ctrl Pts',(-6.22631625634087,-5.35390358803636,
26.8705827935826));
#65234=CARTESIAN_POINT('Ctrl Pts',(-7.6529404869374,-2.3138436401746,26.7354627452239));
#65235=CARTESIAN_POINT('Ctrl Pts',(-7.9107562251631,-1.15812141717204,26.6889301325979));
#65236=CARTESIAN_POINT('Ctrl Pts',(-7.9109998272103,-0.00164059837198713,
26.642397519972));
#65237=CARTESIAN_POINT('',(-7.90279014835528,-0.00473842408097357,24.6423332821822));
#65238=CARTESIAN_POINT('Ctrl Pts',(-7.92184818564761,-0.00157506937677171,
26.6421942210654));
#65239=CARTESIAN_POINT('Ctrl Pts',(-7.90527866078965,2.38817114548611,26.5457221946099));
#65240=CARTESIAN_POINT('Ctrl Pts',(-5.47644787019391,7.43173693689856,26.3433157883521));
#65241=CARTESIAN_POINT('Ctrl Pts',(1.61672921772412,8.57512333172727,26.0879421921928));
#65242=CARTESIAN_POINT('Ctrl Pts',(6.10409558131502,5.51035650884788,25.8760734325877));
#65243=CARTESIAN_POINT('Ctrl Pts',(8.69528679823428,0.733853537314583,25.6642046729827));
#65244=CARTESIAN_POINT('Ctrl Pts',(6.76558824356892,-6.46288284829038,25.3993687234762));
#65245=CARTESIAN_POINT('Ctrl Pts',(-1.77924551132568,-9.18489542958251,
25.0815655840685));
#65246=CARTESIAN_POINT('Ctrl Pts',(-7.25618309704257,-4.65554030243547,
24.8292205841656));
#65247=CARTESIAN_POINT('Ctrl Pts',(-7.90576535995413,-1.01347673874075,
24.6828099640653));
#65248=CARTESIAN_POINT('Ctrl Pts',(-7.90074683040818,-0.00474821529727623,
24.6423337237675));
#65249=CARTESIAN_POINT('',(-7.90432432633472,0.00627944674389112,22.6423294472501));
#65250=CARTESIAN_POINT('Ctrl Pts',(-7.91099860438285,-0.00469909061914475,
24.642331508237));
#65251=CARTESIAN_POINT('Ctrl Pts',(-7.91111988382393,0.199476901486499,
24.6341493331127));
#65252=CARTESIAN_POINT('Ctrl Pts',(-7.90333194721171,0.403663036123113,
24.6259671579884));
#65253=CARTESIAN_POINT('Ctrl Pts',(-7.88766198850874,0.60721442261722,24.617784982864));
#65254=CARTESIAN_POINT('Ctrl Pts',(-7.87238375930625,0.805677277324782,
24.6098073519529));
#65255=CARTESIAN_POINT('Ctrl Pts',(-7.84961292323444,1.00353639927101,24.6018297210419));
#65256=CARTESIAN_POINT('Ctrl Pts',(-7.81942730419529,1.20019899783543,24.5938520901308));
#65257=CARTESIAN_POINT('Ctrl Pts',(-7.78923239663649,1.39692211211797,24.5858720043957));
#65258=CARTESIAN_POINT('Ctrl Pts',(-7.75161820732367,1.592447639378,24.5778919186606));
#65259=CARTESIAN_POINT('Ctrl Pts',(-7.70671387622014,1.78619210335169,24.5699118329255));
#65260=CARTESIAN_POINT('Ctrl Pts',(-7.66178892353793,1.98002554129762,24.5619280824668));
#65261=CARTESIAN_POINT('Ctrl Pts',(-7.6095672292207,2.17207596064996,24.553944332008));
#65262=CARTESIAN_POINT('Ctrl Pts',(-7.55022817545046,2.36177380344395,24.5459605815493));
#65263=CARTESIAN_POINT('Ctrl Pts',(-7.48829006397143,2.55978043462141,24.5376271418579));
#65264=CARTESIAN_POINT('Ctrl Pts',(-7.41859721950583,2.75522337689826,24.5292937021666));
#65265=CARTESIAN_POINT('Ctrl Pts',(-7.34140975810823,2.94747752553829,24.5209602624752));
#65266=CARTESIAN_POINT('Ctrl Pts',(-7.26731873141991,3.13201925031989,24.5129611251621));
#65267=CARTESIAN_POINT('Ctrl Pts',(-7.18632283809609,3.31362275397686,24.5049619878489));
#65268=CARTESIAN_POINT('Ctrl Pts',(-7.09869945867559,3.49175987080997,24.4969628505357));
#65269=CARTESIAN_POINT('Ctrl Pts',(-7.01100849759306,3.67003438022603,24.4889575436933));
#65270=CARTESIAN_POINT('Ctrl Pts',(-6.91668001319148,3.84483687849186,24.4809522368509));
#65271=CARTESIAN_POINT('Ctrl Pts',(-6.81603576199685,4.01566650646939,24.4729469300086));
#65272=CARTESIAN_POINT('Ctrl Pts',(-6.71525529087635,4.18672734883804,24.4649307881479));
#65273=CARTESIAN_POINT('Ctrl Pts',(-6.60814215854351,4.3538043018684,24.4569146462873));
#65274=CARTESIAN_POINT('Ctrl Pts',(-6.49506023788673,4.51642707305485,24.4488985044266));
#65275=CARTESIAN_POINT('Ctrl Pts',(-6.48123936272855,4.53630283219823,24.4479187713688));
#65276=CARTESIAN_POINT('Ctrl Pts',(-6.46732937497621,4.55611209863451,24.446939038311));
#65277=CARTESIAN_POINT('Ctrl Pts',(-6.45333097816966,4.5758540499229,24.4459593052532));
#65278=CARTESIAN_POINT('Ctrl Pts',(-6.34130840660208,4.7338395808127,24.438118963384));
#65279=CARTESIAN_POINT('Ctrl Pts',(-6.22331232814448,4.88794656333586,24.4302786215148));
#65280=CARTESIAN_POINT('Ctrl Pts',(-6.09964126902208,5.03768770263131,24.4224382796456));
#65281=CARTESIAN_POINT('Ctrl Pts',(-5.97610847782461,5.18726142687627,24.414606703512));
#65282=CARTESIAN_POINT('Ctrl Pts',(-5.84691356140695,5.33247875908419,24.4067751273783));
#65283=CARTESIAN_POINT('Ctrl Pts',(-5.71239872668933,5.47288057491831,24.3989435512447));
#65284=CARTESIAN_POINT('Ctrl Pts',(-5.57800812805659,5.61315271753127,24.391119208249));
#65285=CARTESIAN_POINT('Ctrl Pts',(-5.43830763749175,5.74861794886992,24.3832948652533));
#65286=CARTESIAN_POINT('Ctrl Pts',(-5.29368031332814,5.87884935512742,24.3754705222576));
#65287=CARTESIAN_POINT('Ctrl Pts',(-5.14915845798907,6.00898579071866,24.3676518851288));
#65288=CARTESIAN_POINT('Ctrl Pts',(-4.99971718517095,6.13389576897055,24.359833248));
#65289=CARTESIAN_POINT('Ctrl Pts',(-4.84577719711519,6.25318833523495,24.3520146108712));
#65290=CARTESIAN_POINT('Ctrl Pts',(-4.69191956297701,6.37241708305754,24.3442001565113));
#65291=CARTESIAN_POINT('Ctrl Pts',(-4.5335682850339,6.48603419050078,24.3363857021514));
#65292=CARTESIAN_POINT('Ctrl Pts',(-4.3711781539614,6.59368808379124,24.3285712477916));
#65293=CARTESIAN_POINT('Ctrl Pts',(-4.20884335727195,6.70130529405344,24.3207594562044));
#65294=CARTESIAN_POINT('Ctrl Pts',(-4.04247274225547,6.80296314473486,24.3129476646172));
#65295=CARTESIAN_POINT('Ctrl Pts',(-3.87255131813304,6.89835250537591,24.3051358730301));
#65296=CARTESIAN_POINT('Ctrl Pts',(-3.70262194141433,6.99374633039264,24.2973237158385));
#65297=CARTESIAN_POINT('Ctrl Pts',(-3.5291417257168,7.08287089914626,24.2895115586469));
#65298=CARTESIAN_POINT('Ctrl Pts',(-3.35262204987139,7.16546205005066,24.2816994014553));
#65299=CARTESIAN_POINT('Ctrl Pts',(-3.17608794338219,7.24805995285664,24.2738866056127));
#65300=CARTESIAN_POINT('Ctrl Pts',(-2.99651420014128,7.32412322397701,24.2660738097702));
#65301=CARTESIAN_POINT('Ctrl Pts',(-2.81443395397274,7.39343509599735,24.2582610139277));
#65302=CARTESIAN_POINT('Ctrl Pts',(-2.6323067839967,7.46276483034493,24.2504462046535));
#65303=CARTESIAN_POINT('Ctrl Pts',(-2.44767215300058,7.52533957430112,24.2426313953793));
#65304=CARTESIAN_POINT('Ctrl Pts',(-2.26108033499531,7.58099180310186,24.2348165861052));
#65305=CARTESIAN_POINT('Ctrl Pts',(-2.07440759527138,7.63666816733388,24.2269983876803));
#65306=CARTESIAN_POINT('Ctrl Pts',(-1.88577631439626,7.68541593548877,24.2191801892554));
#65307=CARTESIAN_POINT('Ctrl Pts',(-1.69574913354654,7.72711821289646,24.2113619908304));
#65308=CARTESIAN_POINT('Ctrl Pts',(-1.50550076208681,7.76886903152934,24.2035346920649));
#65309=CARTESIAN_POINT('Ctrl Pts',(-1.31385358901552,7.80355790455573,24.1957073932993));
#65310=CARTESIAN_POINT('Ctrl Pts',(-1.12137868713031,7.83111938614461,24.1878800945338));
#65311=CARTESIAN_POINT('Ctrl Pts',(-0.92877813684542,7.8586988599809,24.1800476860757));
#65312=CARTESIAN_POINT('Ctrl Pts',(-0.73534912940628,7.87914163335445,24.1722152776176));
#65313=CARTESIAN_POINT('Ctrl Pts',(-0.541665045788452,7.8924343505772,24.1643828691595));
#65314=CARTESIAN_POINT('Ctrl Pts',(-0.347702998217335,7.90574614472233,
24.1565392200916));
#65315=CARTESIAN_POINT('Ctrl Pts',(-0.15348549339493,7.91188737686632,24.1486955710237));
#65316=CARTESIAN_POINT('Ctrl Pts',(0.040415717483983,7.91089676141588,24.1408519219558));
#65317=CARTESIAN_POINT('Ctrl Pts',(0.1450320961399,7.91036229027671,24.1366200032524));
#65318=CARTESIAN_POINT('Ctrl Pts',(0.249556504707496,7.90775265085662,24.1323880845489));
#65319=CARTESIAN_POINT('Ctrl Pts',(0.353900185828802,7.90308013741923,24.1281561658455));
#65320=CARTESIAN_POINT('Ctrl Pts',(0.549123101975789,7.89433804887892,24.1202384126927));
#65321=CARTESIAN_POINT('Ctrl Pts',(0.744296330346685,7.87834574622237,24.1123206595398));
#65322=CARTESIAN_POINT('Ctrl Pts',(0.938839588114405,7.85509396683383,24.104402906387));
#65323=CARTESIAN_POINT('Ctrl Pts',(1.13315932967706,7.83186890206675,24.0964942501628));
#65324=CARTESIAN_POINT('Ctrl Pts',(1.32685020368346,7.80140101411378,24.0885855939386));
#65325=CARTESIAN_POINT('Ctrl Pts',(1.51933232660837,7.76373301198095,24.0806769377144));
#65326=CARTESIAN_POINT('Ctrl Pts',(1.71162893255038,7.72610131479947,24.0727759039646));
#65327=CARTESIAN_POINT('Ctrl Pts',(1.90271877253867,7.68128339320356,24.0648748702147));
#65328=CARTESIAN_POINT('Ctrl Pts',(2.09202719526749,7.62937371048642,24.0569738364649));
#65329=CARTESIAN_POINT('Ctrl Pts',(2.28118819123502,7.57750445320989,24.049078955763));
#65330=CARTESIAN_POINT('Ctrl Pts',(2.46857020327513,7.51855452867736,24.0411840750612));
#65331=CARTESIAN_POINT('Ctrl Pts',(2.65360860351722,7.45266948008158,24.0332891943594));
#65332=CARTESIAN_POINT('Ctrl Pts',(2.83853713485194,7.38682355157272,24.0253990013435));
#65333=CARTESIAN_POINT('Ctrl Pts',(3.02112450363762,7.31405081939341,24.0175088083277));
#65334=CARTESIAN_POINT('Ctrl Pts',(3.2008208115859,7.23454678138987,24.0096186153118));
#65335=CARTESIAN_POINT('Ctrl Pts',(3.38044366061104,7.15507524422669,24.0017316477662));
#65336=CARTESIAN_POINT('Ctrl Pts',(3.55717748969029,7.06887802450121,23.9938446802205));
#65337=CARTESIAN_POINT('Ctrl Pts',(3.73049170866777,6.9761990088845,23.9859577126748));
#65338=CARTESIAN_POINT('Ctrl Pts',(3.90379087648731,6.88352804180823,23.9780714300585));
#65339=CARTESIAN_POINT('Ctrl Pts',(4.07367071921496,6.78437655700258,23.9701851474422));
#65340=CARTESIAN_POINT('Ctrl Pts',(4.23962415783559,6.67903496025413,23.9622988648259));
#65341=CARTESIAN_POINT('Ctrl Pts',(4.40557730476928,6.57369354865862,23.9544125960708));
#65342=CARTESIAN_POINT('Ctrl Pts',(4.56760377012997,6.46216223100105,23.9465263273158));
#65343=CARTESIAN_POINT('Ctrl Pts',(4.72522435664793,6.34477547115271,23.9386400585607));
#65344=CARTESIAN_POINT('Ctrl Pts',(4.88287108415609,6.2273692429963,23.9307524818872));
#65345=CARTESIAN_POINT('Ctrl Pts',(5.03611020051353,6.10410584347305,23.9228649052137));
#65346=CARTESIAN_POINT('Ctrl Pts',(5.18449437880163,5.97536099630594,23.9149773285402));
#65347=CARTESIAN_POINT('Ctrl Pts',(5.33292803630578,5.84657321872548,23.9070871217271));
#65348=CARTESIAN_POINT('Ctrl Pts',(5.47650327003698,5.7123005772867,23.8991969149139));
#65349=CARTESIAN_POINT('Ctrl Pts',(5.61480832495223,5.57295688786906,23.8913067081008));
#65350=CARTESIAN_POINT('Ctrl Pts',(5.75324693570809,5.43347863964165,23.8834088820202));
#65351=CARTESIAN_POINT('Ctrl Pts',(5.88640495959489,5.28891980691886,23.8755110559396));
#65352=CARTESIAN_POINT('Ctrl Pts',(6.0139090833572,5.13972942255852,23.867613229859));
#65353=CARTESIAN_POINT('Ctrl Pts',(6.14148380856284,4.99045642866246,23.8597110306028));
#65354=CARTESIAN_POINT('Ctrl Pts',(6.26339817817814,4.83654703931126,23.8518088313466));
#65355=CARTESIAN_POINT('Ctrl Pts',(6.37932104863958,4.67848094560446,23.8439066320904));
#65356=CARTESIAN_POINT('Ctrl Pts',(6.49538384679467,4.52022405413836,23.8359948942806));
#65357=CARTESIAN_POINT('Ctrl Pts',(6.60544050707392,4.35780072065255,23.8280831564708));
#65358=CARTESIAN_POINT('Ctrl Pts',(6.70920426454532,4.19171792187963,23.820171418661));
#65359=CARTESIAN_POINT('Ctrl Pts',(6.75212754696815,4.12301552471299,23.8168986212532));
#65360=CARTESIAN_POINT('Ctrl Pts',(6.79397455576169,4.05368720450044,23.8136258238455));
#65361=CARTESIAN_POINT('Ctrl Pts',(6.83472736305399,3.98376993220254,23.8103530264378));
#65362=CARTESIAN_POINT('Ctrl Pts',(6.93826378547244,3.80613838434233,23.8020381701762));
#65363=CARTESIAN_POINT('Ctrl Pts',(7.03496030254178,3.6243162306715,23.7937233139146));
#65364=CARTESIAN_POINT('Ctrl Pts',(7.12448314941557,3.43884586070582,23.7854084576529));
#65365=CARTESIAN_POINT('Ctrl Pts',(7.21389575201512,3.25360389105408,23.7771038408477));
#65366=CARTESIAN_POINT('Ctrl Pts',(7.2961521767793,3.06472292830131,23.7687992240426));
#65367=CARTESIAN_POINT('Ctrl Pts',(7.37096373096742,2.87277125381797,23.7604946072374));
#65368=CARTESIAN_POINT('Ctrl Pts',(7.44568809197913,2.68104329980665,23.7521996694975));
#65369=CARTESIAN_POINT('Ctrl Pts',(7.51298478295705,2.48625204459096,23.7439047317576));
#65370=CARTESIAN_POINT('Ctrl Pts',(7.57261219626893,2.28898788221323,23.7356097940178));
#65371=CARTESIAN_POINT('Ctrl Pts',(7.63215023917516,2.09201938213637,23.7273272888472));
#65372=CARTESIAN_POINT('Ctrl Pts',(7.68404185948036,1.89258565149747,23.7190447836767));
#65373=CARTESIAN_POINT('Ctrl Pts',(7.72809444914455,1.69129452937721,23.7107622785062));
#65374=CARTESIAN_POINT('Ctrl Pts',(7.7721065702309,1.49018832182164,23.7024873819963));
#65375=CARTESIAN_POINT('Ctrl Pts',(7.8082939586741,1.28722841083785,23.6942124854864));
#65376=CARTESIAN_POINT('Ctrl Pts',(7.83651401943129,1.08303694454844,23.6859375889765));
#65377=CARTESIAN_POINT('Ctrl Pts',(7.86470180014006,0.879079046516573,23.677672157863));
#65378=CARTESIAN_POINT('Ctrl Pts',(7.884940398717,0.673892694018034,23.6694067267494));
#65379=CARTESIAN_POINT('Ctrl Pts',(7.89713836537564,0.468109643259195,23.6611412956359));
#65380=CARTESIAN_POINT('Ctrl Pts',(7.90190505893862,0.387694212485036,23.6579113493353));
#65381=CARTESIAN_POINT('Ctrl Pts',(7.90544444214007,0.307187765194219,23.6546814030347));
#65382=CARTESIAN_POINT('Ctrl Pts',(7.9077531950713,0.226628342975039,23.651451456734));
#65383=CARTESIAN_POINT('Ctrl Pts',(7.91366210694694,0.0204484091214447,
23.6431848865891));
#65384=CARTESIAN_POINT('Ctrl Pts',(7.91149972666629,-0.185846420877929,
23.6349183164441));
#65385=CARTESIAN_POINT('Ctrl Pts',(7.90130094414447,-0.391617658005469,
23.6266517462991));
#65386=CARTESIAN_POINT('Ctrl Pts',(7.89109302339534,-0.597573268545718,
23.6183777692115));
#65387=CARTESIAN_POINT('Ctrl Pts',(7.8728343396224,-0.803004056335675,23.6101037921239));
#65388=CARTESIAN_POINT('Ctrl Pts',(7.84661163214932,-1.00727696996359,23.6018298150363));
#65389=CARTESIAN_POINT('Ctrl Pts',(7.82036372674066,-1.21174617360933,23.593547887315));
#65390=CARTESIAN_POINT('Ctrl Pts',(7.78613655671095,-1.41505499083991,23.5852659595937));
#65391=CARTESIAN_POINT('Ctrl Pts',(7.74406804962572,-1.61658004527027,23.5769840318724));
#65392=CARTESIAN_POINT('Ctrl Pts',(7.70192980903953,-1.81843915119313,23.5686883758813));
#65393=CARTESIAN_POINT('Ctrl Pts',(7.6519243053614,-2.01850829498922,23.5603927198903));
#65394=CARTESIAN_POINT('Ctrl Pts',(7.59424001638265,-2.21617679203903,23.5520970638992));
#65395=CARTESIAN_POINT('Ctrl Pts',(7.53650359197021,-2.41402394315571,23.5437939102405));
#65396=CARTESIAN_POINT('Ctrl Pts',(7.47107461759645,-2.60946583698416,23.5354907565819));
#65397=CARTESIAN_POINT('Ctrl Pts',(7.39819038259295,-2.80191007402257,23.5271876029232));
#65398=CARTESIAN_POINT('Ctrl Pts',(7.32519502560454,-2.99464771862167,23.5188717899711));
#65399=CARTESIAN_POINT('Ctrl Pts',(7.24472179802206,-3.18437829881425,23.5105559770191));
#65400=CARTESIAN_POINT('Ctrl Pts',(7.15705553730343,-3.37053067571774,23.502240164067));
#65401=CARTESIAN_POINT('Ctrl Pts',(7.12300353068101,-3.44283742085703,23.4990100717214));
#65402=CARTESIAN_POINT('Ctrl Pts',(7.08786675124449,-3.51460457707592,23.4957799793758));
#65403=CARTESIAN_POINT('Ctrl Pts',(7.05166370350665,-3.58579977308366,23.4925498870302));
#65404=CARTESIAN_POINT('Ctrl Pts',(6.96299717529939,-3.76016716062393,23.484638921187));
#65405=CARTESIAN_POINT('Ctrl Pts',(6.86774749850498,-3.93146395442826,23.4767279553439));
#65406=CARTESIAN_POINT('Ctrl Pts',(6.76615185853524,-4.0991596733038,23.4688169895007));
#65407=CARTESIAN_POINT('Ctrl Pts',(6.66465902396409,-4.26668569960961,23.4609140288238));
#65408=CARTESIAN_POINT('Ctrl Pts',(6.55683319458905,-4.43061761729703,23.453011068147));
#65409=CARTESIAN_POINT('Ctrl Pts',(6.44295846077933,-4.59044739351973,23.4451081074701));
#65410=CARTESIAN_POINT('Ctrl Pts',(6.3291778838376,-4.7501450151315,23.4372116813247));
#65411=CARTESIAN_POINT('Ctrl Pts',(6.20935856514258,-4.90574697343133,23.4293152551793));
#65412=CARTESIAN_POINT('Ctrl Pts',(6.08382924630566,-5.05677196458333,23.4214188290338));
#65413=CARTESIAN_POINT('Ctrl Pts',(5.95838049654882,-5.20770002264655,23.4135274710892));
#65414=CARTESIAN_POINT('Ctrl Pts',(5.82722926808575,-5.35405670266394,23.4056361131445));
#65415=CARTESIAN_POINT('Ctrl Pts',(5.69074630437131,-5.4953914782556,23.3977447551998));
#65416=CARTESIAN_POINT('Ctrl Pts',(5.5543256942733,-5.63666168363172,23.3898570025015));
#65417=CARTESIAN_POINT('Ctrl Pts',(5.4125784417489,-5.7729143092266,23.3819692498032));
#65418=CARTESIAN_POINT('Ctrl Pts',(5.2659142710303,-5.90373338576188,23.3740814971049));
#65419=CARTESIAN_POINT('Ctrl Pts',(5.11928998009721,-6.03451689098696,23.3661958891832));
#65420=CARTESIAN_POINT('Ctrl Pts',(4.96775169261106,-6.15986956290902,23.3583102812615));
#65421=CARTESIAN_POINT('Ctrl Pts',(4.81174474820048,-6.2794134660942,23.3504246733398));
#65422=CARTESIAN_POINT('Ctrl Pts',(4.65571940412607,-6.39897146844424,23.3425381353792));
#65423=CARTESIAN_POINT('Ctrl Pts',(4.49522461937134,-6.51271911820504,23.3346515974186));
#65424=CARTESIAN_POINT('Ctrl Pts',(4.33073796624141,-6.62031945360307,23.3267650594579));
#65425=CARTESIAN_POINT('Ctrl Pts',(4.16623059090162,-6.72793334460995,23.3188775279425));
#65426=CARTESIAN_POINT('Ctrl Pts',(3.99773063316515,-6.82939818878412,23.3109899964272));
#65427=CARTESIAN_POINT('Ctrl Pts',(3.82574370650676,-6.92442099327618,23.3031024649118));
#65428=CARTESIAN_POINT('Ctrl Pts',(3.65370628574886,-7.0194716957663,23.295212617675));
#65429=CARTESIAN_POINT('Ctrl Pts',(3.47818015752651,-7.10807642291331,23.2873227704383));
#65430=CARTESIAN_POINT('Ctrl Pts',(3.29969474408242,-7.18998856715884,23.2794329232015));
#65431=CARTESIAN_POINT('Ctrl Pts',(3.12112701174214,-7.27193848993859,23.2715394371043));
#65432=CARTESIAN_POINT('Ctrl Pts',(2.93959758720813,-7.34718953530905,23.2636459510071));
#65433=CARTESIAN_POINT('Ctrl Pts',(2.75565525731032,-7.41554347993847,23.2557524649098));
#65434=CARTESIAN_POINT('Ctrl Pts',(2.57150029033558,-7.4839764416326,23.2478498539537));
#65435=CARTESIAN_POINT('Ctrl Pts',(2.384927169524,-7.54549625696796,23.2399472429976));
#65436=CARTESIAN_POINT('Ctrl Pts',(2.19650032593727,-7.59995442868952,23.2320446320414));
#65437=CARTESIAN_POINT('Ctrl Pts',(2.00794850740072,-7.65444872003793,23.2241367796431));
#65438=CARTESIAN_POINT('Ctrl Pts',(1.81754084822449,-7.7018719475486,23.2162289272447));
#65439=CARTESIAN_POINT('Ctrl Pts',(1.62585157652943,-7.74212681703786,23.2083210748464));
#65440=CARTESIAN_POINT('Ctrl Pts',(1.43390001954144,-7.78243676660616,23.2004024022631));
#65441=CARTESIAN_POINT('Ctrl Pts',(1.24066368569655,-7.8155587091444,23.1924837296797));
#65442=CARTESIAN_POINT('Ctrl Pts',(1.04672269370989,-7.84144709874859,23.1845650570964));
#65443=CARTESIAN_POINT('Ctrl Pts',(0.966567311649314,-7.85214671278274,
23.1812922872718));
#65444=CARTESIAN_POINT('Ctrl Pts',(0.886291575390236,-7.86161134336304,
23.1780195174471));
#65445=CARTESIAN_POINT('Ctrl Pts',(0.805936402846742,-7.86984037414778,
23.1747467476225));
#65446=CARTESIAN_POINT('Ctrl Pts',(0.613366704165532,-7.8895610956458,23.1669036147036));
#65447=CARTESIAN_POINT('Ctrl Pts',(0.419770715722492,-7.90224040504155,
23.1590604817847));
#65448=CARTESIAN_POINT('Ctrl Pts',(0.225710951693573,-7.90777943333561,
23.1512173488658));
#65449=CARTESIAN_POINT('Ctrl Pts',(0.0318790902025709,-7.91331195663048,
23.1433834268718));
#65450=CARTESIAN_POINT('Ctrl Pts',(-0.162415114935045,-7.91172088590572,
23.1355495048777));
#65451=CARTESIAN_POINT('Ctrl Pts',(-0.35660128971044,-7.90295871937699,
23.1277155828836));
#65452=CARTESIAN_POINT('Ctrl Pts',(-0.55059717936082,-7.89420513898966,
23.1198893374341));
#65453=CARTESIAN_POINT('Ctrl Pts',(-0.744484901034405,-7.87829447231448,
23.1120630919846));
#65454=CARTESIAN_POINT('Ctrl Pts',(-0.93769112081678,-7.8552311463089,23.1042368465351));
#65455=CARTESIAN_POINT('Ctrl Pts',(-1.13074556891857,-7.83218593752414,
23.0964167489334));
#65456=CARTESIAN_POINT('Ctrl Pts',(-1.32311923407877,-7.80199930159378,
23.0885966513316));
#65457=CARTESIAN_POINT('Ctrl Pts',(-1.51424075520649,-7.76472767940201,
23.0807765537299));
#65458=CARTESIAN_POINT('Ctrl Pts',(-1.70524927526403,-7.72747809414867,
23.0729610797801));
#65459=CARTESIAN_POINT('Ctrl Pts',(-1.89500678198136,-7.68315193419874,
23.0651456058303));
#65460=CARTESIAN_POINT('Ctrl Pts',(-2.08294880594098,-7.63185726228086,
23.0573301318806));
#65461=CARTESIAN_POINT('Ctrl Pts',(-2.27081621400834,-7.5805829551416,23.0495177607949));
#65462=CARTESIAN_POINT('Ctrl Pts',(-2.45686923670015,-7.52234574061494,
23.0417053897093));
#65463=CARTESIAN_POINT('Ctrl Pts',(-2.64055515475202,-7.45730443757747,
23.0338930186236));
#65464=CARTESIAN_POINT('Ctrl Pts',(-2.82423411963755,-7.392265596585,23.026080943264));
#65465=CARTESIAN_POINT('Ctrl Pts',(-3.00554582402382,-7.3204232890152,23.0182688679044));
#65466=CARTESIAN_POINT('Ctrl Pts',(-3.18395378716133,-7.24198586585344,
23.0104567925449));
#65467=CARTESIAN_POINT('Ctrl Pts',(-3.36236696817639,-7.16354614864123,
23.0026444887064));
#65468=CARTESIAN_POINT('Ctrl Pts',(-3.53787591637705,-7.07851107249217,
22.9948321848679));
#65469=CARTESIAN_POINT('Ctrl Pts',(-3.70996521119385,-6.98713669050001,
22.9870198810295));
#65470=CARTESIAN_POINT('Ctrl Pts',(-3.8820898187468,-6.89574355847783,22.9792059741057));
#65471=CARTESIAN_POINT('Ctrl Pts',(-4.0507930643653,-6.79800869423773,22.9713920671819));
#65472=CARTESIAN_POINT('Ctrl Pts',(-4.21558503163935,-6.69423362611571,
22.9635781602581));
#65473=CARTESIAN_POINT('Ctrl Pts',(-4.38043981196355,-6.59041900249431,
22.9557612749407));
#65474=CARTESIAN_POINT('Ctrl Pts',(-4.54138004686675,-6.48055977616732,
22.9479443896234));
#65475=CARTESIAN_POINT('Ctrl Pts',(-4.69794552818048,-6.36500029962679,
22.9401275043061));
#65476=CARTESIAN_POINT('Ctrl Pts',(-4.8546808499172,-6.24931546550287,22.932302139322));
#65477=CARTESIAN_POINT('Ctrl Pts',(-5.00703165659419,-6.12791823983644,
22.9244767743379));
#65478=CARTESIAN_POINT('Ctrl Pts',(-5.15457070589401,-6.00119336781772,
22.9166514093538));
#65479=CARTESIAN_POINT('Ctrl Pts',(-5.30219942289215,-5.87439147803558,
22.9088212884596));
#65480=CARTESIAN_POINT('Ctrl Pts',(-5.44501029713251,-5.74225572714289,
22.9009911675653));
#65481=CARTESIAN_POINT('Ctrl Pts',(-5.58261354661621,-5.605207131689,22.893161046671));
#65482=CARTESIAN_POINT('Ctrl Pts',(-5.72040489062322,-5.4679711998871,22.8853202225204));
#65483=CARTESIAN_POINT('Ctrl Pts',(-5.85297415308385,-5.32580926684511,
22.8774793983697));
#65484=CARTESIAN_POINT('Ctrl Pts',(-5.97997163617299,-5.17917563233441,
22.8696385742191));
#65485=CARTESIAN_POINT('Ctrl Pts',(-6.04851157106872,-5.10003816032772,
22.8654069188843));
#65486=CARTESIAN_POINT('Ctrl Pts',(-6.11542934495411,-5.01959872920869,
22.8611752635496));
#65487=CARTESIAN_POINT('Ctrl Pts',(-6.18067532756721,-4.93793210718839,
22.8569436082148));
#65488=CARTESIAN_POINT('Ctrl Pts',(-6.30271867379094,-4.78517376978624,
22.849028249193));
#65489=CARTESIAN_POINT('Ctrl Pts',(-6.41926470017325,-4.62767631910825,
22.8411128901711));
#65490=CARTESIAN_POINT('Ctrl Pts',(-6.52992445675855,-4.46587142549207,
22.8331975311492));
#65491=CARTESIAN_POINT('Ctrl Pts',(-6.64110696691312,-4.30330217012168,
22.8252447801945));
#65492=CARTESIAN_POINT('Ctrl Pts',(-6.74634718042822,-4.13638489684024,
22.8172920292398));
#65493=CARTESIAN_POINT('Ctrl Pts',(-6.84528955920018,-3.96559350547998,
22.8093392782852));
#65494=CARTESIAN_POINT('Ctrl Pts',(-6.94352912354301,-3.79601529148324,
22.8014430178676));
#65495=CARTESIAN_POINT('Ctrl Pts',(-7.03555983439679,-3.62261810730013,
22.7935467574501));
#65496=CARTESIAN_POINT('Ctrl Pts',(-7.12107525983665,-3.44589729152545,
22.7856504970326));
#65497=CARTESIAN_POINT('Ctrl Pts',(-7.20652914612961,-3.26930364869278,
22.7777599189715));
#65498=CARTESIAN_POINT('Ctrl Pts',(-7.28547693697055,-3.08939144689937,
22.7698693409104));
#65499=CARTESIAN_POINT('Ctrl Pts',(-7.35765725544608,-2.90668207951638,
22.7619787628493));
#65500=CARTESIAN_POINT('Ctrl Pts',(-7.42979771891297,-2.72407359674528,
22.7540925416415));
#65501=CARTESIAN_POINT('Ctrl Pts',(-7.49517802851293,-2.53867134475953,
22.7462063204337));
#65502=CARTESIAN_POINT('Ctrl Pts',(-7.55358412795725,-2.35101846480887,
22.7383200992259));
#65503=CARTESIAN_POINT('Ctrl Pts',(-7.61282584253642,-2.16068083809245,
22.7303210499768));
#65504=CARTESIAN_POINT('Ctrl Pts',(-7.66489210879814,-1.96802801737583,
22.7223220007277));
#65505=CARTESIAN_POINT('Ctrl Pts',(-7.70961103913861,-1.773645574852,22.7143229514787));
#65506=CARTESIAN_POINT('Ctrl Pts',(-7.75367631114435,-1.58210442801016,
22.7064408246419));
#65507=CARTESIAN_POINT('Ctrl Pts',(-7.79060750583644,-1.38888422606102,
22.6985586978051));
#65508=CARTESIAN_POINT('Ctrl Pts',(-7.82029101971393,-1.19455823088774,
22.6906765709684));
#65509=CARTESIAN_POINT('Ctrl Pts',(-7.8506350154868,-0.995908327091516,
22.6826190605132));
#65510=CARTESIAN_POINT('Ctrl Pts',(-7.87340495139189,-0.796103210318132,
22.6745615500579));
#65511=CARTESIAN_POINT('Ctrl Pts',(-7.88853513891433,-0.595763679753899,
22.6665040396027));
#65512=CARTESIAN_POINT('Ctrl Pts',(-7.90366532643677,-0.395424149189665,
22.6584465291475));
#65513=CARTESIAN_POINT('Ctrl Pts',(-7.91115575002603,-0.194550588700236,
22.6503890186922));
#65514=CARTESIAN_POINT('Ctrl Pts',(-7.91099754422913,0.00623339398873903,
22.642331508237));
#65515=CARTESIAN_POINT('',(-7.91848594748034,0.000888686695662845,20.6423541988083));
#65516=CARTESIAN_POINT('Ctrl Pts',(-7.90381617034521,0.00628295359526841,
22.6423292903089));
#65517=CARTESIAN_POINT('Ctrl Pts',(-7.90984156749653,0.86262601629398,22.6079330164751));
#65518=CARTESIAN_POINT('Ctrl Pts',(-7.38540658840461,4.34883843418324,22.4676023628386));
#65519=CARTESIAN_POINT('Ctrl Pts',(-2.30235307566298,9.06792087288601,22.2213373293996));
#65520=CARTESIAN_POINT('Ctrl Pts',(6.38434810196999,6.83974694744736,21.9035341899918));
#65521=CARTESIAN_POINT('Ctrl Pts',(8.72304347646132,-0.234661512707255,
21.6386982404854));
#65522=CARTESIAN_POINT('Ctrl Pts',(6.40966022654009,-5.15172471127276,21.4268294808803));
#65523=CARTESIAN_POINT('Ctrl Pts',(2.10518128385569,-8.46845707787939,21.2149607212753));
#65524=CARTESIAN_POINT('Ctrl Pts',(-5.21263751244591,-7.71560869397964,
20.9534841473543));
#65525=CARTESIAN_POINT('Ctrl Pts',(-7.91649490000832,-2.53781226327639,
20.7449747633346));
#65526=CARTESIAN_POINT('Ctrl Pts',(-7.92424408506929,0.000873706451288429,
20.6423997591175));
#65527=CARTESIAN_POINT('',(-7.911,-2.74780198594726E-13,18.642331508237));
#65528=CARTESIAN_POINT('Ctrl Pts',(-7.91099994505201,0.000908162115281039,
20.6422949670549));
#65529=CARTESIAN_POINT('Ctrl Pts',(-7.9107335608261,2.20227658242684,20.5537197117162));
#65530=CARTESIAN_POINT('Ctrl Pts',(-6.94192137756157,4.38630738163188,20.4651444563776));
#65531=CARTESIAN_POINT('Ctrl Pts',(-3.67820201488333,7.34180684107607,20.2879817653061));
#65532=CARTESIAN_POINT('Ctrl Pts',(-1.40868175871801,8.08992666571325,20.1993943295734));
#65533=CARTESIAN_POINT('Ctrl Pts',(2.97309270521211,7.6545422802528,20.022219458108));
#65534=CARTESIAN_POINT('Ctrl Pts',(5.05102072675545,6.47444880834269,19.9336320223752));
#65535=CARTESIAN_POINT('Ctrl Pts',(7.66951518847842,2.93425195367783,19.7564571509098));
#65536=CARTESIAN_POINT('Ctrl Pts',(8.18956872247064,0.601881960100036,19.6678697151771));
#65537=CARTESIAN_POINT('Ctrl Pts',(7.32306689761385,-3.71537198232363,19.4906948437116));
#65538=CARTESIAN_POINT('Ctrl Pts',(5.94329958850271,-5.66643518936436,19.4021074079789));
#65539=CARTESIAN_POINT('Ctrl Pts',(2.16154501637954,-7.92205913232967,19.2249325365135));
#65540=CARTESIAN_POINT('Ctrl Pts',(-0.210816529299205,-8.20894963713004,
19.1363451007807));
#65541=CARTESIAN_POINT('Ctrl Pts',(-4.42123908576331,-6.91982244717898,
18.9591702293153));
#65542=CARTESIAN_POINT('Ctrl Pts',(-6.22631625634102,-5.35390358803619,
18.8705827935826));
#65543=CARTESIAN_POINT('Ctrl Pts',(-7.65317280859465,-2.31334857514614,
18.7354407413122));
#65544=CARTESIAN_POINT('Ctrl Pts',(-7.91099999999996,-1.15702837836581,
18.6888861247746));
#65545=CARTESIAN_POINT('Ctrl Pts',(-7.911,-2.74780198594726E-13,18.642331508237));
#65546=CARTESIAN_POINT('',(-7.9028343770497,0.00216472906886937,16.642331508237));
#65547=CARTESIAN_POINT('Ctrl Pts',(-7.911,-2.74780198594726E-13,18.642331508237));
#65548=CARTESIAN_POINT('Ctrl Pts',(-7.91100000000008,2.20167589666645,18.5537440725043));
#65549=CARTESIAN_POINT('Ctrl Pts',(-6.94214576672391,4.3861041833865,18.4651566367716));
#65550=CARTESIAN_POINT('Ctrl Pts',(-3.67820201488328,7.3418068410761,18.2879817653061));
#65551=CARTESIAN_POINT('Ctrl Pts',(-1.40868175871795,8.08992666571326,18.1993943295734));
#65552=CARTESIAN_POINT('Ctrl Pts',(2.97309270521216,7.65454228025278,18.022219458108));
#65553=CARTESIAN_POINT('Ctrl Pts',(5.05102072675549,6.47444880834266,17.9336320223752));
#65554=CARTESIAN_POINT('Ctrl Pts',(7.66951518847843,2.93425195367777,17.7564571509098));
#65555=CARTESIAN_POINT('Ctrl Pts',(8.18956872247064,0.601881960099978,17.6678697151771));
#65556=CARTESIAN_POINT('Ctrl Pts',(7.32306689761383,-3.71537198232368,17.4906948437116));
#65557=CARTESIAN_POINT('Ctrl Pts',(5.94329958850267,-5.6664351893644,17.4021074079789));
#65558=CARTESIAN_POINT('Ctrl Pts',(2.16154501637949,-7.92205913232969,17.2249325365135));
#65559=CARTESIAN_POINT('Ctrl Pts',(-0.210816529299263,-8.20894963713004,
17.1363451007807));
#65560=CARTESIAN_POINT('Ctrl Pts',(-4.42123908576336,-6.91982244717894,
16.9591702293153));
#65561=CARTESIAN_POINT('Ctrl Pts',(-6.22631625634105,-5.35390358803615,
16.8705827935826));
#65562=CARTESIAN_POINT('Ctrl Pts',(-7.65317280859467,-2.31334857514607,
16.7354407413122));
#65563=CARTESIAN_POINT('Ctrl Pts',(-7.91099999999997,-1.15702837836572,
16.6888861247746));
#65564=CARTESIAN_POINT('Ctrl Pts',(-7.911,-1.64868119156836E-13,16.642331508237));
#65565=CARTESIAN_POINT('',(-7.91527914730039,0.000969948445309178,14.6424015413963));
#65566=CARTESIAN_POINT('Ctrl Pts',(-7.89668078699942,0.00379606269054533,
16.642331508237));
#65567=CARTESIAN_POINT('Ctrl Pts',(-7.90106252337055,1.17903434357931,16.5951812788451));
#65568=CARTESIAN_POINT('Ctrl Pts',(-7.10778324508014,4.98943963042238,16.4420966696509));
#65569=CARTESIAN_POINT('Ctrl Pts',(-1.19022084510717,9.27962245901281,16.1830776806536));
#65570=CARTESIAN_POINT('Ctrl Pts',(7.1481032504245,6.02560715721669,15.8652745412461));
#65571=CARTESIAN_POINT('Ctrl Pts',(8.94447937923684,-2.74304707876909,15.5474714018383));
#65572=CARTESIAN_POINT('Ctrl Pts',(2.52814114509511,-9.00835952561415,15.2296682624306));
#65573=CARTESIAN_POINT('Ctrl Pts',(-4.73176752524436,-7.33191172920264,
14.9648323129244));
#65574=CARTESIAN_POINT('Ctrl Pts',(-7.50325925665173,-3.14592317945734,
14.7690954788964));
#65575=CARTESIAN_POINT('Ctrl Pts',(-7.91181181028092,-0.91279513892285,
14.679293024671));
#65576=CARTESIAN_POINT('Ctrl Pts',(-7.91746780378482,0.000959046564810386,
14.6424577603469));
#65577=CARTESIAN_POINT('',(-7.91553726929787,-0.000951753929678635,12.6422689007438));
#65578=CARTESIAN_POINT('Ctrl Pts',(-7.91099993453595,0.000991263561006212,
14.6422916233472));
#65579=CARTESIAN_POINT('Ctrl Pts',(-7.91070917900769,2.20233154695537,14.5537174825778));
#65580=CARTESIAN_POINT('Ctrl Pts',(-6.94190084478929,4.38632597532549,14.4651433418083));
#65581=CARTESIAN_POINT('Ctrl Pts',(-3.67820201488291,7.3418068410763,14.2879817653061));
#65582=CARTESIAN_POINT('Ctrl Pts',(-1.40868175871746,8.08992666571337,14.1993943295734));
#65583=CARTESIAN_POINT('Ctrl Pts',(2.97309270521278,7.65454228025256,14.0222194581079));
#65584=CARTESIAN_POINT('Ctrl Pts',(5.05102072675609,6.47444880834222,13.9336320223752));
#65585=CARTESIAN_POINT('Ctrl Pts',(7.66951518847877,2.93425195367695,13.7564571509098));
#65586=CARTESIAN_POINT('Ctrl Pts',(8.18956872247073,0.601881960099008,13.667869715177));
#65587=CARTESIAN_POINT('Ctrl Pts',(7.32306689761334,-3.71537198232469,13.4906948437116));
#65588=CARTESIAN_POINT('Ctrl Pts',(5.94329958850185,-5.66643518936529,13.4021074079789));
#65589=CARTESIAN_POINT('Ctrl Pts',(2.16154501637819,-7.92205913233006,13.2249325365134));
#65590=CARTESIAN_POINT('Ctrl Pts',(-0.210816529300703,-8.20894963713002,
13.1363451007807));
#65591=CARTESIAN_POINT('Ctrl Pts',(-4.4212390857647,-6.91982244717811,12.9591702293152));
#65592=CARTESIAN_POINT('Ctrl Pts',(-6.22631625634216,-5.35390358803489,
12.8705827935825));
#65593=CARTESIAN_POINT('Ctrl Pts',(-7.65303491965023,-2.31364240911259,
12.735453801206));
#65594=CARTESIAN_POINT('Ctrl Pts',(-7.91085532589086,-1.15767713118784,
12.6889122445621));
#65595=CARTESIAN_POINT('Ctrl Pts',(-7.91099993913047,-0.000973737913675424,
12.6423706879183));
#65596=CARTESIAN_POINT('',(-7.89704659861909,-0.00212787115983104,10.6422490387989));
#65597=CARTESIAN_POINT('Ctrl Pts',(-7.91798387824917,-0.000939899775352797,
12.642214015293));
#65598=CARTESIAN_POINT('Ctrl Pts',(-7.91240748074079,0.9404534482577,12.6042565360171));
#65599=CARTESIAN_POINT('Ctrl Pts',(-7.48579772889252,3.20106885968654,12.5133318668401));
#65600=CARTESIAN_POINT('Ctrl Pts',(-4.65416054181148,7.3814187774994,12.3164728178603));
#65601=CARTESIAN_POINT('Ctrl Pts',(2.6230288800739,8.9811891465743,12.051636868354));
#65602=CARTESIAN_POINT('Ctrl Pts',(8.97291786243676,2.64853991397236,11.7338337289462));
#65603=CARTESIAN_POINT('Ctrl Pts',(7.08414191259461,-6.1006766062498,11.4160305895387));
#65604=CARTESIAN_POINT('Ctrl Pts',(-1.28804455293763,-9.26655059186473,
11.0982274501309));
#65605=CARTESIAN_POINT('Ctrl Pts',(-7.13464643336658,-4.93299045016783,
10.8403277563637));
#65606=CARTESIAN_POINT('Ctrl Pts',(-7.90190329265851,-1.1513941715232,10.6883624423991));
#65607=CARTESIAN_POINT('Ctrl Pts',(-7.89705579113888,-0.00418322831448492,
10.642331508237));
#65608=CARTESIAN_POINT('',(-7.90817188740471,-3.24836861786255E-5,8.64270656474482));
#65609=CARTESIAN_POINT('Ctrl Pts',(-7.89703740609931,-7.2514005176659E-5,
10.6421665693608));
#65610=CARTESIAN_POINT('Ctrl Pts',(-7.89702702068455,0.00212803473133817,
10.6420782743881));
#65611=CARTESIAN_POINT('Ctrl Pts',(-7.8970167925981,0.00413170092462163,
10.6419978793563));
#65612=CARTESIAN_POINT('Ctrl Pts',(-7.89700473044708,0.00632931527902227,
10.6419097025558));
#65613=CARTESIAN_POINT('Ctrl Pts',(-7.89555713694605,0.27006770257325,10.631327496845));
#65614=CARTESIAN_POINT('Ctrl Pts',(-7.88121311475603,0.534201069122857,
10.620936877814));
#65615=CARTESIAN_POINT('Ctrl Pts',(-7.85413508916187,0.797232455759467,
10.6106644974064));
#65616=CARTESIAN_POINT('Ctrl Pts',(-7.82687300158976,1.06205178949431,10.6003222908348));
#65617=CARTESIAN_POINT('Ctrl Pts',(-7.78670404858205,1.32575354639783,10.5900999357962));
#65618=CARTESIAN_POINT('Ctrl Pts',(-7.73382622050846,1.58685167858934,10.579922578301));
#65619=CARTESIAN_POINT('Ctrl Pts',(-7.68088919018293,1.84824213741315,10.5697338261911));
#65620=CARTESIAN_POINT('Ctrl Pts',(-7.61521569910729,2.10702279727448,10.5595901724399));
#65621=CARTESIAN_POINT('Ctrl Pts',(-7.5370235017524,2.36175098493019,10.5494165113558));
#65622=CARTESIAN_POINT('Ctrl Pts',(-7.45905535631495,2.6157492744528,10.5392720018796));
#65623=CARTESIAN_POINT('Ctrl Pts',(-7.36864102369296,2.8657181736505,10.5290976567902));
#65624=CARTESIAN_POINT('Ctrl Pts',(-7.26600211153003,3.11027875781575,10.5188190141712));
#65625=CARTESIAN_POINT('Ctrl Pts',(-7.16384440122462,3.35369276896209,10.508588560897));
#65626=CARTESIAN_POINT('Ctrl Pts',(-7.04957730822994,3.59174915994034,10.4982547857566));
#65627=CARTESIAN_POINT('Ctrl Pts',(-6.92341216917452,3.82313929640141,10.4877442692305));
#65628=CARTESIAN_POINT('Ctrl Pts',(-6.84744917416091,3.96245739895959,10.4814159734711));
#65629=CARTESIAN_POINT('Ctrl Pts',(-6.76717276827334,4.09935987343639,10.4750236063915));
#65630=CARTESIAN_POINT('Ctrl Pts',(-6.68262590130838,4.23356965677974,10.4685511429316));
#65631=CARTESIAN_POINT('Ctrl Pts',(-6.54417057120691,4.45335378980207,10.4579517310659));
#65632=CARTESIAN_POINT('Ctrl Pts',(-6.3942646586491,4.66591471059473,10.4471375177489));
#65633=CARTESIAN_POINT('Ctrl Pts',(-6.2341008017312,4.87068285980329,10.436038125106));
#65634=CARTESIAN_POINT('Ctrl Pts',(-6.09355091025868,5.05037471851674,10.4262979848435));
#65635=CARTESIAN_POINT('Ctrl Pts',(-5.94510155572144,5.22406642500045,10.4163382356336));
#65636=CARTESIAN_POINT('Ctrl Pts',(-5.78953492220527,5.39139621295431,10.4061113183207));
#65637=CARTESIAN_POINT('Ctrl Pts',(-5.70004020286178,5.48765806597681,10.4002279545558));
#65638=CARTESIAN_POINT('Ctrl Pts',(-5.60808757673465,5.58164513007581,10.3943687592721));
#65639=CARTESIAN_POINT('Ctrl Pts',(-5.51362768341834,5.67309653812542,10.3886852955563));
#65640=CARTESIAN_POINT('Ctrl Pts',(-5.44683502953349,5.73776189006145,10.3846665145531));
#65641=CARTESIAN_POINT('Ctrl Pts',(-5.37878938090202,5.80115853730033,10.3807355978151));
#65642=CARTESIAN_POINT('Ctrl Pts',(-5.3094837862637,5.8631825275386,10.3769461295963));
#65643=CARTESIAN_POINT('Ctrl Pts',(-5.13111694733864,6.0228092233927,10.3671934469895));
#65644=CARTESIAN_POINT('Ctrl Pts',(-4.94564170770916,6.17430019275652,10.3575033034082));
#65645=CARTESIAN_POINT('Ctrl Pts',(-4.75385236145091,6.31723214046822,10.3478841393255));
#65646=CARTESIAN_POINT('Ctrl Pts',(-4.55885457981442,6.46255519032749,10.3381040566779));
#65647=CARTESIAN_POINT('Ctrl Pts',(-4.3573289131039,6.59903091686291,10.3283973482188));
#65648=CARTESIAN_POINT('Ctrl Pts',(-4.15007692950517,6.72617240645461,10.3187728851479));
#65649=CARTESIAN_POINT('Ctrl Pts',(-4.04720521653535,6.78928042885673,10.3139956811602));
#65650=CARTESIAN_POINT('Ctrl Pts',(-3.94292225070908,6.85008805127412,10.3092387402827));
#65651=CARTESIAN_POINT('Ctrl Pts',(-3.83732397753682,6.90853144666653,10.3045031473766));
#65652=CARTESIAN_POINT('Ctrl Pts',(-3.620076390972,7.0287671874437,10.2947606004685));
#65653=CARTESIAN_POINT('Ctrl Pts',(-3.3972622476175,7.13899997770821,10.2851084087083));
#65654=CARTESIAN_POINT('Ctrl Pts',(-3.16976350958247,7.23873507443482,10.275556018546));
#65655=CARTESIAN_POINT('Ctrl Pts',(-2.94226477154745,7.33847017116143,10.2660036283837));
#65656=CARTESIAN_POINT('Ctrl Pts',(-2.71008049778106,7.42770786090225,10.2565510398193));
#65657=CARTESIAN_POINT('Ctrl Pts',(-2.47409109842804,7.50589469250486,10.2472076993025));
#65658=CARTESIAN_POINT('Ctrl Pts',(-2.19846253296326,7.59721457505867,10.2362949568219));
#65659=CARTESIAN_POINT('Ctrl Pts',(-1.91787860110224,7.67403236286004,10.2251698700566));
#65660=CARTESIAN_POINT('Ctrl Pts',(-1.6340284544711,7.73543001613488,10.213830036402));
#65661=CARTESIAN_POINT('Ctrl Pts',(-1.35036972588251,7.79678626510274,10.202497849912));
#65662=CARTESIAN_POINT('Ctrl Pts',(-1.06345026831751,7.84274278214282,10.1909512060697));
#65663=CARTESIAN_POINT('Ctrl Pts',(-0.774977872832234,7.87242967015964,
10.1791877071281));
#65664=CARTESIAN_POINT('Ctrl Pts',(-0.53831386443594,7.89678492225596,10.1695368814135));
#65665=CARTESIAN_POINT('Ctrl Pts',(-0.300605292751217,7.91019043798737,
10.1597400984903));
#65666=CARTESIAN_POINT('Ctrl Pts',(-0.0627986367552478,7.91219190920741,
10.1497960343608));
#65667=CARTESIAN_POINT('Ctrl Pts',(0.219271870481511,7.91456592182659,10.1380010440092));
#65668=CARTESIAN_POINT('Ctrl Pts',(0.501479517216926,7.90089439683192,10.1259988417638));
#65669=CARTESIAN_POINT('Ctrl Pts',(0.782278769383866,7.87199419134308,10.1137872181538));
#65670=CARTESIAN_POINT('Ctrl Pts',(1.01297476499424,7.84825067483746,10.1037545252425));
#65671=CARTESIAN_POINT('Ctrl Pts',(1.24234299120268,7.81377352999714,10.0938813063388));
#65672=CARTESIAN_POINT('Ctrl Pts',(1.46963759991846,7.76913012586632,10.0841330693608));
#65673=CARTESIAN_POINT('Ctrl Pts',(1.70346444832434,7.72320371102965,10.0741046769455));
#65674=CARTESIAN_POINT('Ctrl Pts',(1.93509725439572,7.66651851932442,10.0642085534158));
#65675=CARTESIAN_POINT('Ctrl Pts',(2.16375259399093,7.59964465304451,10.0544071465934));
#65676=CARTESIAN_POINT('Ctrl Pts',(2.39560012060677,7.53183718124139,10.0444689053385));
#65677=CARTESIAN_POINT('Ctrl Pts',(2.624387123297,7.45355465361222,10.034628043873));
#65678=CARTESIAN_POINT('Ctrl Pts',(2.84931711292389,7.36534096512308,10.0248454151962));
#65679=CARTESIAN_POINT('Ctrl Pts',(3.07724198741346,7.27595273409839,10.0149325333389));
#65680=CARTESIAN_POINT('Ctrl Pts',(3.30120723175786,7.1763671808047,10.0050794453031));
#65681=CARTESIAN_POINT('Ctrl Pts',(3.52039379899349,7.06709768473889,9.99524541947884));
#65682=CARTESIAN_POINT('Ctrl Pts',(3.6483425847122,7.00331230083493,9.98950486850069));
#65683=CARTESIAN_POINT('Ctrl Pts',(3.77466312743019,6.93622606141243,9.98377081309979));
#65684=CARTESIAN_POINT('Ctrl Pts',(3.89919232314342,6.86593288751937,9.97803515116346));
#65685=CARTESIAN_POINT('Ctrl Pts',(4.1684164793643,6.7139635415274,9.96563501691116));
#65686=CARTESIAN_POINT('Ctrl Pts',(4.42910711837882,6.54663212729827,9.9534595189747));
#65687=CARTESIAN_POINT('Ctrl Pts',(4.67936144343141,6.36497348585735,9.94142699231249));
#65688=CARTESIAN_POINT('Ctrl Pts',(4.92193896997612,6.18888740260204,9.92976357528588));
#65689=CARTESIAN_POINT('Ctrl Pts',(5.15471203616973,5.99933981309755,9.91823449250182));
#65690=CARTESIAN_POINT('Ctrl Pts',(5.37594902342265,5.79722587738221,9.90676536619906));
#65691=CARTESIAN_POINT('Ctrl Pts',(5.58221097229248,5.60879258332934,9.89607255948345));
#65692=CARTESIAN_POINT('Ctrl Pts',(5.77844670814061,5.40943631042047,9.88543186730674));
#65693=CARTESIAN_POINT('Ctrl Pts',(5.96323750513471,5.19984156073173,9.87478301605315));
#65694=CARTESIAN_POINT('Ctrl Pts',(6.10325066591985,5.04103482432902,9.86671454431647));
#65695=CARTESIAN_POINT('Ctrl Pts',(6.2366932871527,4.87634952504931,9.85864138856705));
#65696=CARTESIAN_POINT('Ctrl Pts',(6.36293627257074,4.70606719169118,9.85053733121235));
#65697=CARTESIAN_POINT('Ctrl Pts',(6.45160000815178,4.58647347542257,9.84484564073109));
#65698=CARTESIAN_POINT('Ctrl Pts',(6.53673968783333,4.46439922780143,9.83903742432002));
#65699=CARTESIAN_POINT('Ctrl Pts',(6.61812466727398,4.3399314349128,9.83313430227379));
#65700=CARTESIAN_POINT('Ctrl Pts',(6.75370500146756,4.13257886110665,9.82330021169203));
#65701=CARTESIAN_POINT('Ctrl Pts',(6.87886655377201,3.91858118728099,9.81320273256478));
#65702=CARTESIAN_POINT('Ctrl Pts',(6.99344417898774,3.69901002383476,9.80294182320879));
#65703=CARTESIAN_POINT('Ctrl Pts',(7.10858965371848,3.4783506603282,9.79263006053488));
#65704=CARTESIAN_POINT('Ctrl Pts',(7.2130450888691,3.2520621136234,9.7821532436896));
#65705=CARTESIAN_POINT('Ctrl Pts',(7.30662205930488,3.02128078655226,9.77161282455504));
#65706=CARTESIAN_POINT('Ctrl Pts',(7.40058146661728,2.78955628628909,9.76102932810184));
#65707=CARTESIAN_POINT('Ctrl Pts',(7.48357232131068,2.5533021140594,9.75038170842851));
#65708=CARTESIAN_POINT('Ctrl Pts',(7.55539753140135,2.31372078523287,9.73977266636942));
#65709=CARTESIAN_POINT('Ctrl Pts',(7.61423297563002,2.11746832885144,9.73108229565418));
#65710=CARTESIAN_POINT('Ctrl Pts',(7.66557588020918,1.91898436532077,9.72241781062201));
#65711=CARTESIAN_POINT('Ctrl Pts',(7.70932182241582,1.71895566935502,9.71383566080776));
#65712=CARTESIAN_POINT('Ctrl Pts',(7.75822972503801,1.49532386511304,9.70424082923638));
#65713=CARTESIAN_POINT('Ctrl Pts',(7.79765925323227,1.26973381984225,9.69474443889133));
#65714=CARTESIAN_POINT('Ctrl Pts',(7.82759777935467,1.04295255634549,9.68534929909551));
#65715=CARTESIAN_POINT('Ctrl Pts',(7.85781617323768,0.814051323278355,9.67586633277394));
#65716=CARTESIAN_POINT('Ctrl Pts',(7.87836535250214,0.583935620769487,9.66648651884618));
#65717=CARTESIAN_POINT('Ctrl Pts',(7.88918039584671,0.353385737595114,9.65721274615922));
#65718=CARTESIAN_POINT('Ctrl Pts',(7.89991464852466,0.124558110925905,9.64800825052032));
#65719=CARTESIAN_POINT('Ctrl Pts',(7.90105957925932,-0.104698090131597,
9.63890821773866));
#65720=CARTESIAN_POINT('Ctrl Pts',(7.89250110137832,-0.333615219723845,
9.62991547240277));
#65721=CARTESIAN_POINT('Ctrl Pts',(7.88416383567005,-0.556615496306306,
9.62115516381114));
#65722=CARTESIAN_POINT('Ctrl Pts',(7.86661808081932,-0.779294703447366,
9.61249666819413));
#65723=CARTESIAN_POINT('Ctrl Pts',(7.83971248071679,-1.00092736644294,9.60394259673));
#65724=CARTESIAN_POINT('Ctrl Pts',(7.81714654705787,-1.18681238483126,9.59676823122847));
#65725=CARTESIAN_POINT('Ctrl Pts',(7.78799582433962,-1.37196117934447,9.58966732087001));
#65726=CARTESIAN_POINT('Ctrl Pts',(7.75214648273455,-1.55593149415293,9.58264140617834));
#65727=CARTESIAN_POINT('Ctrl Pts',(7.70467843800058,-1.7995262365404,9.57333840595717));
#65728=CARTESIAN_POINT('Ctrl Pts',(7.64595391924143,-2.04102238733024,9.56389437275389));
#65729=CARTESIAN_POINT('Ctrl Pts',(7.57581145299394,-2.27912565841045,9.55431751332156));
#65730=CARTESIAN_POINT('Ctrl Pts',(7.50656737413922,-2.51417929368003,9.54486331467144));
#65731=CARTESIAN_POINT('Ctrl Pts',(7.42619596540761,-2.74592550209097,9.53527967048953));
#65732=CARTESIAN_POINT('Ctrl Pts',(7.33459218539083,-2.97312081782567,9.52557447621325));
#65733=CARTESIAN_POINT('Ctrl Pts',(7.30181172033032,-3.05442279147776,9.5221014668918));
#65734=CARTESIAN_POINT('Ctrl Pts',(7.26759334344641,-3.13514207242139,9.51861289222605));
#65735=CARTESIAN_POINT('Ctrl Pts',(7.23193383328093,-3.21522206971646,9.51510911402665));
#65736=CARTESIAN_POINT('Ctrl Pts',(7.1325267868186,-3.43845889980398,9.50534172685153));
#65737=CARTESIAN_POINT('Ctrl Pts',(7.02191693766909,-3.65672597042445,9.4954561911977));
#65738=CARTESIAN_POINT('Ctrl Pts',(6.90104335864473,-3.86925749793192,9.48546034509179));
#65739=CARTESIAN_POINT('Ctrl Pts',(6.77871191293198,-4.08435238656995,9.47534393822167));
#65740=CARTESIAN_POINT('Ctrl Pts',(6.64586829745989,-4.29357193377647,9.46511454392482));
#65741=CARTESIAN_POINT('Ctrl Pts',(6.50353113152558,-4.49615234994838,9.45478028726757));
#65742=CARTESIAN_POINT('Ctrl Pts',(6.36119286381313,-4.69873433421864,9.44444595061675));
#65743=CARTESIAN_POINT('Ctrl Pts',(6.20936163863106,-4.89467652984285,9.43400674998211));
#65744=CARTESIAN_POINT('Ctrl Pts',(6.0490904654515,-5.08325368747344,9.42347081061866));
#65745=CARTESIAN_POINT('Ctrl Pts',(5.91049103437001,-5.24633159003101,9.41435953269691));
#65746=CARTESIAN_POINT('Ctrl Pts',(5.76558064259386,-5.40390197968804,9.4051759091224));
#65747=CARTESIAN_POINT('Ctrl Pts',(5.61505461253099,-5.55552384739372,9.39592519468185));
#65748=CARTESIAN_POINT('Ctrl Pts',(5.47480690155528,-5.6967925692932,9.38730614371349));
#65749=CARTESIAN_POINT('Ctrl Pts',(5.32928970466327,-5.83266074883043,9.37888526581639));
#65750=CARTESIAN_POINT('Ctrl Pts',(5.17898788440507,-5.96294046145067,9.37060028741146));
#65751=CARTESIAN_POINT('Ctrl Pts',(5.02767409623669,-6.09409733502806,9.36225952703219));
#65752=CARTESIAN_POINT('Ctrl Pts',(4.87151084921231,-6.21959087718161,9.35405650230249));
#65753=CARTESIAN_POINT('Ctrl Pts',(4.71094050224414,-6.33922128397126,9.34592767330901));
#65754=CARTESIAN_POINT('Ctrl Pts',(4.55019310037605,-6.45898360272413,9.33778988096065));
#65755=CARTESIAN_POINT('Ctrl Pts',(4.38502860122831,-6.57287052360287,9.32972644806442));
#65756=CARTESIAN_POINT('Ctrl Pts',(4.21584208175296,-6.68066364004644,9.32167362428589));
#65757=CARTESIAN_POINT('Ctrl Pts',(4.16007671984261,-6.71619319741638,9.31901934288213));
#65758=CARTESIAN_POINT('Ctrl Pts',(4.10387402278031,-6.75106052327771,9.31636621407356));
#65759=CARTESIAN_POINT('Ctrl Pts',(4.04724706045905,-6.78525717371924,9.31371195500284));
#65760=CARTESIAN_POINT('Ctrl Pts',(3.86877282023437,-6.89303659460988,9.3053463840524));
#65761=CARTESIAN_POINT('Ctrl Pts',(3.68574723757595,-6.99386394134694,9.29720584355353));
#65762=CARTESIAN_POINT('Ctrl Pts',(3.49889719965554,-7.08730734369488,9.28920532526346));
#65763=CARTESIAN_POINT('Ctrl Pts',(3.31226265849002,-7.18064297646356,9.28121403408274));
#65764=CARTESIAN_POINT('Ctrl Pts',(3.12181315928759,-7.26661192393304,9.27336244231793));
#65765=CARTESIAN_POINT('Ctrl Pts',(2.92825622783153,-7.34483285249033,9.26556583551076));
#65766=CARTESIAN_POINT('Ctrl Pts',(2.73518574491443,-7.42285719570125,9.25778882318653));
#65767=CARTESIAN_POINT('Ctrl Pts',(2.5390240120457,-7.49317274126278,9.25006651979013));
#65768=CARTESIAN_POINT('Ctrl Pts',(2.34044700890272,-7.55544561978073,9.24231484797419));
#65769=CARTESIAN_POINT('Ctrl Pts',(2.14248387900954,-7.61752599033601,9.23458713937601));
#65770=CARTESIAN_POINT('Ctrl Pts',(1.9421208672976,-7.67161374140195,9.22683024365442));
#65771=CARTESIAN_POINT('Ctrl Pts',(1.73999367948123,-7.7174170398759,9.21896086079442));
#65772=CARTESIAN_POINT('Ctrl Pts',(1.56613390118553,-7.75681476466454,9.21219200810249));
#65773=CARTESIAN_POINT('Ctrl Pts',(1.39096847410628,-7.7900839588043,9.2053399308244));
#65774=CARTESIAN_POINT('Ctrl Pts',(1.21487801380399,-7.81705842571823,9.19835161768601));
#65775=CARTESIAN_POINT('Ctrl Pts',(1.0098590372569,-7.84846431556657,9.19021524956609));
#65776=CARTESIAN_POINT('Ctrl Pts',(0.803587424053422,-7.87133746293345,
9.18189420653297));
#65777=CARTESIAN_POINT('Ctrl Pts',(0.596720111584622,-7.88607584164099,
9.17330482375524));
#65778=CARTESIAN_POINT('Ctrl Pts',(0.39076607409736,-7.9007491535558,9.16475336126711));
#65779=CARTESIAN_POINT('Ctrl Pts',(0.184221793699587,-7.90736010137687,
9.15593592312961));
#65780=CARTESIAN_POINT('Ctrl Pts',(-0.0223140826013648,-7.90631499665483,
9.14676994771359));
#65781=CARTESIAN_POINT('Ctrl Pts',(-0.131389206576435,-7.90576305900039,
9.14192923953853));
#65782=CARTESIAN_POINT('Ctrl Pts',(-0.240462840871124,-7.90307594974536,
9.13699132164999));
#65783=CARTESIAN_POINT('Ctrl Pts',(-0.349452669468577,-7.89831402156496,
9.13194403305901));
#65784=CARTESIAN_POINT('Ctrl Pts',(-0.533994996194332,-7.89025109204741,
9.12339792933334));
#65785=CARTESIAN_POINT('Ctrl Pts',(-0.718108056857789,-7.87516509976259,
9.11517006747972));
#65786=CARTESIAN_POINT('Ctrl Pts',(-0.901368396608811,-7.85341029818643,
9.10717206460129));
#65787=CARTESIAN_POINT('Ctrl Pts',(-1.08568892050605,-7.83152964234323,
9.0991277922689));
#65788=CARTESIAN_POINT('Ctrl Pts',(-1.26914711928099,-7.80290320176188,
9.0913160461308));
#65789=CARTESIAN_POINT('Ctrl Pts',(-1.45135891336227,-7.76786640856552,
9.08364690048055));
#65790=CARTESIAN_POINT('Ctrl Pts',(-1.63498581304967,-7.73255751024708,
9.07591819419066));
#65791=CARTESIAN_POINT('Ctrl Pts',(-1.81734721592646,-7.69073871274669,
9.06833431193674));
#65792=CARTESIAN_POINT('Ctrl Pts',(-1.99809262181031,-7.64272181670799,
9.06080321653726));
#65793=CARTESIAN_POINT('Ctrl Pts',(-2.10335603487673,-7.61475749674548,
9.05641721954883));
#65794=CARTESIAN_POINT('Ctrl Pts',(-2.20807211685569,-7.58469033334239,
9.05204912639857));
#65795=CARTESIAN_POINT('Ctrl Pts',(-2.31217745076366,-7.55257622973733,
9.04768075708763));
#65796=CARTESIAN_POINT('Ctrl Pts',(-2.53339558011493,-7.48433551950067,
9.0383982116982));
#65797=CARTESIAN_POINT('Ctrl Pts',(-2.75200593699641,-7.40633864216497,
9.02935840111635));
#65798=CARTESIAN_POINT('Ctrl Pts',(-2.96702330165383,-7.31902232135849,
9.0204752354755));
#65799=CARTESIAN_POINT('Ctrl Pts',(-3.18265007296923,-7.2314585268313,9.01156689298304));
#65800=CARTESIAN_POINT('Ctrl Pts',(-3.39466327846068,-7.13452322304539,
9.00281608462254));
#65801=CARTESIAN_POINT('Ctrl Pts',(-3.60212000872174,-7.02867003300061,
8.99413598645784));
#65802=CARTESIAN_POINT('Ctrl Pts',(-3.82000675679168,-6.91749500714021,
8.98501949088956));
#65803=CARTESIAN_POINT('Ctrl Pts',(-4.03286685373061,-6.79648380236499,
8.97598099424619));
#65804=CARTESIAN_POINT('Ctrl Pts',(-4.23966966324943,-6.66616269160833,
8.96691990779514));
#65805=CARTESIAN_POINT('Ctrl Pts',(-4.4361580294336,-6.54234144279908,8.95831074974374));
#65806=CARTESIAN_POINT('Ctrl Pts',(-4.62717887254434,-6.41011651956876,
8.94968119905727));
#65807=CARTESIAN_POINT('Ctrl Pts',(-4.81190003464847,-6.26992772426865,
8.94094497962545));
#65808=CARTESIAN_POINT('Ctrl Pts',(-4.99616121317992,-6.13008802022683,
8.93223051469852));
#65809=CARTESIAN_POINT('Ctrl Pts',(-5.17415435597442,-5.98232474636406,
8.92340991160736));
#65810=CARTESIAN_POINT('Ctrl Pts',(-5.34510027977848,-5.82705221848147,
8.91439753715966));
#65811=CARTESIAN_POINT('Ctrl Pts',(-5.51533200361693,-5.67242840822611,
8.90542281577428));
#65812=CARTESIAN_POINT('Ctrl Pts',(-5.67857572524734,-5.51035857045978,
8.89625792209928));
#65813=CARTESIAN_POINT('Ctrl Pts',(-5.83410269058135,-5.34122009760758,
8.88681829177263));
#65814=CARTESIAN_POINT('Ctrl Pts',(-5.86019177437216,-5.31284773284747,
8.88523482805612));
#65815=CARTESIAN_POINT('Ctrl Pts',(-5.88606380104645,-5.28427638023463,
8.88364363356768));
#65816=CARTESIAN_POINT('Ctrl Pts',(-5.91171542817903,-5.25550771479195,
8.88204430914758));
#65817=CARTESIAN_POINT('Ctrl Pts',(-6.06300674317755,-5.085832348661,8.87261161728062));
#65818=CARTESIAN_POINT('Ctrl Pts',(-6.2066291982959,-4.90929692272948,8.86289612173482));
#65819=CARTESIAN_POINT('Ctrl Pts',(-6.34255282084846,-4.72680038854599,
8.85281593003401));
#65820=CARTESIAN_POINT('Ctrl Pts',(-6.42443673137412,-4.61685974985719,
8.8467433614855));
#65821=CARTESIAN_POINT('Ctrl Pts',(-6.50352715000144,-4.50475489559639,
8.84053843851567));
#65822=CARTESIAN_POINT('Ctrl Pts',(-6.57982143804972,-4.39067407350341,
8.83418325692507));
#65823=CARTESIAN_POINT('Ctrl Pts',(-6.66262998064053,-4.26685265964994,
8.82728544925323));
#65824=CARTESIAN_POINT('Ctrl Pts',(-6.74183405868872,-4.14066738188957,
8.82037815828341));
#65825=CARTESIAN_POINT('Ctrl Pts',(-6.81720648710848,-4.01222251231833,
8.81359871654385));
#65826=CARTESIAN_POINT('Ctrl Pts',(-6.89252770279151,-3.88386491621602,
8.80682388118055));
#65827=CARTESIAN_POINT('Ctrl Pts',(-6.96402204106891,-3.75325047507872,
8.80017672136903));
#65828=CARTESIAN_POINT('Ctrl Pts',(-7.0314313039316,-3.62052458635116,8.79379428989082));
#65829=CARTESIAN_POINT('Ctrl Pts',(-7.0752591266859,-3.53422952126631,8.78964459200525));
#65830=CARTESIAN_POINT('Ctrl Pts',(-7.1173594500746,-3.44704274577096,8.78560680210125));
#65831=CARTESIAN_POINT('Ctrl Pts',(-7.15765548612065,-3.35901452181828,
8.78171858872071));
#65832=CARTESIAN_POINT('Ctrl Pts',(-7.25215275396775,-3.1525816447121,8.77260043275997));
#65833=CARTESIAN_POINT('Ctrl Pts',(-7.33793684335818,-2.94228142107834,
8.76349613287821));
#65834=CARTESIAN_POINT('Ctrl Pts',(-7.41492855600244,-2.72885753313259,
8.7543997876551));
#65835=CARTESIAN_POINT('Ctrl Pts',(-7.49370634335228,-2.51048257974443,
8.74509242293966));
#65836=CARTESIAN_POINT('Ctrl Pts',(-7.56327943433531,-2.28883665517175,
8.73579338623242));
#65837=CARTESIAN_POINT('Ctrl Pts',(-7.62351601627474,-2.06468814798325,
8.72649635580341));
#65838=CARTESIAN_POINT('Ctrl Pts',(-7.68355400772679,-1.84127862298557,
8.71722997621388));
#65839=CARTESIAN_POINT('Ctrl Pts',(-7.73431710757442,-1.61538216568751,
8.70796558969562));
#65840=CARTESIAN_POINT('Ctrl Pts',(-7.77562516852486,-1.38774352143513,
8.69869693683797));
#65841=CARTESIAN_POINT('Ctrl Pts',(-7.81713818439863,-1.15897542061162,
8.68938229644199));
#65842=CARTESIAN_POINT('Ctrl Pts',(-7.84910234635378,-0.928446981403521,
8.68006334726568));
#65843=CARTESIAN_POINT('Ctrl Pts',(-7.87128150063596,-0.696910155248286,
8.67073373626488));
#65844=CARTESIAN_POINT('Ctrl Pts',(-7.89346065491813,-0.46537332909306,
8.66140412526407));
#65845=CARTESIAN_POINT('Ctrl Pts',(-7.90585501534277,-0.232827279694014,
8.65206385243877));
#65846=CARTESIAN_POINT('Ctrl Pts',(-7.90817188740471,-3.24836861791286E-5,
8.64270656474482));
#65847=CARTESIAN_POINT('',(-7.91099726676438,-0.00657611181310816,4.63857422362495));
#65848=CARTESIAN_POINT('Ctrl Pts',(-7.91099897267188,0.00403167266891616,
8.64093322807217));
#65849=CARTESIAN_POINT('Ctrl Pts',(-7.91071147929497,0.568154803721865,
8.62151017142005));
#65850=CARTESIAN_POINT('Ctrl Pts',(-7.85008557225209,1.13058901663712,8.60282672000359));
#65851=CARTESIAN_POINT('Ctrl Pts',(-7.70446776992235,1.79992327657939,8.57706428746811));
#65852=CARTESIAN_POINT('Ctrl Pts',(-7.67605254157754,1.91748852523687,8.57239830883372));
#65853=CARTESIAN_POINT('Ctrl Pts',(-7.6399084192444,2.05331572809818,8.56679485636979));
#65854=CARTESIAN_POINT('Ctrl Pts',(-7.6347912945223,2.0722615688514,8.56600840973354));
#65855=CARTESIAN_POINT('Ctrl Pts',(-7.62806804450101,2.09679103890409,8.56498366270866));
#65856=CARTESIAN_POINT('Ctrl Pts',(-7.62652615056634,2.10239235794477,8.56474921959791));
#65857=CARTESIAN_POINT('Ctrl Pts',(-7.62402124448975,2.11145304428912,8.56436926261314));
#65858=CARTESIAN_POINT('Ctrl Pts',(-7.62306204223672,2.11491347217686,8.56422398012812));
#65859=CARTESIAN_POINT('Ctrl Pts',(-7.62122376175076,2.12152777333931,8.56394595733856));
#65860=CARTESIAN_POINT('Ctrl Pts',(-7.62034508045135,2.12468175842142,8.56381324124017));
#65861=CARTESIAN_POINT('Ctrl Pts',(-7.61833566936705,2.13187716354249,8.56351013942218));
#65862=CARTESIAN_POINT('Ctrl Pts',(-7.61720368449931,2.13591821948406,8.56333967710951));
#65863=CARTESIAN_POINT('Ctrl Pts',(-7.61420202700498,2.14660105771514,8.56288842810637));
#65864=CARTESIAN_POINT('Ctrl Pts',(-7.61232688358175,2.15324128371969,8.56260730836368));
#65865=CARTESIAN_POINT('Ctrl Pts',(-7.60015111553249,2.1961432186556,8.56078696564003));
#65866=CARTESIAN_POINT('Ctrl Pts',(-7.58960026718761,2.23233279484788,8.55923271180766));
#65867=CARTESIAN_POINT('Ctrl Pts',(-7.57802455891257,2.2710068109678,8.55755275284633));
#65868=CARTESIAN_POINT('Ctrl Pts',(-7.57725646716247,2.27356824875688,8.55744139715597));
#65869=CARTESIAN_POINT('Ctrl Pts',(-7.39494893255526,2.88041017289333,8.53103848636192));
#65870=CARTESIAN_POINT('Ctrl Pts',(-7.14178172006194,3.46076605949351,8.50098841716276));
#65871=CARTESIAN_POINT('Ctrl Pts',(-6.78930611493616,4.06122111193233,8.46861726726607));
#65872=CARTESIAN_POINT('Ctrl Pts',(-6.75551486324552,4.11718514032574,8.4655848389041));
#65873=CARTESIAN_POINT('Ctrl Pts',(-6.69032316780531,4.2221898212127,8.45987102659698));
#65874=CARTESIAN_POINT('Ctrl Pts',(-6.65906731570989,4.27131520287284,8.45718768349993));
#65875=CARTESIAN_POINT('Ctrl Pts',(-6.55894981573849,4.42490127654341,8.44877142898938));
#65876=CARTESIAN_POINT('Ctrl Pts',(-6.48814977801939,4.52807771686597,8.44307795031505));
#65877=CARTESIAN_POINT('Ctrl Pts',(-6.17375540666743,4.96371945335501,8.41892192422169));
#65878=CARTESIAN_POINT('Ctrl Pts',(-5.90681704168521,5.27857445365528,8.40121017526256));
#65879=CARTESIAN_POINT('Ctrl Pts',(-5.6038122881104,5.5840428638979,8.38382601181636));
#65880=CARTESIAN_POINT('Ctrl Pts',(-5.59105566449164,5.59681547208216,8.38309863132567));
#65881=CARTESIAN_POINT('Ctrl Pts',(-5.5725244527013,5.61524332025531,8.38204844792172));
#65882=CARTESIAN_POINT('Ctrl Pts',(-5.56678478686352,5.62093350422191,8.38172406678175));
#65883=CARTESIAN_POINT('Ctrl Pts',(-5.55675804883858,5.63084338008546,8.38115894861103));
#65884=CARTESIAN_POINT('Ctrl Pts',(-5.55247487036598,5.63506699148698,8.3809180353069));
#65885=CARTESIAN_POINT('Ctrl Pts',(-5.54419430983004,5.64321378516719,8.38045323002627));
#65886=CARTESIAN_POINT('Ctrl Pts',(-5.54019757168485,5.64713761450091,8.38022930906826));
#65887=CARTESIAN_POINT('Ctrl Pts',(-5.53071810214171,5.6564244091298,8.37969921575778));
#65888=CARTESIAN_POINT('Ctrl Pts',(-5.52523172734549,5.66178365721794,8.37939320963027));
#65889=CARTESIAN_POINT('Ctrl Pts',(-5.50596437987271,5.68054987733145,8.37832133040583));
#65890=CARTESIAN_POINT('Ctrl Pts',(-5.49214228102466,5.69391463169782,8.37755733713394));
#65891=CARTESIAN_POINT('Ctrl Pts',(-5.32278698876308,5.85647588315636,8.36825642986655));
#65892=CARTESIAN_POINT('Ctrl Pts',(-5.1612628419349,5.99931208686304,8.36000377675366));
#65893=CARTESIAN_POINT('Ctrl Pts',(-4.66516204581226,6.40312992346567,8.3362209467074));
#65894=CARTESIAN_POINT('Ctrl Pts',(-4.31521484457735,6.64400151538207,8.32145224818872));
#65895=CARTESIAN_POINT('Ctrl Pts',(-3.75707114934672,6.96539253531888,8.29926001363458));
#65896=CARTESIAN_POINT('Ctrl Pts',(-3.5620160801797,7.0671292925896,8.29172391110682));
#65897=CARTESIAN_POINT('Ctrl Pts',(-3.11522632764545,7.27696407111459,8.27450682254273));
#65898=CARTESIAN_POINT('Ctrl Pts',(-2.8616145661547,7.38037851881212,8.26476429999101));
#65899=CARTESIAN_POINT('Ctrl Pts',(-2.49138092852051,7.50939121013662,8.24996743660681));
#65900=CARTESIAN_POINT('Ctrl Pts',(-2.37873420362238,7.54583057561246,8.24538864031097));
#65901=CARTESIAN_POINT('Ctrl Pts',(-2.24400670352834,7.58609578229227,8.23978811780086));
#65902=CARTESIAN_POINT('Ctrl Pts',(-2.22267818384232,7.59237228928891,8.23889815169648));
#65903=CARTESIAN_POINT('Ctrl Pts',(-2.19434584367898,7.60058024723546,8.23771173906431));
#65904=CARTESIAN_POINT('Ctrl Pts',(-2.18736526461459,7.60259212209678,8.23741909063928));
#65905=CARTESIAN_POINT('Ctrl Pts',(-2.1758968110581,7.60588034600524,8.23693775216939));
#65906=CARTESIAN_POINT('Ctrl Pts',(-2.17141055071119,7.607162348093,8.23674932434889));
#65907=CARTESIAN_POINT('Ctrl Pts',(-2.16271412783194,7.60963913430154,8.23638380382866));
#65908=CARTESIAN_POINT('Ctrl Pts',(-2.15850410188849,7.61083439545462,8.23620673307318));
#65909=CARTESIAN_POINT('Ctrl Pts',(-2.14878100683365,7.61358614591791,8.23579751593458));
#65910=CARTESIAN_POINT('Ctrl Pts',(-2.14326723885183,7.61514014048698,8.23556525656888));
#65911=CARTESIAN_POINT('Ctrl Pts',(-2.12847429791216,7.61929202848718,8.23494159587623));
#65912=CARTESIAN_POINT('Ctrl Pts',(-2.11919207693431,7.62187895417693,8.23454970477561));
#65913=CARTESIAN_POINT('Ctrl Pts',(-2.0540618783678,7.63990236087384,8.23179612460157));
#65914=CARTESIAN_POINT('Ctrl Pts',(-1.99805144706895,7.65474156724469,8.22940847016318));
#65915=CARTESIAN_POINT('Ctrl Pts',(-1.35206344752239,7.81831435710219,8.2016817481281));
#65916=CARTESIAN_POINT('Ctrl Pts',(-0.746993376766655,7.89912069534865,
8.17408137396201));
#65917=CARTESIAN_POINT('Ctrl Pts',(0.163515756134235,7.91508183977154,8.13400391078272));
#65918=CARTESIAN_POINT('Ctrl Pts',(0.465755618220304,7.90305921801159,8.12090484267445));
#65919=CARTESIAN_POINT('Ctrl Pts',(0.91591458075945,7.85923240971991,8.10182484749996));
#65920=CARTESIAN_POINT('Ctrl Pts',(1.06480982682816,7.8404474255024,8.09558244888485));
#65921=CARTESIAN_POINT('Ctrl Pts',(1.29560376783461,7.80463357671714,8.08600515604046));
#65922=CARTESIAN_POINT('Ctrl Pts',(1.37791608591314,7.79052257714193,8.08260896460322));
#65923=CARTESIAN_POINT('Ctrl Pts',(1.47869669300443,7.77159824890433,8.07847200904348));
#65924=CARTESIAN_POINT('Ctrl Pts',(1.49739000352375,7.76801817930019,8.07770556191647));
#65925=CARTESIAN_POINT('Ctrl Pts',(1.52494814395747,7.76263717945895,8.07657692017905));
#65926=CARTESIAN_POINT('Ctrl Pts',(1.53382305243678,7.76088845854323,8.07621364400052));
#65927=CARTESIAN_POINT('Ctrl Pts',(1.55102784302016,7.75746774483151,8.07550977210399));
#65928=CARTESIAN_POINT('Ctrl Pts',(1.55935806730456,7.75579754765237,8.0751691397102));
#65929=CARTESIAN_POINT('Ctrl Pts',(1.5764696628885,7.75233801609144,8.07446976777318));
#65930=CARTESIAN_POINT('Ctrl Pts',(1.58525072100077,7.75054717202455,8.07411106014527));
#65931=CARTESIAN_POINT('Ctrl Pts',(1.60627968801366,7.74622120787136,8.07325246477966));
#65932=CARTESIAN_POINT('Ctrl Pts',(1.61852467619761,7.74367195270736,8.07275287096891));
#65933=CARTESIAN_POINT('Ctrl Pts',(1.65576251266275,7.73582731078088,8.07123465667474));
#65934=CARTESIAN_POINT('Ctrl Pts',(1.68073587378208,7.73043987192592,8.07021796221002));
#65935=CARTESIAN_POINT('Ctrl Pts',(1.96176477363138,7.66838803904843,8.0587933920971));
#65936=CARTESIAN_POINT('Ctrl Pts',(2.21488403218841,7.59914437091114,8.04866522825797));
#65937=CARTESIAN_POINT('Ctrl Pts',(2.83684592915637,7.39527472089752,8.0239755458874));
#65938=CARTESIAN_POINT('Ctrl Pts',(3.19999003836993,7.24554065522871,8.00975853284183));
#65939=CARTESIAN_POINT('Ctrl Pts',(3.83226704636499,6.92799005811155,7.98417475481596));
#65940=CARTESIAN_POINT('Ctrl Pts',(4.10528376745843,6.76978218201824,7.97280843355973));
#65941=CARTESIAN_POINT('Ctrl Pts',(4.524343642968,6.49225265196611,7.95399458963835));
#65942=CARTESIAN_POINT('Ctrl Pts',(4.67683302577009,6.38327945724006,7.94683078210738));
#65943=CARTESIAN_POINT('Ctrl Pts',(4.85198578698879,6.24846290926921,7.93806446732156));
#65944=CARTESIAN_POINT('Ctrl Pts',(4.87853720774578,6.22775476960711,7.9367204309245));
#65945=CARTESIAN_POINT('Ctrl Pts',(4.91157533751003,6.20164654719234,7.93502801022562));
#65946=CARTESIAN_POINT('Ctrl Pts',(4.91818695243797,6.19640454557412,7.93468831109778));
#65947=CARTESIAN_POINT('Ctrl Pts',(4.92864675021852,6.1880842347254,7.9341492729188));
#65948=CARTESIAN_POINT('Ctrl Pts',(4.93250047685226,6.18501288035744,7.93395032399543));
#65949=CARTESIAN_POINT('Ctrl Pts',(4.93972326643218,6.17924539655191,7.93357678553511));
#65950=CARTESIAN_POINT('Ctrl Pts',(4.94309299961681,6.17655010639183,7.93340224365291));
#65951=CARTESIAN_POINT('Ctrl Pts',(4.95062267914803,6.17051736343863,7.93301162011654));
#65952=CARTESIAN_POINT('Ctrl Pts',(4.95478145807877,6.16717845909347,7.93279545518975));
#65953=CARTESIAN_POINT('Ctrl Pts',(4.96526805247362,6.15874177051359,7.93224932342807));
#65954=CARTESIAN_POINT('Ctrl Pts',(4.97159138449121,6.15363844677584,7.93191903472614));
#65955=CARTESIAN_POINT('Ctrl Pts',(5.00532151805875,6.12633019788134,7.93015192034964));
#65956=CARTESIAN_POINT('Ctrl Pts',(5.03258710438046,6.103952175792,7.92870484104854));
#65957=CARTESIAN_POINT('Ctrl Pts',(5.4392996066812,5.76556851714933,7.90682426751278));
#65958=CARTESIAN_POINT('Ctrl Pts',(5.78844946786801,5.41493286596525,7.8841274704591));
#65959=CARTESIAN_POINT('Ctrl Pts',(6.30597278406671,4.78756397113375,7.84663887023609));
#65960=CARTESIAN_POINT('Ctrl Pts',(6.4942248692803,4.52892029569258,7.83190454295929));
#65961=CARTESIAN_POINT('Ctrl Pts',(6.84390426293828,3.98166718509391,7.80276521183197));
#65962=CARTESIAN_POINT('Ctrl Pts',(7.00394690589092,3.69289314831301,7.78841660649541));
#65963=CARTESIAN_POINT('Ctrl Pts',(7.16839311585861,3.3467753782507,7.77250025044536));
#65964=CARTESIAN_POINT('Ctrl Pts',(7.19079270161591,3.29837320010106,7.77030188466864));
#65965=CARTESIAN_POINT('Ctrl Pts',(7.23367884508027,3.2031888997531,7.76603192031594));
#65966=CARTESIAN_POINT('Ctrl Pts',(7.25420521718807,3.15642765774219,7.76395900688133));
#65967=CARTESIAN_POINT('Ctrl Pts',(7.27897985240022,3.0984700137937,7.76141991328677));
#65968=CARTESIAN_POINT('Ctrl Pts',(7.28365711946097,3.08745900147985,7.76093886117387));
#65969=CARTESIAN_POINT('Ctrl Pts',(7.29097103463763,3.07013179145667,7.76018395424569));
#65970=CARTESIAN_POINT('Ctrl Pts',(7.29362448407297,3.0638227315688,7.75990951742222));
#65971=CARTESIAN_POINT('Ctrl Pts',(7.2983236661073,3.0526088689214,7.75942249718236));
#65972=CARTESIAN_POINT('Ctrl Pts',(7.30037264874885,3.04770543711758,7.75920980130275));
#65973=CARTESIAN_POINT('Ctrl Pts',(7.30473604574677,3.03723371905589,7.75875612642902));
#65974=CARTESIAN_POINT('Ctrl Pts',(7.30704903818827,3.0316648422801,7.75851519673983));
#65975=CARTESIAN_POINT('Ctrl Pts',(7.31368417655183,3.0156380443322,7.75782278194854));
#65976=CARTESIAN_POINT('Ctrl Pts',(7.31799026257383,3.00517346704651,7.7573718523875));
#65977=CARTESIAN_POINT('Ctrl Pts',(7.33673571501738,2.95933937591365,7.75540194126166));
#65978=CARTESIAN_POINT('Ctrl Pts',(7.35094133533399,2.92387448970292,7.75389103712112));
#65979=CARTESIAN_POINT('Ctrl Pts',(7.5620322506461,2.38561422750803,7.73115787573218));
#65980=CARTESIAN_POINT('Ctrl Pts',(7.70719697583827,1.86405079231759,7.7118797281732));
#65981=CARTESIAN_POINT('Ctrl Pts',(7.86646791400167,0.931407599437989,7.67940979006949));
#65982=CARTESIAN_POINT('Ctrl Pts',(7.90390263768989,0.526446351861149,7.66590036787826));
#65983=CARTESIAN_POINT('Ctrl Pts',(7.91262224721879,-0.0463581511342715,
7.64591947725558));
#65984=CARTESIAN_POINT('Ctrl Pts',(7.9098860977543,-0.213162061307259,7.63999209352008));
#65985=CARTESIAN_POINT('Ctrl Pts',(7.8936979611195,-0.550007916894117,7.62760144786612));
#65986=CARTESIAN_POINT('Ctrl Pts',(7.88001543409475,-0.719948806275036,
7.62113232594531));
#65987=CARTESIAN_POINT('Ctrl Pts',(7.85816077260593,-0.913129314617089,
7.61340312474966));
#65988=CARTESIAN_POINT('Ctrl Pts',(7.8553572149372,-0.936941233684731,7.61244386459863));
#65989=CARTESIAN_POINT('Ctrl Pts',(7.85169101467516,-0.966906306303083,
7.61122809659573));
#65990=CARTESIAN_POINT('Ctrl Pts',(7.85092928579957,-0.973071911035898,
7.61097748014946));
#65991=CARTESIAN_POINT('Ctrl Pts',(7.84970641544429,-0.982875188773056,
7.61057826058596));
#65992=CARTESIAN_POINT('Ctrl Pts',(7.84925000441222,-0.9865134634709,7.61042993651213));
#65993=CARTESIAN_POINT('Ctrl Pts',(7.84838296473613,-0.99338636503417,7.61014943560255));
#65994=CARTESIAN_POINT('Ctrl Pts',(7.84797286655356,-0.99662104993463,7.61001729077698));
#65995=CARTESIAN_POINT('Ctrl Pts',(7.8470405120942,-1.00393881580851,7.60971805183827));
#65996=CARTESIAN_POINT('Ctrl Pts',(7.84651706888449,-1.00802174179599,7.60955088788374));
#65997=CARTESIAN_POINT('Ctrl Pts',(7.84516621765225,-1.01849375181251,7.60912161983706));
#65998=CARTESIAN_POINT('Ctrl Pts',(7.84433419284816,-1.02488222518112,7.6088592463545));
#65999=CARTESIAN_POINT('Ctrl Pts',(7.83950938961043,-1.06157807558204,7.60734932592833));
#66000=CARTESIAN_POINT('Ctrl Pts',(7.83534882271064,-1.09186274666821,7.60609212004813));
#66001=CARTESIAN_POINT('Ctrl Pts',(7.76527231781697,-1.58090934348024,7.58562018664586));
#66002=CARTESIAN_POINT('Ctrl Pts',(7.65934622298113,-2.03299577745273,7.56432048276451));
#66003=CARTESIAN_POINT('Ctrl Pts',(7.42154091190563,-2.75554484602005,7.52911039680101));
#66004=CARTESIAN_POINT('Ctrl Pts',(7.31275807224921,-3.03247020277189,7.51530509923572));
#66005=CARTESIAN_POINT('Ctrl Pts',(7.07222674984201,-3.55602244542797,7.4891368304081));
#66006=CARTESIAN_POINT('Ctrl Pts',(6.94248527659778,-3.80310448702041,7.47675485164227));
#66007=CARTESIAN_POINT('Ctrl Pts',(6.72923071275136,-4.16179392610184,7.45888440052028));
#66008=CARTESIAN_POINT('Ctrl Pts',(6.65539287671006,-4.27888103919119,7.45306665618013));
#66009=CARTESIAN_POINT('Ctrl Pts',(6.53699824154604,-4.45613769102088,7.44428469662259));
#66010=CARTESIAN_POINT('Ctrl Pts',(6.49459830995342,-4.51770985548721,7.44123894550398));
#66011=CARTESIAN_POINT('Ctrl Pts',(6.44334450773971,-4.58992624971152,7.4376713101261));
#66012=CARTESIAN_POINT('Ctrl Pts',(6.43532833567487,-4.60115861907106,7.43711654157955));
#66013=CARTESIAN_POINT('Ctrl Pts',(6.4230807990294,-4.61822541587162,7.43627380038086));
#66014=CARTESIAN_POINT('Ctrl Pts',(6.41887080351395,-4.6240751022041,7.43598498299026));
#66015=CARTESIAN_POINT('Ctrl Pts',(6.41154961035063,-4.63421845718184,7.43548423097848));
#66016=CARTESIAN_POINT('Ctrl Pts',(6.40844208244668,-4.63851476131563,7.43527215109287));
#66017=CARTESIAN_POINT('Ctrl Pts',(6.40196972703011,-4.64744417953311,7.43483140140609));
#66018=CARTESIAN_POINT('Ctrl Pts',(6.39860418325591,-4.65207677214078,7.43460276023524));
#66019=CARTESIAN_POINT('Ctrl Pts',(6.38937233023096,-4.66475523205794,7.4339770697975));
#66020=CARTESIAN_POINT('Ctrl Pts',(6.38349584602102,-4.67279369693589,7.43358042561094));
#66021=CARTESIAN_POINT('Ctrl Pts',(6.36096424233352,-4.70349293709222,7.43206583789562));
#66022=CARTESIAN_POINT('Ctrl Pts',(6.34420341297114,-4.72607606557458,7.43095211592028));
#66023=CARTESIAN_POINT('Ctrl Pts',(6.07855565993108,-5.08004350379971,7.41350126157916));
#66024=CARTESIAN_POINT('Ctrl Pts',(5.80411864030804,-5.39146879504295,7.39827663107649));
#66025=CARTESIAN_POINT('Ctrl Pts',(5.14622568717159,-6.0292696252545,7.3660095330975));
#66026=CARTESIAN_POINT('Ctrl Pts',(4.75353722307944,-6.34346828974936,7.34935014834362));
#66027=CARTESIAN_POINT('Ctrl Pts',(4.13846064785114,-6.74622506733091,7.32352948275121));
#66028=CARTESIAN_POINT('Ctrl Pts',(3.93762125777047,-6.86538681493492,7.31512043375686));
#66029=CARTESIAN_POINT('Ctrl Pts',(3.63637664995337,-7.0265498410981,7.30212492202932));
#66030=CARTESIAN_POINT('Ctrl Pts',(3.5398987143048,-7.07564505802181,7.29790769161243));
#66031=CARTESIAN_POINT('Ctrl Pts',(3.43419631081239,-7.12673141724409,7.2931959927669));
#66032=CARTESIAN_POINT('Ctrl Pts',(3.42593774283983,-7.13070512472645,7.29282726863415));
#66033=CARTESIAN_POINT('Ctrl Pts',(3.41374762366139,-7.13654447892173,7.29228210394887));
#66034=CARTESIAN_POINT('Ctrl Pts',(3.40982138858437,-7.13842125651517,7.29210637706188));
#66035=CARTESIAN_POINT('Ctrl Pts',(3.40312566407425,-7.14161509178855,7.29180646271214));
#66036=CARTESIAN_POINT('Ctrl Pts',(3.40035694879235,-7.14293378280346,7.29168237874522));
#66037=CARTESIAN_POINT('Ctrl Pts',(3.39470754023777,-7.14562046893532,7.29142905501253));
#66038=CARTESIAN_POINT('Ctrl Pts',(3.39182678710229,-7.14698833188202,7.29129980708599));
#66039=CARTESIAN_POINT('Ctrl Pts',(3.38497603078409,-7.15023618955032,7.29099226938482));
#66040=CARTESIAN_POINT('Ctrl Pts',(3.3810052911652,-7.15211461851389,7.29081388182533));
#66041=CARTESIAN_POINT('Ctrl Pts',(3.36908528655124,-7.15774144359293,7.29027796368081));
#66042=CARTESIAN_POINT('Ctrl Pts',(3.36113136277975,-7.16147988912177,7.28991981779205));
#66043=CARTESIAN_POINT('Ctrl Pts',(3.28487925283945,-7.19716433657516,7.28648131511179));
#66044=CARTESIAN_POINT('Ctrl Pts',(3.21613584699936,-7.2281446943565,7.28334261282636));
#66045=CARTESIAN_POINT('Ctrl Pts',(2.75001866550971,-7.43024245417687,7.2618547921381));
#66046=CARTESIAN_POINT('Ctrl Pts',(2.33965115898892,-7.5694839270577,7.24197358517235));
#66047=CARTESIAN_POINT('Ctrl Pts',(1.42928893271001,-7.79723787145641,7.19864974593833));
#66048=CARTESIAN_POINT('Ctrl Pts',(0.927892356212872,-7.87266721608372,
7.17532035901489));
#66049=CARTESIAN_POINT('Ctrl Pts',(0.18230046849807,-7.91256240755643,7.14290499246501));
#66050=CARTESIAN_POINT('Ctrl Pts',(-0.0585698784159418,-7.91444629599931,
7.13276054190036));
#66051=CARTESIAN_POINT('Ctrl Pts',(-0.324829722659474,-7.90437006971546,
7.12191139033257));
#66052=CARTESIAN_POINT('Ctrl Pts',(-0.350488286076147,-7.90327391181675,
7.12086957961653));
#66053=CARTESIAN_POINT('Ctrl Pts',(-0.395192057562846,-7.90114599248355,
7.11906082405882));
#66054=CARTESIAN_POINT('Ctrl Pts',(-0.414239641911428,-7.90017026921181,
7.11829214960519));
#66055=CARTESIAN_POINT('Ctrl Pts',(-0.441769593808843,-7.89866019365127,
7.11718403722202));
#66056=CARTESIAN_POINT('Ctrl Pts',(-0.450254850499073,-7.89818104369389,
7.11684289036724));
#66057=CARTESIAN_POINT('Ctrl Pts',(-0.464962902089955,-7.89732672257769,
7.11625223849874));
#66058=CARTESIAN_POINT('Ctrl Pts',(-0.471186047924912,-7.89695786818719,
7.1160025380797));
#66059=CARTESIAN_POINT('Ctrl Pts',(-0.483138517865475,-7.8962352499575,
7.11552335556403));
#66060=CARTESIAN_POINT('Ctrl Pts',(-0.488867903856261,-7.89588260569163,
7.11529383898065));
#66061=CARTESIAN_POINT('Ctrl Pts',(-0.502343938871402,-7.89503843049926,
7.11475441303453));
#66062=CARTESIAN_POINT('Ctrl Pts',(-0.510090265005628,-7.89454173299364,
7.11444466379778));
#66063=CARTESIAN_POINT('Ctrl Pts',(-0.536763249935253,-7.89279202824524,
7.11337921440185));
#66064=CARTESIAN_POINT('Ctrl Pts',(-0.555686193364753,-7.89148234797809,
7.1126252691143));
#66065=CARTESIAN_POINT('Ctrl Pts',(-0.762587658718213,-7.87641455317025,
7.10440250932966));
#66066=CARTESIAN_POINT('Ctrl Pts',(-0.950027801780292,-7.8560103739309,
7.0971431839287));
#66067=CARTESIAN_POINT('Ctrl Pts',(-1.29009060629585,-7.80664159572602,
7.08424311733428));
#66068=CARTESIAN_POINT('Ctrl Pts',(-1.44292741037141,-7.77984252840712,
7.07854569161725));
#66069=CARTESIAN_POINT('Ctrl Pts',(-2.20016694196386,-7.62398048251643,
7.05063645513779));
#66070=CARTESIAN_POINT('Ctrl Pts',(-2.78872370337274,-7.42891439450698,
7.03015134615013));
#66071=CARTESIAN_POINT('Ctrl Pts',(-3.44521394135837,-7.12220490875548,
7.004144308134));
#66072=CARTESIAN_POINT('Ctrl Pts',(-3.54094160453842,-7.07509953283296,
7.00026228163398));
#66073=CARTESIAN_POINT('Ctrl Pts',(-3.74785418237849,-6.96803134782176,
6.99161641703096));
#66074=CARTESIAN_POINT('Ctrl Pts',(-3.85861301536865,-6.90731315259118,
6.98682298630535));
#66075=CARTESIAN_POINT('Ctrl Pts',(-4.01474589726591,-6.81679343589915,
6.9797623386975));
#66076=CARTESIAN_POINT('Ctrl Pts',(-4.06134383345277,-6.78913421493755,
6.97761542655229));
#66077=CARTESIAN_POINT('Ctrl Pts',(-4.11472255728099,-6.75670390827992,
6.97510596640457));
#66078=CARTESIAN_POINT('Ctrl Pts',(-4.12178539476263,-6.75239769164559,
6.97477290566087));
#66079=CARTESIAN_POINT('Ctrl Pts',(-4.13247418609869,-6.74585770962509,
6.97426729047583));
#66080=CARTESIAN_POINT('Ctrl Pts',(-4.13610512939409,-6.74363207001609,
6.97409526055397));
#66081=CARTESIAN_POINT('Ctrl Pts',(-4.1426642050995,-6.73960429887846,6.97378399993207));
#66082=CARTESIAN_POINT('Ctrl Pts',(-4.14559295448717,-6.73780319372323,
6.9736448360087));
#66083=CARTESIAN_POINT('Ctrl Pts',(-4.15189385609066,-6.73392263863843,
6.97334505037147));
#66084=CARTESIAN_POINT('Ctrl Pts',(-4.15526560547604,-6.73184257415849,
6.97318438892134));
#66085=CARTESIAN_POINT('Ctrl Pts',(-4.16435200880427,-6.72622765740883,
6.97275078507602));
#66086=CARTESIAN_POINT('Ctrl Pts',(-4.1700637133671,-6.72268806196385,6.97247753546295));
#66087=CARTESIAN_POINT('Ctrl Pts',(-4.19638147682942,-6.70633225887918,
6.97121534363996));
#66088=CARTESIAN_POINT('Ctrl Pts',(-4.21693281919563,-6.69342867598355,
6.97022081350512));
#66089=CARTESIAN_POINT('Ctrl Pts',(-4.54489276868713,-6.4854023565472,6.95421158154743));
#66090=CARTESIAN_POINT('Ctrl Pts',(-4.83850588341102,-6.26939466798868,
6.93794134598426));
#66091=CARTESIAN_POINT('Ctrl Pts',(-5.56255141416055,-5.65547924242552,
6.89467056812326));
#66092=CARTESIAN_POINT('Ctrl Pts',(-5.96560570703009,-5.22858421540378,
6.86742087018337));
#66093=CARTESIAN_POINT('Ctrl Pts',(-6.4863507765081,-4.53756879106466,6.82978984664789));
#66094=CARTESIAN_POINT('Ctrl Pts',(-6.64284250436611,-4.30522253935676,
6.81801894587401));
#66095=CARTESIAN_POINT('Ctrl Pts',(-6.79586806638635,-4.04974278978103,
6.80599024775713));
#66096=CARTESIAN_POINT('Ctrl Pts',(-6.80498582709915,-4.03440297162688,
6.80527134013262));
#66097=CARTESIAN_POINT('Ctrl Pts',(-6.81821431821871,-4.01197478160315,
6.80422506498984));
#66098=CARTESIAN_POINT('Ctrl Pts',(-6.8223660321924,-4.00491071819191,6.80389622317893));
#66099=CARTESIAN_POINT('Ctrl Pts',(-6.82963139472718,-3.99250475796903,
6.80331992733872));
#66100=CARTESIAN_POINT('Ctrl Pts',(-6.83274976585024,-3.98716564337876,
6.80307230379194));
#66101=CARTESIAN_POINT('Ctrl Pts',(-6.83879076757475,-3.97679465131281,
6.80259207107961));
#66102=CARTESIAN_POINT('Ctrl Pts',(-6.84171411123687,-3.97176319556593,
6.80235943643488));
#66103=CARTESIAN_POINT('Ctrl Pts',(-6.84867647494627,-3.95974956351787,
6.80180480380491));
#66104=CARTESIAN_POINT('Ctrl Pts',(-6.8527103767237,-3.95276441968311,6.80148298924659));
#66105=CARTESIAN_POINT('Ctrl Pts',(-6.86485964847448,-3.93165212620949,
6.80051232926105));
#66106=CARTESIAN_POINT('Ctrl Pts',(-6.87294209043584,-3.91750602556343,
6.79986466113227));
#66107=CARTESIAN_POINT('Ctrl Pts',(-6.95369601770744,-3.77514924013578,
6.79337402167086));
#66108=CARTESIAN_POINT('Ctrl Pts',(-7.02281711840131,-3.64495303543774,
6.78765862509866));
#66109=CARTESIAN_POINT('Ctrl Pts',(-7.11824231190146,-3.45240573578784,
6.77949794533659));
#66110=CARTESIAN_POINT('Ctrl Pts',(-7.14744630711651,-3.39153217702231,
6.77695922614847));
#66111=CARTESIAN_POINT('Ctrl Pts',(-7.46176102839755,-2.71426984332509,
6.74914170098844));
#66112=CARTESIAN_POINT('Ctrl Pts',(-7.6671252487402,-2.06404914908849,6.72663812453134));
#66113=CARTESIAN_POINT('Ctrl Pts',(-7.82376566730491,-1.19004905646277,
6.69562366334662));
#66114=CARTESIAN_POINT('Ctrl Pts',(-7.85244955238754,-0.983135444346683,
6.68820075373254));
#66115=CARTESIAN_POINT('Ctrl Pts',(-7.88874576839007,-0.61457782966774,
6.67449659629814));
#66116=CARTESIAN_POINT('Ctrl Pts',(-7.89964926935827,-0.453378014245832,
6.66833997739062));
#66117=CARTESIAN_POINT('Ctrl Pts',(-7.90648316265765,-0.268335920070195,
6.66097868722274));
#66118=CARTESIAN_POINT('Ctrl Pts',(-7.90724991391673,-0.244701745842623,
6.66003298460298));
#66119=CARTESIAN_POINT('Ctrl Pts',(-7.90808784598529,-0.214727302504374,
6.65882623507));
#66120=CARTESIAN_POINT('Ctrl Pts',(-7.90825738900562,-0.208389690394877,
6.65857067098738));
#66121=CARTESIAN_POINT('Ctrl Pts',(-7.90851595994916,-0.198269085449415,
6.65816188371518));
#66122=CARTESIAN_POINT('Ctrl Pts',(-7.90860989258907,-0.194486209701014,
6.65800893699114));
#66123=CARTESIAN_POINT('Ctrl Pts',(-7.90878219758714,-0.187340507902215,
6.65771974035148));
#66124=CARTESIAN_POINT('Ctrl Pts',(-7.90886113940516,-0.183977695150078,
6.65758352277971));
#66125=CARTESIAN_POINT('Ctrl Pts',(-7.90903436488574,-0.17639232957355,
6.65727598997111));
#66126=CARTESIAN_POINT('Ctrl Pts',(-7.90912741173672,-0.172169752447682,
6.65710460418133));
#66127=CARTESIAN_POINT('Ctrl Pts',(-7.90939154332332,-0.159730871858649,
6.65659917005622));
#66128=CARTESIAN_POINT('Ctrl Pts',(-7.90955320593334,-0.151514415141959,
6.65626457951751));
#66129=CARTESIAN_POINT('Ctrl Pts',(-7.91055658713074,-0.0961301159729605,
6.65400438583313));
#66130=CARTESIAN_POINT('Ctrl Pts',(-7.91098916588274,-0.0489566925479483,
6.65205564367597));
#66131=CARTESIAN_POINT('Ctrl Pts',(-7.91102344790239,0.103134037520468,
6.64570318947202));
#66132=CARTESIAN_POINT('Ctrl Pts',(-7.90895994131844,0.208037490304112,
6.64121498214525));
#66133=CARTESIAN_POINT('Ctrl Pts',(-7.89734454701748,0.50151101491396,6.62842160014599));
#66134=CARTESIAN_POINT('Ctrl Pts',(-7.88312778758773,0.689821860973479,
6.61993882411635));
#66135=CARTESIAN_POINT('Ctrl Pts',(-7.76369551942669,1.75998621118394,6.57083169253472));
#66136=CARTESIAN_POINT('Ctrl Pts',(-7.51724645926729,2.61997199051387,6.52885975577479));
#66137=CARTESIAN_POINT('Ctrl Pts',(-7.10957271997544,3.46999187554645,6.49027534514519));
#66138=CARTESIAN_POINT('Ctrl Pts',(-7.08559408268638,3.51869642489519,6.48807148846915));
#66139=CARTESIAN_POINT('Ctrl Pts',(-7.05590584847955,3.57746378792904,6.4854203244357));
#66140=CARTESIAN_POINT('Ctrl Pts',(-7.05067339831071,3.58776519973336,6.48495589902699));
#66141=CARTESIAN_POINT('Ctrl Pts',(-7.04204949574865,3.60465182299889,6.48419507458754));
#66142=CARTESIAN_POINT('Ctrl Pts',(-7.03867133844764,3.61124378231878,6.48389819673668));
#66143=CARTESIAN_POINT('Ctrl Pts',(-7.03259413603216,3.623061593723,6.48336618210451));
#66144=CARTESIAN_POINT('Ctrl Pts',(-7.02989851402985,3.62828919419385,6.48313092197821));
#66145=CARTESIAN_POINT('Ctrl Pts',(-7.02416628167898,3.63937530219927,6.4826321689708));
#66146=CARTESIAN_POINT('Ctrl Pts',(-7.02112816522473,3.64523302831263,6.48236873079233));
#66147=CARTESIAN_POINT('Ctrl Pts',(-7.01299910361643,3.66085862898465,6.48166625555504));
#66148=CARTESIAN_POINT('Ctrl Pts',(-7.00789507253669,3.67061970004345,6.4812276926898));
#66149=CARTESIAN_POINT('Ctrl Pts',(-6.98384590010682,3.71637891289789,6.47917295105448));
#66150=CARTESIAN_POINT('Ctrl Pts',(-6.96464350685349,3.75224155238918,6.4775661239629));
#66151=CARTESIAN_POINT('Ctrl Pts',(-6.8177594581398,4.02155151523423,6.46552419682136));
#66152=CARTESIAN_POINT('Ctrl Pts',(-6.6786449454492,4.24858063965722,6.45552117709732));
#66153=CARTESIAN_POINT('Ctrl Pts',(-6.24096730423131,4.88806012939086,6.42737479122158));
#66154=CARTESIAN_POINT('Ctrl Pts',(-5.91374514936757,5.2792452545901,6.41026666768018));
#66155=CARTESIAN_POINT('Ctrl Pts',(-5.23416753709721,5.94856819957873,6.37746628043565));
#66156=CARTESIAN_POINT('Ctrl Pts',(-4.8913456869406,6.23350829206073,6.3618823575361));
#66157=CARTESIAN_POINT('Ctrl Pts',(-4.50322756710697,6.50428039620954,6.34312301587694));
#66158=CARTESIAN_POINT('Ctrl Pts',(-4.47992979496336,6.52034899275809,6.34199284329726));
#66159=CARTESIAN_POINT('Ctrl Pts',(-4.45136932705794,6.53982196841356,6.34060174153448));
#66160=CARTESIAN_POINT('Ctrl Pts',(-4.4461878927256,6.54334574102412,6.34034914273798));
#66161=CARTESIAN_POINT('Ctrl Pts',(-4.43764100856011,6.5491434383596,6.3399320949884));
#66162=CARTESIAN_POINT('Ctrl Pts',(-4.43427797698291,6.5514209389849,6.33976789787987));
#66163=CARTESIAN_POINT('Ctrl Pts',(-4.42821645607803,6.55551909575341,6.33947177189199));
#66164=CARTESIAN_POINT('Ctrl Pts',(-4.42551859195046,6.55734067964341,6.33933990877247));
#66165=CARTESIAN_POINT('Ctrl Pts',(-4.41974936168588,6.56123085192514,6.33905779005097));
#66166=CARTESIAN_POINT('Ctrl Pts',(-4.41667767387697,6.56329894468278,6.33890749967426));
#66167=CARTESIAN_POINT('Ctrl Pts',(-4.40831325910088,6.56892197093703,6.33849802512201));
#66168=CARTESIAN_POINT('Ctrl Pts',(-4.40301769180088,6.57247265919341,6.33823854066548));
#66169=CARTESIAN_POINT('Ctrl Pts',(-4.37620879031418,6.59040113868457,6.33692369092501));
#66170=CARTESIAN_POINT('Ctrl Pts',(-4.3546295283039,6.60467956723946,6.33586140936924));
#66171=CARTESIAN_POINT('Ctrl Pts',(-4.1636277665221,6.72971741569367,6.32642738100648));
#66172=CARTESIAN_POINT('Ctrl Pts',(-3.99009346743656,6.83403505707336,6.31763871742243));
#66173=CARTESIAN_POINT('Ctrl Pts',(-3.63802423351111,7.02769330109621,6.29968584484765));
#66174=CARTESIAN_POINT('Ctrl Pts',(-3.45971831647988,7.11716494505054,6.29053561573333));
#66175=CARTESIAN_POINT('Ctrl Pts',(-2.74278111754678,7.44360245588153,6.25402064440536));
#66176=CARTESIAN_POINT('Ctrl Pts',(-2.18173738972459,7.62694020339394,6.22621450780322));
#66177=CARTESIAN_POINT('Ctrl Pts',(-1.49565644334698,7.76913922536113,6.19533442674687));
#66178=CARTESIAN_POINT('Ctrl Pts',(-1.38530506027283,7.78957275603625,6.19045365597572));
#66179=CARTESIAN_POINT('Ctrl Pts',(-1.07332300422859,7.84050198934743,6.17690545029293));
#66180=CARTESIAN_POINT('Ctrl Pts',(-0.870889506981382,7.86556124031206,
6.16840922762043));
#66181=CARTESIAN_POINT('Ctrl Pts',(-0.648794529560549,7.88437357916863,
6.1593983861036));
#66182=CARTESIAN_POINT('Ctrl Pts',(-0.629880743417078,7.8859071344546,6.15863344098221));
#66183=CARTESIAN_POINT('Ctrl Pts',(-0.603358397050679,7.88796157440263,
6.15756414342877));
#66184=CARTESIAN_POINT('Ctrl Pts',(-0.595754399091126,7.88853952585184,
6.15725796185806));
#66185=CARTESIAN_POINT('Ctrl Pts',(-0.582575416170867,7.88952204688443,
6.15672796766475));
#66186=CARTESIAN_POINT('Ctrl Pts',(-0.577000822407313,7.88993170407207,
6.15650399215719));
#66187=CARTESIAN_POINT('Ctrl Pts',(-0.565418769516555,7.89077048764221,
6.15603907891336));
#66188=CARTESIAN_POINT('Ctrl Pts',(-0.559411243757319,7.89119866269632,
6.15579817177235));
#66189=CARTESIAN_POINT('Ctrl Pts',(-0.545296992296478,7.89218843061656,
6.15523273932184));
#66190=CARTESIAN_POINT('Ctrl Pts',(-0.537189871659079,7.89274439447207,
6.15490839431645));
#66191=CARTESIAN_POINT('Ctrl Pts',(-0.511234745258356,7.89448414951912,
6.15387138250419));
#66192=CARTESIAN_POINT('Ctrl Pts',(-0.493383516506788,7.89561990364859,
6.15316025162415));
#66193=CARTESIAN_POINT('Ctrl Pts',(-0.451659946713336,7.89813244171489,
6.15150297207179));
#66194=CARTESIAN_POINT('Ctrl Pts',(-0.427784855312348,7.89946155790637,
6.15055834497181));
#66195=CARTESIAN_POINT('Ctrl Pts',(-0.185309265694481,7.91185755709024,
6.14100162603336));
#66196=CARTESIAN_POINT('Ctrl Pts',(0.033662794855598,7.91395634601143,6.13267970517584));
#66197=CARTESIAN_POINT('Ctrl Pts',(0.749017906919613,7.89111670623702,6.10625032271572));
#66198=CARTESIAN_POINT('Ctrl Pts',(1.24300245222186,7.82851947334889,6.08926480322795));
#66199=CARTESIAN_POINT('Ctrl Pts',(2.0430668001165,7.64945351220834,6.06101556156691));
#66200=CARTESIAN_POINT('Ctrl Pts',(2.35365483102663,7.55966607977866,6.04982963553433));
#66201=CARTESIAN_POINT('Ctrl Pts',(2.84775816177783,7.3834165937122,6.03057518549417));
#66202=CARTESIAN_POINT('Ctrl Pts',(3.03498640570151,7.30844897378979,6.02291021662726));
#66203=CARTESIAN_POINT('Ctrl Pts',(3.23225750486438,7.22057049262203,6.01426989212432));
#66204=CARTESIAN_POINT('Ctrl Pts',(3.24534636538813,7.214697067876,6.01369409370674));
#66205=CARTESIAN_POINT('Ctrl Pts',(3.26356614932882,7.20646160702582,6.01288913612258));
#66206=CARTESIAN_POINT('Ctrl Pts',(3.26871068462162,7.204129604927,6.01266146508798));
#66207=CARTESIAN_POINT('Ctrl Pts',(3.27758437254653,7.20009572740804,6.012268104008));
#66208=CARTESIAN_POINT('Ctrl Pts',(3.2813147124833,7.19839645758281,6.01210254152987));
#66209=CARTESIAN_POINT('Ctrl Pts',(3.28862764790719,7.19505835377466,6.01177758276833));
#66210=CARTESIAN_POINT('Ctrl Pts',(3.29221034410869,7.19341974104402,6.01161819723236));
#66211=CARTESIAN_POINT('Ctrl Pts',(3.30087138391499,7.18945062767021,6.01123244506941));
#66212=CARTESIAN_POINT('Ctrl Pts',(3.30594848193471,7.18711742323972,6.0110059484111));
#66213=CARTESIAN_POINT('Ctrl Pts',(3.32151743922212,7.17994264747415,6.01031027133182));
#66214=CARTESIAN_POINT('Ctrl Pts',(3.33200113533262,7.17508348050341,6.009840255225));
#66215=CARTESIAN_POINT('Ctrl Pts',(3.44323285405106,7.12323150033678,6.0048370101673));
#66216=CARTESIAN_POINT('Ctrl Pts',(3.5429872951274,7.07414439760871,6.00020718659184));
#66217=CARTESIAN_POINT('Ctrl Pts',(3.8322530047261,6.92414945003292,5.98642274432849));
#66218=CARTESIAN_POINT('Ctrl Pts',(4.01872728951156,6.81761198786974,5.97707687422037));
#66219=CARTESIAN_POINT('Ctrl Pts',(4.90514703219556,6.26216319322926,5.93102501476368));
#66220=CARTESIAN_POINT('Ctrl Pts',(5.53581723435538,5.71229141104296,5.89385793602659));
#66221=CARTESIAN_POINT('Ctrl Pts',(6.10098617330596,5.03630194739823,5.85800112057454));
#66222=CARTESIAN_POINT('Ctrl Pts',(6.1323690200035,4.9980416036641,5.85599719808608));
#66223=CARTESIAN_POINT('Ctrl Pts',(6.17374451740898,4.94662232028513,5.85333715379805));
#66224=CARTESIAN_POINT('Ctrl Pts',(6.18405766507667,4.93372319284318,5.85267259218814));
#66225=CARTESIAN_POINT('Ctrl Pts',(6.20009105885904,4.91354023419417,5.85163700123266));
#66226=CARTESIAN_POINT('Ctrl Pts',(6.20583901581246,4.90627851650074,5.85126525198408));
#66227=CARTESIAN_POINT('Ctrl Pts',(6.21724995299581,4.89181030133763,5.850526262223));
#66228=CARTESIAN_POINT('Ctrl Pts',(6.22291319113226,4.8846040185932,5.8501590147725));
#66229=CARTESIAN_POINT('Ctrl Pts',(6.23548452618911,4.86855006404709,5.84934270250191));
#66230=CARTESIAN_POINT('Ctrl Pts',(6.24238634706428,4.85969749031077,5.84889379989512));
#66231=CARTESIAN_POINT('Ctrl Pts',(6.25667198856353,4.84129346118173,5.84796310739756));
#66232=CARTESIAN_POINT('Ctrl Pts',(6.26405283568117,4.83173973043217,5.84748139482729));
#66233=CARTESIAN_POINT('Ctrl Pts',(6.28299112466769,4.80710977533512,5.84624315873157));
#66234=CARTESIAN_POINT('Ctrl Pts',(6.2945162046897,4.79200872473228,5.84548747163797));
#66235=CARTESIAN_POINT('Ctrl Pts',(6.32780741229175,4.74806068336325,5.84329830717785));
#66236=CARTESIAN_POINT('Ctrl Pts',(6.34943049754676,4.7191057718518,5.84186853036351));
#66237=CARTESIAN_POINT('Ctrl Pts',(6.49042612227705,4.52757870647068,5.83249240352917));
#66238=CARTESIAN_POINT('Ctrl Pts',(6.60374530757276,4.36063674694733,5.82470569087755));
#66239=CARTESIAN_POINT('Ctrl Pts',(6.81375538505173,4.02425478886288,5.80967662482413));
#66240=CARTESIAN_POINT('Ctrl Pts',(6.91080692907022,3.85520943798788,5.80242975799392));
#66241=CARTESIAN_POINT('Ctrl Pts',(7.33824612423678,3.04257640137642,5.76869844499615));
#66242=CARTESIAN_POINT('Ctrl Pts',(7.58554213421754,2.35933032892604,5.74381727703515));
#66243=CARTESIAN_POINT('Ctrl Pts',(7.74404968218386,1.61706515113415,5.71375224029246));
#66244=CARTESIAN_POINT('Ctrl Pts',(7.75129517153371,1.58196974985342,5.71232312961162));
#66245=CARTESIAN_POINT('Ctrl Pts',(7.75989868319961,1.53881776691502,5.71055547441325));
#66246=CARTESIAN_POINT('Ctrl Pts',(7.76148307976106,1.53080635457468,5.7102268566353));
#66247=CARTESIAN_POINT('Ctrl Pts',(7.76408345169298,1.51754989963186,5.70968234354736));
#66248=CARTESIAN_POINT('Ctrl Pts',(7.7651065261497,1.51230624544787,5.70946676469407));
#66249=CARTESIAN_POINT('Ctrl Pts',(7.76686435049282,1.50324790131082,5.70909401439142));
#66250=CARTESIAN_POINT('Ctrl Pts',(7.76760160436761,1.49943369559405,5.70893695579678));
#66251=CARTESIAN_POINT('Ctrl Pts',(7.76923991502855,1.49092421011634,5.70858632310695));
#66252=CARTESIAN_POINT('Ctrl Pts',(7.77013952521912,1.48622865538102,5.70839268341547));
#66253=CARTESIAN_POINT('Ctrl Pts',(7.7724920410848,1.47388907770682,5.70788338675628));
#66254=CARTESIAN_POINT('Ctrl Pts',(7.77393792435386,1.46624373476725,5.70756740831289));
#66255=CARTESIAN_POINT('Ctrl Pts',(7.78030083328137,1.43232483101939,5.70616361034092));
#66256=CARTESIAN_POINT('Ctrl Pts',(7.78509591580113,1.40602881614237,5.70507012487186));
#66257=CARTESIAN_POINT('Ctrl Pts',(7.81772317784502,1.22181720806596,5.69737093919074));
#66258=CARTESIAN_POINT('Ctrl Pts',(7.84087851624784,1.06313023775982,5.69052266048115));
#66259=CARTESIAN_POINT('Ctrl Pts',(7.87075959753136,0.803311390275426,5.67906787879977));
#66260=CARTESIAN_POINT('Ctrl Pts',(7.88039290012531,0.702547185654779,5.67456737271057));
#66261=CARTESIAN_POINT('Ctrl Pts',(7.92853959033575,0.0712849214034552,
5.64611904344095));
#66262=CARTESIAN_POINT('Ctrl Pts',(7.91540312773242,-0.461788922677369,
5.62108359128015));
#66263=CARTESIAN_POINT('Ctrl Pts',(7.79398026758889,-1.42490740654869,5.57730803467653));
#66264=CARTESIAN_POINT('Ctrl Pts',(7.70295655714242,-1.85500137982462,5.55829215853666));
#66265=CARTESIAN_POINT('Ctrl Pts',(7.56818997241208,-2.30375778674544,5.53926796679553));
#66266=CARTESIAN_POINT('Ctrl Pts',(7.5595060046451,-2.33209527885939,5.53806992817338));
#66267=CARTESIAN_POINT('Ctrl Pts',(7.547612705697,-2.37014091472058,5.53646578947383));
#66268=CARTESIAN_POINT('Ctrl Pts',(7.54454356268742,-2.37989242248096,5.53605501548854));
#66269=CARTESIAN_POINT('Ctrl Pts',(7.53970050021364,-2.39517663730959,5.53541177923968));
#66270=CARTESIAN_POINT('Ctrl Pts',(7.53793937862533,-2.40071336922869,5.53517888914768));
#66271=CARTESIAN_POINT('Ctrl Pts',(7.53454859079476,-2.41133303897929,5.53473243237383));
#66272=CARTESIAN_POINT('Ctrl Pts',(7.5329198769411,-2.41641627615211,5.53451883394969));
#66273=CARTESIAN_POINT('Ctrl Pts',(7.52908470320697,-2.42834434377707,5.53401785705166));
#66274=CARTESIAN_POINT('Ctrl Pts',(7.52687405021886,-2.43518782694959,5.53373061937226));
#66275=CARTESIAN_POINT('Ctrl Pts',(7.52055205146019,-2.45466788526552,5.53291352475275));
#66276=CARTESIAN_POINT('Ctrl Pts',(7.51641818475173,-2.46729715678315,5.53238442451228));
#66277=CARTESIAN_POINT('Ctrl Pts',(7.49406862765426,-2.53499925504279,5.52955144002753));
#66278=CARTESIAN_POINT('Ctrl Pts',(7.47527922314624,-2.58988156872399,5.52726692462762));
#66279=CARTESIAN_POINT('Ctrl Pts',(7.419002104162,-2.74854576203569,5.52069516276651));
#66280=CARTESIAN_POINT('Ctrl Pts',(7.37994412608967,-2.85175768996061,5.51646136557125));
#66281=CARTESIAN_POINT('Ctrl Pts',(7.23833043271452,-3.20355970950644,5.50214614670354));
#66282=CARTESIAN_POINT('Ctrl Pts',(7.12526656651669,-3.44772556345542,5.49241976365217));
#66283=CARTESIAN_POINT('Ctrl Pts',(6.89051923623114,-3.89356761827715,5.47470902098286));
#66284=CARTESIAN_POINT('Ctrl Pts',(6.77184723745495,-4.0964878828728,5.46666682230964));
#66285=CARTESIAN_POINT('Ctrl Pts',(6.30382404455578,-4.82071219808375,5.43734913745196));
#66286=CARTESIAN_POINT('Ctrl Pts',(5.9019117183868,-5.30515752190417,5.41662268430215));
#66287=CARTESIAN_POINT('Ctrl Pts',(5.44582022749347,-5.73820234441149,5.39185914061455));
#66288=CARTESIAN_POINT('Ctrl Pts',(5.44454390179606,-5.73941336697351,5.39178983285197));
#66289=CARTESIAN_POINT('Ctrl Pts',(5.41561536434037,-5.76684344414265,5.39021872098501));
#66290=CARTESIAN_POINT('Ctrl Pts',(5.38777491550423,-5.79286237111219,5.38870219151012));
#66291=CARTESIAN_POINT('Ctrl Pts',(5.35465441903023,-5.82337058851257,5.3868912766207));
#66292=CARTESIAN_POINT('Ctrl Pts',(5.34955466991898,-5.82805574710614,5.38661225191621));
#66293=CARTESIAN_POINT('Ctrl Pts',(5.34134909306165,-5.8355743968328,5.38616298304038));
#66294=CARTESIAN_POINT('Ctrl Pts',(5.338247138314,-5.83841212702958,5.38599307403998));
#66295=CARTESIAN_POINT('Ctrl Pts',(5.33272467074675,-5.8434561102553,5.38569045117117));
#66296=CARTESIAN_POINT('Ctrl Pts',(5.33030505154964,-5.84566333137357,5.38555781493821));
#66297=CARTESIAN_POINT('Ctrl Pts',(5.3252323925531,-5.85028493607,5.38527965440236));
#66298=CARTESIAN_POINT('Ctrl Pts',(5.32257907969499,-5.85269901910348,5.38513410637005));
#66299=CARTESIAN_POINT('Ctrl Pts',(5.31563658503624,-5.85900693419021,5.38475313839462));
#66300=CARTESIAN_POINT('Ctrl Pts',(5.31134477333396,-5.8628978549431,5.38451749057208));
#66301=CARTESIAN_POINT('Ctrl Pts',(5.29260841750075,-5.87984662144051,5.3834881715472));
#66302=CARTESIAN_POINT('Ctrl Pts',(5.27812007596994,-5.89285572565744,5.38269074111624));
#66303=CARTESIAN_POINT('Ctrl Pts',(5.17442466057858,-5.98527478853529,5.37697389045674));
#66304=CARTESIAN_POINT('Ctrl Pts',(5.08348121995228,-6.06270574425857,5.37191020654303));
#66305=CARTESIAN_POINT('Ctrl Pts',(4.81481472702408,-6.28115760289221,5.35690458604107));
#66306=CARTESIAN_POINT('Ctrl Pts',(4.63273928641868,-6.4166266617673,5.34668086950046));
#66307=CARTESIAN_POINT('Ctrl Pts',(4.24004379146213,-6.683367551155,5.32494517502725));
#66308=CARTESIAN_POINT('Ctrl Pts',(4.02854954289427,-6.81294063864242,5.31341506509093));
#66309=CARTESIAN_POINT('Ctrl Pts',(3.55014522555859,-7.07596087184507,5.28816772428524));
#66310=CARTESIAN_POINT('Ctrl Pts',(3.28105046358647,-7.20468440826013,5.27450473494476));
#66311=CARTESIAN_POINT('Ctrl Pts',(2.85189109243631,-7.38093148878701,5.25387180039208));
#66312=CARTESIAN_POINT('Ctrl Pts',(2.69651134816254,-7.43910365174001,5.24662331968075));
#66313=CARTESIAN_POINT('Ctrl Pts',(2.51267588593666,-7.50141171983601,5.23832199560696));
#66314=CARTESIAN_POINT('Ctrl Pts',(2.48589190813856,-7.51033017524066,5.23711921479041));
#66315=CARTESIAN_POINT('Ctrl Pts',(2.43917513217959,-7.52560850692108,5.23503298502007));
#66316=CARTESIAN_POINT('Ctrl Pts',(2.41926386294814,-7.53203299881919,5.2341474820606));
#66317=CARTESIAN_POINT('Ctrl Pts',(2.3929366404672,-7.54041246959668,5.23298150078921));
#66318=CARTESIAN_POINT('Ctrl Pts',(2.38654344802886,-7.54243835559213,5.2326987360169));
#66319=CARTESIAN_POINT('Ctrl Pts',(2.24068365330851,-7.58845464176538,5.22625610003152));
#66320=CARTESIAN_POINT('Ctrl Pts',(2.10002202388193,-7.62857900902259,5.22022319384978));
#66321=CARTESIAN_POINT('Ctrl Pts',(1.94130260266432,-7.66913123002159,5.21361163633654));
#66322=CARTESIAN_POINT('Ctrl Pts',(1.92426731585183,-7.6734232856582,5.2129045130747));
#66323=CARTESIAN_POINT('Ctrl Pts',(1.89958218180412,-7.6795553539887,5.21188343177967));
#66324=CARTESIAN_POINT('Ctrl Pts',(1.89194372456656,-7.68144074011864,5.21156796872443));
#66325=CARTESIAN_POINT('Ctrl Pts',(1.87850953909575,-7.68473542080214,5.21101401454212));
#66326=CARTESIAN_POINT('Ctrl Pts',(1.87271501229685,-7.68614956002874,5.21077536295318));
#66327=CARTESIAN_POINT('Ctrl Pts',(1.86078256180256,-7.68904734884855,5.21028449933993));
#66328=CARTESIAN_POINT('Ctrl Pts',(1.85464444891714,-7.69053020561584,5.21003231371852));
#66329=CARTESIAN_POINT('Ctrl Pts',(1.8422654391753,-7.69350506767117,5.2095243569158));
#66330=CARTESIAN_POINT('Ctrl Pts',(1.83602448910071,-7.69499683238017,5.20926859384797));
#66331=CARTESIAN_POINT('Ctrl Pts',(1.81139562774766,-7.70085216292545,5.20826055102294));
#66332=CARTESIAN_POINT('Ctrl Pts',(1.79299384759245,-7.70515744319818,5.20751019909747));
#66333=CARTESIAN_POINT('Ctrl Pts',(1.57810016597318,-7.75462244532385,5.1987802541683));
#66334=CARTESIAN_POINT('Ctrl Pts',(1.37995964699328,-7.79232237260666,5.1910512489065));
#66335=CARTESIAN_POINT('Ctrl Pts',(0.890968020032899,-7.86612265833955,
5.17262840179251));
#66336=CARTESIAN_POINT('Ctrl Pts',(0.599137367636005,-7.89371635379074,
5.16219693247563));
#66337=CARTESIAN_POINT('Ctrl Pts',(-0.428471933227776,-7.93355122247504,
5.12641603759899));
#66338=CARTESIAN_POINT('Ctrl Pts',(-1.16363922138665,-7.85941737862278,
5.10277865502671));
#66339=CARTESIAN_POINT('Ctrl Pts',(-1.91999253216604,-7.67459643573014,
5.07220294834361));
#66340=CARTESIAN_POINT('Ctrl Pts',(-1.96203479673353,-7.66395596914826,
5.07048127575492));
#66341=CARTESIAN_POINT('Ctrl Pts',(-2.01103863132241,-7.65112395424004,
5.06844642171024));
#66342=CARTESIAN_POINT('Ctrl Pts',(-2.01808799430845,-7.64926761110933,
5.06815302008423));
#66343=CARTESIAN_POINT('Ctrl Pts',(-2.02936187150806,-7.64628213682953,
5.06768268524874));
#66344=CARTESIAN_POINT('Ctrl Pts',(-2.03358804624155,-7.64515923833829,
5.06750612489999));
#66345=CARTESIAN_POINT('Ctrl Pts',(-2.04109050360451,-7.64315916749087,
5.06719224995212));
#66346=CARTESIAN_POINT('Ctrl Pts',(-2.04436716138332,-7.64228338998845,
5.06705501810331));
#66347=CARTESIAN_POINT('Ctrl Pts',(-2.05118423540561,-7.64045664023745,
5.06676919991644));
#66348=CARTESIAN_POINT('Ctrl Pts',(-2.05472455511314,-7.63950531392277,
5.06662059272963));
#66349=CARTESIAN_POINT('Ctrl Pts',(-2.0638764039309,-7.63703928056875,5.0662359934031));
#66350=CARTESIAN_POINT('Ctrl Pts',(-2.06948691881879,-7.63552085166107,
5.06599978350611));
#66351=CARTESIAN_POINT('Ctrl Pts',(-2.09305728041989,-7.6291138853219,5.06500563905816));
#66352=CARTESIAN_POINT('Ctrl Pts',(-2.11100139144183,-7.62416818864292,
5.06424439861309));
#66353=CARTESIAN_POINT('Ctrl Pts',(-2.23402160194552,-7.58979416784353,
5.05899615232844));
#66354=CARTESIAN_POINT('Ctrl Pts',(-2.33849244929992,-7.55825900139326,
5.05439205598049));
#66355=CARTESIAN_POINT('Ctrl Pts',(-2.66461291928151,-7.45240912924316,
5.03962993170186));
#66356=CARTESIAN_POINT('Ctrl Pts',(-2.88363371305214,-7.37042798336743,
5.02914512901995));
#66357=CARTESIAN_POINT('Ctrl Pts',(-3.32546959450999,-7.18233403775669,
5.00724378642243));
#66358=CARTESIAN_POINT('Ctrl Pts',(-3.54761102952931,-7.07524728994771,
4.99582061292049));
#66359=CARTESIAN_POINT('Ctrl Pts',(-3.87552666056263,-6.89783887445839,
4.97862181384411));
#66360=CARTESIAN_POINT('Ctrl Pts',(-3.98520935426634,-6.8350563357683,4.97280819635379));
#66361=CARTESIAN_POINT('Ctrl Pts',(-4.22829323390074,-6.68807353137622,
4.95982983710774));
#66362=CARTESIAN_POINT('Ctrl Pts',(-4.36077719442273,-6.60245529898888,
4.95269083661561));
#66363=CARTESIAN_POINT('Ctrl Pts',(-4.80699792251463,-6.2947895277123,4.92851108551677));
#66364=CARTESIAN_POINT('Ctrl Pts',(-5.10708594539538,-6.05386909264616,
4.9120446361679));
#66365=CARTESIAN_POINT('Ctrl Pts',(-5.40765727608774,-5.77424007167193,
4.89540307254504));
#66366=CARTESIAN_POINT('Ctrl Pts',(-5.42672583031313,-5.75632281935096,
4.89434644852284));
#66367=CARTESIAN_POINT('Ctrl Pts',(-5.45287813165452,-5.73150406683766,
4.89289602763517));
#66368=CARTESIAN_POINT('Ctrl Pts',(-5.4600382483855,-5.72468349465123,4.89249879095456));
#66369=CARTESIAN_POINT('Ctrl Pts',(-5.47142371467195,-5.71379715406999,
4.89186691877582));
#66370=CARTESIAN_POINT('Ctrl Pts',(-5.47565735380193,-5.70974009279524,
4.89163191170061));
#66371=CARTESIAN_POINT('Ctrl Pts',(-5.4838859887871,-5.70183709106808,4.89117504964814));
#66372=CARTESIAN_POINT('Ctrl Pts',(-5.48788145906199,-5.69799164991946,
4.89095317348654));
#66373=CARTESIAN_POINT('Ctrl Pts',(-5.49613082791164,-5.69003531776596,
4.89049497853555));
#66374=CARTESIAN_POINT('Ctrl Pts',(-5.50038416581546,-5.68592384961104,
4.89025868476488));
#66375=CARTESIAN_POINT('Ctrl Pts',(-5.51003213202295,-5.67657673407986,
4.88972257637979));
#66376=CARTESIAN_POINT('Ctrl Pts',(-5.51542392066684,-5.6713381568686,4.88942288795969));
#66377=CARTESIAN_POINT('Ctrl Pts',(-5.52908126568421,-5.65803099835766,
4.8886635652447));
#66378=CARTESIAN_POINT('Ctrl Pts',(-5.53733664542472,-5.64995197303344,
4.88820438124126));
#66379=CARTESIAN_POINT('Ctrl Pts',(-5.62953882810789,-5.55932325814271,
4.88307355545819));
#66380=CARTESIAN_POINT('Ctrl Pts',(-5.71165241360203,-5.47492563031201,
4.87848289381951));
#66381=CARTESIAN_POINT('Ctrl Pts',(-5.92513051783187,-5.2454772625069,4.86646638034512));
#66382=CARTESIAN_POINT('Ctrl Pts',(-6.05305100791411,-5.0973309005762,4.859180563585));
#66383=CARTESIAN_POINT('Ctrl Pts',(-6.26408275052058,-4.83377098473046,
4.84689468706409));
#66384=CARTESIAN_POINT('Ctrl Pts',(-6.34981621841605,-4.72058366149653,
4.84181779491729));
#66385=CARTESIAN_POINT('Ctrl Pts',(-6.82622800964603,-4.05513295250188,
4.81289545506634));
#66386=CARTESIAN_POINT('Ctrl Pts',(-7.1477806944428,-3.45695464486397,4.79070779214516));
#66387=CARTESIAN_POINT('Ctrl Pts',(-7.40972639245703,-2.77184859914397,
4.76285418706393));
#66388=CARTESIAN_POINT('Ctrl Pts',(-7.42956501495622,-2.71822613366663,
4.7606573527678));
#66389=CARTESIAN_POINT('Ctrl Pts',(-7.46984340307126,-2.6056202526197,4.75600035716128));
#66390=CARTESIAN_POINT('Ctrl Pts',(-7.49016965978471,-2.54660076678196,
4.75353470644808));
#66391=CARTESIAN_POINT('Ctrl Pts',(-7.51244983040541,-2.47933254075756,
4.75069015977429));
#66392=CARTESIAN_POINT('Ctrl Pts',(-7.51509193466226,-2.47131250849409,
4.75035046899859));
#66393=CARTESIAN_POINT('Ctrl Pts',(-7.51907665262619,-2.45915152888948,
4.74983453246708));
#66394=CARTESIAN_POINT('Ctrl Pts',(-7.52042870319198,-2.45501365986703,
4.74965883118682));
#66395=CARTESIAN_POINT('Ctrl Pts',(-7.5227766250305,-2.44780784661962,4.74935259552582));
#66396=CARTESIAN_POINT('Ctrl Pts',(-7.52377403764787,-2.44474040225809,
4.74922215075859));
#66397=CARTESIAN_POINT('Ctrl Pts',(-7.5258587182061,-2.43831581346585,4.74894876571159));
#66398=CARTESIAN_POINT('Ctrl Pts',(-7.52694561464965,-2.43495855541102,
4.74880580391882));
#66399=CARTESIAN_POINT('Ctrl Pts',(-7.5295368802034,-2.42693621585783,4.74846395090658));
#66400=CARTESIAN_POINT('Ctrl Pts',(-7.53103916009834,-2.42227046282022,
4.74826493833207));
#66401=CARTESIAN_POINT('Ctrl Pts',(-7.53610174353222,-2.40649694980396,
4.74759149341887));
#66402=CARTESIAN_POINT('Ctrl Pts',(-7.53964180203625,-2.39538275701834,
4.74711589951726));
#66403=CARTESIAN_POINT('Ctrl Pts',(-7.6510658372388,-2.04286720655529,4.73199803653185));
#66404=CARTESIAN_POINT('Ctrl Pts',(-7.73566424716292,-1.69456991453052,
4.71608971253339));
#66405=CARTESIAN_POINT('Ctrl Pts',(-7.87227861830664,-0.90077509254703,
4.67947086257571));
#66406=CARTESIAN_POINT('Ctrl Pts',(-7.91062332330754,-0.454110717659903,
4.65865197264493));
#66407=CARTESIAN_POINT('Ctrl Pts',(-7.91099723840516,-0.0066101396285724,
4.63857575021375));
#66408=CARTESIAN_POINT('Ctrl Pts',(-7.91099726676438,-0.00657611181310816,
4.63857422362495));
#66409=CARTESIAN_POINT('Ctrl Pts',(-7.9113461326049,0.413106033086809,4.61974605390583));
#66410=CARTESIAN_POINT('Ctrl Pts',(-7.87829895328532,0.832195301771229,
4.60162986480888));
#66411=CARTESIAN_POINT('Ctrl Pts',(-7.80869075279927,1.26836483588196,4.58368330375488));
#66412=CARTESIAN_POINT('Ctrl Pts',(-7.80514953152656,1.28997729834642,4.58279626632511));
#66413=CARTESIAN_POINT('Ctrl Pts',(-7.79957281418619,1.32314876595044,4.58143819724901));
#66414=CARTESIAN_POINT('Ctrl Pts',(-7.79760128023062,1.33471832860122,4.5809651620792));
#66415=CARTESIAN_POINT('Ctrl Pts',(-7.79431135143178,1.35376853773993,4.58018730769839));
#66416=CARTESIAN_POINT('Ctrl Pts',(-7.79300791898969,1.36125172977364,4.57988201897181));
#66417=CARTESIAN_POINT('Ctrl Pts',(-7.79066592557885,1.3745838366973,4.57933858188826));
#66418=CARTESIAN_POINT('Ctrl Pts',(-7.78963155133526,1.38043347639168,4.57910030208452));
#66419=CARTESIAN_POINT('Ctrl Pts',(-7.78761651413336,1.39175462195172,4.57863945487179));
#66420=CARTESIAN_POINT('Ctrl Pts',(-7.78663667154418,1.39722626815737,4.57841686186114));
#66421=CARTESIAN_POINT('Ctrl Pts',(-7.78461698452675,1.40843651503787,4.57796110166126));
#66422=CARTESIAN_POINT('Ctrl Pts',(-7.78357655964526,1.41417500790755,4.57772795291462));
#66423=CARTESIAN_POINT('Ctrl Pts',(-7.78107324115795,1.42789567922791,4.57717086270932));
#66424=CARTESIAN_POINT('Ctrl Pts',(-7.77960440781211,1.43587677517552,4.57684710843452));
#66425=CARTESIAN_POINT('Ctrl Pts',(-7.77428334955081,1.46454158546665,4.57568537435958));
#66426=CARTESIAN_POINT('Ctrl Pts',(-7.77036088056845,1.48521225724189,4.57484960884818));
#66427=CARTESIAN_POINT('Ctrl Pts',(-7.71297578157759,1.78117004491051,4.56291121538317));
#66428=CARTESIAN_POINT('Ctrl Pts',(-7.64499308453453,2.05345086443624,4.5522847487377));
#66429=CARTESIAN_POINT('Ctrl Pts',(-7.5258993133572,2.44140875890111,4.53744649876811));
#66430=CARTESIAN_POINT('Ctrl Pts',(-7.48626573197478,2.56036399048052,4.53293754984294));
#66431=CARTESIAN_POINT('Ctrl Pts',(-7.43172633737116,2.71194411482492,4.52721686896124));
#66432=CARTESIAN_POINT('Ctrl Pts',(-7.41940394808735,2.74547670049398,4.52595289539375));
#66433=CARTESIAN_POINT('Ctrl Pts',(-7.18938955804791,3.35854948915662,4.50286190390203));
#66434=CARTESIAN_POINT('Ctrl Pts',(-6.90466090853297,3.91059232269851,4.48255338963114));
#66435=CARTESIAN_POINT('Ctrl Pts',(-6.43819736912211,4.60215586547379,4.45209327277847));
#66436=CARTESIAN_POINT('Ctrl Pts',(-6.31064937823296,4.775553967995,4.44395249049151));
#66437=CARTESIAN_POINT('Ctrl Pts',(-6.16947094897371,4.9519355062321,4.43489464959119));
#66438=CARTESIAN_POINT('Ctrl Pts',(-6.16272211331928,4.96033196469787,4.43446154403397));
#66439=CARTESIAN_POINT('Ctrl Pts',(-6.15301521540111,4.97235826190897,4.43383840975184));
#66440=CARTESIAN_POINT('Ctrl Pts',(-6.15007102283519,4.97599933075136,4.43364938163703));
#66441=CARTESIAN_POINT('Ctrl Pts',(-6.14496447784659,4.98230311521361,4.43332147398018));
#66442=CARTESIAN_POINT('Ctrl Pts',(-6.14280362032367,4.98496704582215,4.43318270338037));
#66443=CARTESIAN_POINT('Ctrl Pts',(-6.13865221788584,4.9900781455581,4.43291606916263));
#66444=CARTESIAN_POINT('Ctrl Pts',(-6.13666194005881,4.99252553166319,4.43278822514949));
#66445=CARTESIAN_POINT('Ctrl Pts',(-6.1319800007823,4.99827574506915,4.4324874510393));
#66446=CARTESIAN_POINT('Ctrl Pts',(-6.1292871344986,5.00157758878303,4.43231443178927));
#66447=CARTESIAN_POINT('Ctrl Pts',(-6.11990333844358,5.01306452104573,4.4317114189976));
#66448=CARTESIAN_POINT('Ctrl Pts',(-6.1131987048338,5.02123832905829,4.43128040706413));
#66449=CARTESIAN_POINT('Ctrl Pts',(-6.0323667443222,5.11938099048258,4.42608236925635));
#66450=CARTESIAN_POINT('Ctrl Pts',(-5.95627915950428,5.20771027995432,4.42117238894877));
#66451=CARTESIAN_POINT('Ctrl Pts',(-5.42676746904316,5.79562568742529,4.38709675512741));
#66452=CARTESIAN_POINT('Ctrl Pts',(-4.91299893262688,6.23711222095047,4.35475675985159));
#66453=CARTESIAN_POINT('Ctrl Pts',(-4.1804002909589,6.71930976424148,4.31498152846115));
#66454=CARTESIAN_POINT('Ctrl Pts',(-4.0071570860641,6.82404345354929,4.30595104611405));
#66455=CARTESIAN_POINT('Ctrl Pts',(-3.6596479254456,7.01632657621063,4.28864502927477));
#66456=CARTESIAN_POINT('Ctrl Pts',(-3.48578344059753,7.10430732468601,4.28035966991629));
#66457=CARTESIAN_POINT('Ctrl Pts',(-3.25612831501158,7.21005665594024,4.26990186611492));
#66458=CARTESIAN_POINT('Ctrl Pts',(-3.20315101459247,7.23374815414356,4.26752189287803));
#66459=CARTESIAN_POINT('Ctrl Pts',(-3.1167633037527,7.27124568226868,4.26369288065955));
#66460=CARTESIAN_POINT('Ctrl Pts',(-3.08351105439703,7.28540917776741,4.26223136304086));
#66461=CARTESIAN_POINT('Ctrl Pts',(-3.04294818463583,7.30235910386455,4.26046334279329));
#66462=CARTESIAN_POINT('Ctrl Pts',(-3.03572928254775,7.30536308883576,4.26014925968905));
#66463=CARTESIAN_POINT('Ctrl Pts',(-3.023065936168,7.31061064623256,4.25959929049798));
#66464=CARTESIAN_POINT('Ctrl Pts',(-3.01762342444244,7.31285884888284,4.25936324329587));
#66465=CARTESIAN_POINT('Ctrl Pts',(-3.00664801553082,7.31737825193149,4.25888787440208));
#66466=CARTESIAN_POINT('Ctrl Pts',(-3.00111504272893,7.31964925878599,4.25864855955188));
#66467=CARTESIAN_POINT('Ctrl Pts',(-2.99045810324077,7.32400928123497,4.2581882545279));
#66468=CARTESIAN_POINT('Ctrl Pts',(-2.98533451129728,7.3260991990737,4.25796723311663));
#66469=CARTESIAN_POINT('Ctrl Pts',(-2.97324025818644,7.33101766180571,4.25744617472242));
#66470=CARTESIAN_POINT('Ctrl Pts',(-2.96626774076713,7.33384164548961,4.25714629610532));
#66471=CARTESIAN_POINT('Ctrl Pts',(-2.94205819848575,7.34360673306386,4.25610687189978));
#66472=CARTESIAN_POINT('Ctrl Pts',(-2.92480069062687,7.35049707295204,4.25536908548243));
#66473=CARTESIAN_POINT('Ctrl Pts',(-2.72763869072126,7.42841290996933,4.24697575651684));
#66474=CARTESIAN_POINT('Ctrl Pts',(-2.54520577019872,7.49288096473461,4.23955016034975));
#66475=CARTESIAN_POINT('Ctrl Pts',(-2.1481941124392,7.61700083548056,4.22401648706631));
#66476=CARTESIAN_POINT('Ctrl Pts',(-1.93309052457241,7.67441253341597,4.21598180268807));
#66477=CARTESIAN_POINT('Ctrl Pts',(-1.44406121445967,7.78306627934274,4.19830125171412));
#66478=CARTESIAN_POINT('Ctrl Pts',(-1.16927581143561,7.82906329113373,4.1887726796936));
#66479=CARTESIAN_POINT('Ctrl Pts',(-0.859015539428168,7.86429641872186,
4.17809123347411));
#66480=CARTESIAN_POINT('Ctrl Pts',(-0.825371726146504,7.86789853587983,
4.17693384475849));
#66481=CARTESIAN_POINT('Ctrl Pts',(-0.753203540400699,7.87515732235826,
4.17445154571953));
#66482=CARTESIAN_POINT('Ctrl Pts',(-0.714673374249742,7.87874738691195,
4.17312649065848));
#66483=CARTESIAN_POINT('Ctrl Pts',(-0.63159310311237,7.88587396853312,4.17026750962228));
#66484=CARTESIAN_POINT('Ctrl Pts',(-0.587036277189106,7.8893159707387,4.16873306794271));
#66485=CARTESIAN_POINT('Ctrl Pts',(-0.490170527452116,7.89597367029267,
4.16539098863235));
#66486=CARTESIAN_POINT('Ctrl Pts',(-0.437854062968823,7.89904748185584,
4.16358201762563));
#66487=CARTESIAN_POINT('Ctrl Pts',(-0.322506537285998,7.90467517138215,
4.15957855518861));
#66488=CARTESIAN_POINT('Ctrl Pts',(-0.25946785672346,7.90699540558906,4.15738074223292));
#66489=CARTESIAN_POINT('Ctrl Pts',(0.0328355819333474,7.91425474497045,
4.14711974313601));
#66490=CARTESIAN_POINT('Ctrl Pts',(0.26220761524485,7.909977391763,4.13887034271463));
#66491=CARTESIAN_POINT('Ctrl Pts',(0.594608680693564,7.88930454105963,4.1262376284037));
#66492=CARTESIAN_POINT('Ctrl Pts',(0.698020675745524,7.88082807214791,4.12221139048813));
#66493=CARTESIAN_POINT('Ctrl Pts',(0.818973251966151,7.86851458849383,4.11735879227862));
#66494=CARTESIAN_POINT('Ctrl Pts',(0.83670828271239,7.86664847674009,4.11664364126642));
#66495=CARTESIAN_POINT('Ctrl Pts',(0.860010697111956,7.86411686312228,4.1156990487015));
#66496=CARTESIAN_POINT('Ctrl Pts',(0.865584020258824,7.86350537225923,4.11547275530861));
#66497=CARTESIAN_POINT('Ctrl Pts',(0.874680690835874,7.86249752052174,4.11510278989729));
#66498=CARTESIAN_POINT('Ctrl Pts',(0.878204438470202,7.86210471408913,4.1149593272395));
#66499=CARTESIAN_POINT('Ctrl Pts',(0.884995674509492,7.86134304484092,4.11468254317032));
#66500=CARTESIAN_POINT('Ctrl Pts',(0.888263199406716,7.86097451345243,4.11454924137605));
#66501=CARTESIAN_POINT('Ctrl Pts',(0.895797945565579,7.86011994094739,4.11424155232053));
#66502=CARTESIAN_POINT('Ctrl Pts',(0.900064988862908,7.85963246348314,4.11406708027626));
#66503=CARTESIAN_POINT('Ctrl Pts',(0.91374006954864,7.85805890638206,4.11350721990209));
#66504=CARTESIAN_POINT('Ctrl Pts',(0.923146522803904,7.8569594110432,4.11312104083225));
#66505=CARTESIAN_POINT('Ctrl Pts',(1.00652200016415,7.84706207992535,4.10968867769814));
#66506=CARTESIAN_POINT('Ctrl Pts',(1.08036307204307,7.83723706174253,4.10658316599355));
#66507=CARTESIAN_POINT('Ctrl Pts',(1.80923373930108,7.72976009046038,4.07535546164927));
#66508=CARTESIAN_POINT('Ctrl Pts',(2.4496657420749,7.5512660580536,4.0435378618385));
#66509=CARTESIAN_POINT('Ctrl Pts',(3.36686820783636,7.16649222607155,3.99756935831303));
#66510=CARTESIAN_POINT('Ctrl Pts',(3.66499985560903,7.01870487430802,3.98251432674953));
#66511=CARTESIAN_POINT('Ctrl Pts',(4.11028283307435,6.76183990387279,3.96017117581671));
#66512=CARTESIAN_POINT('Ctrl Pts',(4.26443130901173,6.66569841696209,3.95246058826742));
#66513=CARTESIAN_POINT('Ctrl Pts',(4.46148063829603,6.53316387841869,3.94263896580992));
#66514=CARTESIAN_POINT('Ctrl Pts',(4.50748920022761,6.50150605869257,3.94034815569935));
#66515=CARTESIAN_POINT('Ctrl Pts',(4.58192315704946,6.4491191927419,3.9366453678727));
#66516=CARTESIAN_POINT('Ctrl Pts',(4.61055187983273,6.42868334773626,3.93522202210638));
#66517=CARTESIAN_POINT('Ctrl Pts',(4.6453607668822,6.40348383042291,3.93349225132037));
#66518=CARTESIAN_POINT('Ctrl Pts',(4.65167116992574,6.39890124539521,3.93317869985202));
#66519=CARTESIAN_POINT('Ctrl Pts',(4.66388318123222,6.39000532904415,3.93257197119375));
#66520=CARTESIAN_POINT('Ctrl Pts',(4.66978560637872,6.38569313577089,3.93227874952173));
#66521=CARTESIAN_POINT('Ctrl Pts',(4.68045423842075,6.37787614508806,3.93174879981233));
#66522=CARTESIAN_POINT('Ctrl Pts',(4.68522250303956,6.37437417298724,3.93151196032289));
#66523=CARTESIAN_POINT('Ctrl Pts',(4.69473080512801,6.36737452714166,3.93103971680801));
#66524=CARTESIAN_POINT('Ctrl Pts',(4.69947087304328,6.36387690131776,3.93080431112737));
#66525=CARTESIAN_POINT('Ctrl Pts',(4.71274907888548,6.35405618486938,3.93014492079969));
#66526=CARTESIAN_POINT('Ctrl Pts',(4.72127840683957,6.34772117277358,3.92972140932326));
#66527=CARTESIAN_POINT('Ctrl Pts',(4.75592001619211,6.32188326456845,3.92800151959611));
#66528=CARTESIAN_POINT('Ctrl Pts',(4.78192459528733,6.30223614355705,3.92671088252802));
#66529=CARTESIAN_POINT('Ctrl Pts',(5.18435880848601,5.99426191876322,3.90674200385417));
#66530=CARTESIAN_POINT('Ctrl Pts',(5.53426070615083,5.67280992077122,3.88952291819492));
#66531=CARTESIAN_POINT('Ctrl Pts',(6.19015867324328,4.95142548559815,3.85543642278137));
#66532=CARTESIAN_POINT('Ctrl Pts',(6.49107402614173,4.54979086371607,3.83870690388996));
#66533=CARTESIAN_POINT('Ctrl Pts',(6.7994156173806,4.04476800415872,3.81745028651577));
#66534=CARTESIAN_POINT('Ctrl Pts',(6.84548840490171,3.96629408710438,3.81413927791344));
#66535=CARTESIAN_POINT('Ctrl Pts',(6.9699844044705,3.74561180077756,3.80476118564742));
#66536=CARTESIAN_POINT('Ctrl Pts',(7.04539800874132,3.60175752857554,3.79856984891739));
#66537=CARTESIAN_POINT('Ctrl Pts',(7.12809184909534,3.43146505073849,3.79104984562325));
#66538=CARTESIAN_POINT('Ctrl Pts',(7.13972818106474,3.4071875904325,3.78997378134248));
#66539=CARTESIAN_POINT('Ctrl Pts',(7.15457606103271,3.37579964487902,3.7885778478988));
#66540=CARTESIAN_POINT('Ctrl Pts',(7.15790142996604,3.36874293672058,3.78826370530835));
#66541=CARTESIAN_POINT('Ctrl Pts',(7.16324982095177,3.35734953530132,3.78775602657592));
#66542=CARTESIAN_POINT('Ctrl Pts',(7.16527936098063,3.35301589296802,3.78756281184802));
#66543=CARTESIAN_POINT('Ctrl Pts',(7.16894909997456,3.34516141442336,3.78721242188283));
#66544=CARTESIAN_POINT('Ctrl Pts',(7.17059064186508,3.34164120355616,3.7870553120658));
#66545=CARTESIAN_POINT('Ctrl Pts',(7.17448069898205,3.33328309045065,3.78668211320358));
#66546=CARTESIAN_POINT('Ctrl Pts',(7.17672691206228,3.32844412461362,3.78646591333636));
#66547=CARTESIAN_POINT('Ctrl Pts',(7.18238909130059,3.31621384136436,3.78591914329472));
#66548=CARTESIAN_POINT('Ctrl Pts',(7.18579853796791,3.30881952839231,3.78558826353629));
#66549=CARTESIAN_POINT('Ctrl Pts',(7.20403239091891,3.26911335549267,3.78380989421684));
#66550=CARTESIAN_POINT('Ctrl Pts',(7.21865012854457,3.23670744515868,3.78235280280194));
#66551=CARTESIAN_POINT('Ctrl Pts',(7.5233897602565,2.54879984287543,3.75131737612828));
#66552=CARTESIAN_POINT('Ctrl Pts',(7.72330635234167,1.85697598462248,3.71845160350633));
#66553=CARTESIAN_POINT('Ctrl Pts',(7.85578943479332,0.953435919954922,3.67860894188584));
#66554=CARTESIAN_POINT('Ctrl Pts',(7.87703192123432,0.758182116598835,3.67014968929901));
#66555=CARTESIAN_POINT('Ctrl Pts',(7.90557668066405,0.357626394008536,3.65313974142851));
#66556=CARTESIAN_POINT('Ctrl Pts',(7.91219390578955,0.152422220298308,3.64460897013142));
#66557=CARTESIAN_POINT('Ctrl Pts',(7.91057662893636,-0.0898222997029053,
3.63473730704896));
#66558=CARTESIAN_POINT('Ctrl Pts',(7.91006986536628,-0.12682825148641,3.6332346696947));
#66559=CARTESIAN_POINT('Ctrl Pts',(7.90890315018272,-0.183154517483053,
3.63095540683182));
#66560=CARTESIAN_POINT('Ctrl Pts',(7.9084320354041,-0.202478053636192,3.63017488473024));
#66561=CARTESIAN_POINT('Ctrl Pts',(7.90754770532422,-0.234007330673138,
3.62890359356408));
#66562=CARTESIAN_POINT('Ctrl Pts',(7.90717703974626,-0.246214146701041,
3.62841195298656));
#66563=CARTESIAN_POINT('Ctrl Pts',(7.90640842014516,-0.269731300098618,
3.62746582082769));
#66564=CARTESIAN_POINT('Ctrl Pts',(7.90601445892209,-0.281041734638155,
3.62701124890992));
#66565=CARTESIAN_POINT('Ctrl Pts',(7.90525713516359,-0.301520849151827,
3.62618901105196));
#66566=CARTESIAN_POINT('Ctrl Pts',(7.90490208906579,-0.310689810305537,
3.62582117688634));
#66567=CARTESIAN_POINT('Ctrl Pts',(7.90415890407945,-0.329055854651695,
3.62508497546821));
#66568=CARTESIAN_POINT('Ctrl Pts',(7.90377066320563,-0.338252923671653,
3.62471661119487));
#66569=CARTESIAN_POINT('Ctrl Pts',(7.90265310833152,-0.36367374169184,3.62369927288451));
#66570=CARTESIAN_POINT('Ctrl Pts',(7.90188988704084,-0.379895981475649,
3.62305099009468));
#66571=CARTESIAN_POINT('Ctrl Pts',(7.89869923170493,-0.443538009338258,
3.62051131205509));
#66572=CARTESIAN_POINT('Ctrl Pts',(7.89589483711112,-0.490938189700778,
3.61862767657726));
#66573=CARTESIAN_POINT('Ctrl Pts',(7.83679487522013,-1.3574567574322,3.58433352492923));
#66574=CARTESIAN_POINT('Ctrl Pts',(7.65376146253957,-2.16285430851055,3.55546092757715));
#66575=CARTESIAN_POINT('Ctrl Pts',(7.27933111055042,-3.10353123309247,3.5184128417499));
#66576=CARTESIAN_POINT('Ctrl Pts',(7.2021041731806,-3.27875871758812,3.51132144737967));
#66577=CARTESIAN_POINT('Ctrl Pts',(7.06094892846123,-3.5699281841366,3.49899125446052));
#66578=CARTESIAN_POINT('Ctrl Pts',(7.0003282870638,-3.6873823346244,3.49386019219852));
#66579=CARTESIAN_POINT('Ctrl Pts',(6.92586660625074,-3.82319364130145,3.48768605027054));
#66580=CARTESIAN_POINT('Ctrl Pts',(6.91485096587378,-3.84308131206811,3.48677575580106));
#66581=CARTESIAN_POINT('Ctrl Pts',(6.90017269478158,-3.86931407985933,3.48556652568591));
#66582=CARTESIAN_POINT('Ctrl Pts',(6.89658668702919,-3.87570209564345,3.48527139278894));
#66583=CARTESIAN_POINT('Ctrl Pts',(6.89069575709783,-3.8861619724174,3.4847870238208));
#66584=CARTESIAN_POINT('Ctrl Pts',(6.88839608119013,-3.89023679501067,3.48459805264576));
#66585=CARTESIAN_POINT('Ctrl Pts',(6.88394141698612,-3.89811373199796,3.48423221706504));
#66586=CARTESIAN_POINT('Ctrl Pts',(6.88178688996864,-3.9019161063546,3.48405537622846));
#66587=CARTESIAN_POINT('Ctrl Pts',(6.87681818007794,-3.91066811897232,3.48364777194068));
#66588=CARTESIAN_POINT('Ctrl Pts',(6.87400180460029,-3.91561650429318,3.48341689547405));
#66589=CARTESIAN_POINT('Ctrl Pts',(6.8650220857485,-3.93135436739274,3.48268127459577));
#66590=CARTESIAN_POINT('Ctrl Pts',(6.85883868507879,-3.94213232770218,3.48217548259414));
#66591=CARTESIAN_POINT('Ctrl Pts',(6.79915976145434,-4.04559005024999,3.47730067454748));
#66592=CARTESIAN_POINT('Ctrl Pts',(6.74382121814735,-4.13717834663212,3.47282585299034));
#66593=CARTESIAN_POINT('Ctrl Pts',(6.68044360613762,-4.2374200617693,3.46775773281299));
#66594=CARTESIAN_POINT('Ctrl Pts',(6.67422319014463,-4.24721089194645,3.46726093549891));
#66595=CARTESIAN_POINT('Ctrl Pts',(6.64395662616424,-4.29461926703525,3.46484686177509));
#66596=CARTESIAN_POINT('Ctrl Pts',(6.61961417028502,-4.33204598564868,3.46291499371247));
#66597=CARTESIAN_POINT('Ctrl Pts',(6.55063146943546,-4.43616830599287,3.45747153876109));
#66598=CARTESIAN_POINT('Ctrl Pts',(6.50529177037389,-4.50239273201016,3.4539293167579));
#66599=CARTESIAN_POINT('Ctrl Pts',(6.31854657755343,-4.76644726493357,3.43951512594269));
#66600=CARTESIAN_POINT('Ctrl Pts',(6.16906481531727,-4.95839515373934,3.42837206930145));
#66601=CARTESIAN_POINT('Ctrl Pts',(5.77954837991584,-5.4136373996023,3.40078035347787));
#66602=CARTESIAN_POINT('Ctrl Pts',(5.53010701885256,-5.66820819805886,3.38431470438502));
#66603=CARTESIAN_POINT('Ctrl Pts',(5.03021769156437,-6.11385521820825,3.35426489861763));
#66604=CARTESIAN_POINT('Ctrl Pts',(4.78385255596312,-6.30849415009625,3.34059416401193));
#66605=CARTESIAN_POINT('Ctrl Pts',(4.4351627534636,-6.5517686100401,3.32285292834257));
#66606=CARTESIAN_POINT('Ctrl Pts',(4.34242608550252,-6.61359793295346,3.31827598207366));
#66607=CARTESIAN_POINT('Ctrl Pts',(4.23372817827796,-6.68279654663093,3.31307073470467));
#66608=CARTESIAN_POINT('Ctrl Pts',(4.2190141431131,-6.69209560874318,3.31236943137613));
#66609=CARTESIAN_POINT('Ctrl Pts',(4.1973919216448,-6.70566089020976,3.3113436961367));
#66610=CARTESIAN_POINT('Ctrl Pts',(4.19050771729806,-6.70996512585298,3.31101783150176));
#66611=CARTESIAN_POINT('Ctrl Pts',(4.17850638290732,-6.71744308983454,3.3104509879392));
#66612=CARTESIAN_POINT('Ctrl Pts',(4.17339223927146,-6.72062158394293,3.31020982973519));
#66613=CARTESIAN_POINT('Ctrl Pts',(4.16352237718879,-6.72674019682897,3.30974516830112));
#66614=CARTESIAN_POINT('Ctrl Pts',(4.15876716235496,-6.72968111803709,3.30952163498626));
#66615=CARTESIAN_POINT('Ctrl Pts',(4.1475133713162,-6.73662468059505,3.30899341062463));
#66616=CARTESIAN_POINT('Ctrl Pts',(4.14101210675458,-6.74062296710052,3.30868888316714));
#66617=CARTESIAN_POINT('Ctrl Pts',(4.11829466574378,-6.75454895377204,3.30762694602706));
#66618=CARTESIAN_POINT('Ctrl Pts',(4.10204843214782,-6.76442763208508,3.30687137427375));
#66619=CARTESIAN_POINT('Ctrl Pts',(3.90983996775815,-6.88035473911191,3.29797749803898));
#66620=CARTESIAN_POINT('Ctrl Pts',(3.72984032651347,-6.97957224301875,3.29009823352059));
#66621=CARTESIAN_POINT('Ctrl Pts',(3.3848435529992,-7.15257486092685,3.2757283582639));
#66622=CARTESIAN_POINT('Ctrl Pts',(3.22078882215947,-7.22793306713144,3.26918915231857));
#66623=CARTESIAN_POINT('Ctrl Pts',(2.53976986034529,-7.51296210826921,3.24299384441545));
#66624=CARTESIAN_POINT('Ctrl Pts',(2.00394032043284,-7.67328024046745,3.22468660656596));
#66625=CARTESIAN_POINT('Ctrl Pts',(1.25148051286011,-7.8141468322362,3.19814487975362));
#66626=CARTESIAN_POINT('Ctrl Pts',(1.04582790496657,-7.84431839046821,3.19079256511615));
#66627=CARTESIAN_POINT('Ctrl Pts',(0.682112183144507,-7.88312202441566,
3.17728068105468));
#66628=CARTESIAN_POINT('Ctrl Pts',(0.524529798662349,-7.89517276227876,
3.17125965750425));
#66629=CARTESIAN_POINT('Ctrl Pts',(0.343699301150583,-7.90356388118705,
3.1640584609471));
#66630=CARTESIAN_POINT('Ctrl Pts',(0.320692927856891,-7.90453080572275,
3.1631368749317));
#66631=CARTESIAN_POINT('Ctrl Pts',(0.291561230009582,-7.90562777880492,
3.16196273131111));
#66632=CARTESIAN_POINT('Ctrl Pts',(0.285439321161095,-7.90585118259775,
3.16171558785424));
#66633=CARTESIAN_POINT('Ctrl Pts',(0.275671790169792,-7.90619626429341,
3.16132061998871));
#66634=CARTESIAN_POINT('Ctrl Pts',(0.272026319682302,-7.90632253243103,
3.16117306438117));
#66635=CARTESIAN_POINT('Ctrl Pts',(0.265118274049408,-7.90655702292956,
3.16089317612412));
#66636=CARTESIAN_POINT('Ctrl Pts',(0.261855725732904,-7.90666574700803,
3.16076087369509));
#66637=CARTESIAN_POINT('Ctrl Pts',(0.254447226148604,-7.90690804397598,
3.16046018306959));
#66638=CARTESIAN_POINT('Ctrl Pts',(0.25030123812789,-7.90704037531561,3.16029172241721));
#66639=CARTESIAN_POINT('Ctrl Pts',(0.239613683606313,-7.90737308560492,
3.15985698665332));
#66640=CARTESIAN_POINT('Ctrl Pts',(0.233071981559446,-7.90756860755657,
3.15959043055696));
#66641=CARTESIAN_POINT('Ctrl Pts',(0.194592457241041,-7.90867091383711,
3.15801982194463));
#66642=CARTESIAN_POINT('Ctrl Pts',(0.162650036029058,-7.9093923127789,3.15670519662121));
#66643=CARTESIAN_POINT('Ctrl Pts',(-0.370402013244937,-7.91820053529516,
3.13459676736143));
#66644=CARTESIAN_POINT('Ctrl Pts',(-0.871124245329878,-7.87884268276986,
3.11138836845481));
#66645=CARTESIAN_POINT('Ctrl Pts',(-1.8440331853989,-7.70845386717232,3.0656354948699));
#66646=CARTESIAN_POINT('Ctrl Pts',(-2.31463408691876,-7.58045331384529,
3.04320730346226));
#66647=CARTESIAN_POINT('Ctrl Pts',(-3.01048162545472,-7.32028373929692,
3.01098232744258));
#66648=CARTESIAN_POINT('Ctrl Pts',(-3.24595845126178,-7.21895588338692,
3.00023387229291));
#66649=CARTESIAN_POINT('Ctrl Pts',(-3.49284756836139,-7.09818875858424,
2.98913616852862));
#66650=CARTESIAN_POINT('Ctrl Pts',(-3.50954688055067,-7.08994700176744,
2.98838635547279));
#66651=CARTESIAN_POINT('Ctrl Pts',(-3.53350968651125,-7.07801502292328,
2.98731156375863));
#66652=CARTESIAN_POINT('Ctrl Pts',(-3.54079676104572,-7.07437245746181,
2.98698487470491));
#66653=CARTESIAN_POINT('Ctrl Pts',(-3.55343109242113,-7.06803256498799,
2.98641872627335));
#66654=CARTESIAN_POINT('Ctrl Pts',(-3.55878093003968,-7.06534041363244,
2.98617908097432));
#66655=CARTESIAN_POINT('Ctrl Pts',(-3.56905912182974,-7.06015357459443,
2.98571882820238));
#66656=CARTESIAN_POINT('Ctrl Pts',(-3.57398792890262,-7.05765979600808,
2.9854981882038));
#66657=CARTESIAN_POINT('Ctrl Pts',(-3.58558790359786,-7.05177540667011,
2.98497907366586));
#66658=CARTESIAN_POINT('Ctrl Pts',(-3.59225688589682,-7.04838048538039,
2.98468075475164));
#66659=CARTESIAN_POINT('Ctrl Pts',(-3.61526618961727,-7.03662619886458,
2.98365192933108));
#66660=CARTESIAN_POINT('Ctrl Pts',(-3.63158228865482,-7.02821940259681,
2.98292313647108));
#66661=CARTESIAN_POINT('Ctrl Pts',(-3.81174316116407,-6.93459744695517,
2.97488398113846));
#66662=CARTESIAN_POINT('Ctrl Pts',(-3.97259050695435,-6.84372398100208,
2.96778304378895));
#66663=CARTESIAN_POINT('Ctrl Pts',(-4.76752217581276,-6.35713512157041,
2.932886150135));
#66664=CARTESIAN_POINT('Ctrl Pts',(-5.34635665456707,-5.8786746103773,2.9085708611738));
#66665=CARTESIAN_POINT('Ctrl Pts',(-5.97664321400985,-5.18645732853546,
2.8756797597553));
#66666=CARTESIAN_POINT('Ctrl Pts',(-6.09877210602362,-5.04227892096413,
2.86890288269143));
#66667=CARTESIAN_POINT('Ctrl Pts',(-6.28072062752146,-4.81118951116262,
2.85792050089018));
#66668=CARTESIAN_POINT('Ctrl Pts',(-6.34416416012781,-4.72721648111431,
2.85390618576162));
#66669=CARTESIAN_POINT('Ctrl Pts',(-6.43418790302885,-4.60298481864827,
2.84789425920229));
#66670=CARTESIAN_POINT('Ctrl Pts',(-6.46210668868853,-4.56370684563079,
2.84598312214154));
#66671=CARTESIAN_POINT('Ctrl Pts',(-6.49409156755445,-4.51782642904247,
2.84373575157979));
#66672=CARTESIAN_POINT('Ctrl Pts',(-6.49850947689704,-4.51146932931417,
2.84342402907383));
#66673=CARTESIAN_POINT('Ctrl Pts',(-6.50523745335268,-4.50175779711832,
2.84294730056086));
#66674=CARTESIAN_POINT('Ctrl Pts',(-6.50755426570889,-4.49840805920864,
2.84278277184036));
#66675=CARTESIAN_POINT('Ctrl Pts',(-6.5117735869608,-4.49229751839385,2.84248247257348));
#66676=CARTESIAN_POINT('Ctrl Pts',(-6.51367693090283,-4.48953729034141,
2.84234676004748));
#66677=CARTESIAN_POINT('Ctrl Pts',(-6.51778667962103,-4.48356922077212,
2.84205319345133));
#66678=CARTESIAN_POINT('Ctrl Pts',(-6.51999247127112,-4.48036096011981,
2.84189529722315));
#66679=CARTESIAN_POINT('Ctrl Pts',(-6.52596120398778,-4.4716658673442,2.84146714100703));
#66680=CARTESIAN_POINT('Ctrl Pts',(-6.52971958614786,-4.4661759247586,2.84119657009575));
#66681=CARTESIAN_POINT('Ctrl Pts',(-6.54729453417257,-4.44043424833065,
2.83992679894327));
#66682=CARTESIAN_POINT('Ctrl Pts',(-6.56102370695979,-4.42012329272008,
2.83892173512237));
#66683=CARTESIAN_POINT('Ctrl Pts',(-6.77700847681125,-4.09737169983901,
2.82290499672281));
#66684=CARTESIAN_POINT('Ctrl Pts',(-6.95824084589083,-3.78141978208877,
2.8066064321629));
#66685=CARTESIAN_POINT('Ctrl Pts',(-7.34232088910019,-2.99004645780602,
2.76634140042128));
#66686=CARTESIAN_POINT('Ctrl Pts',(-7.52164893681742,-2.50497779403031,
2.74218312004849));
#66687=CARTESIAN_POINT('Ctrl Pts',(-7.69981614148297,-1.82527241729796,
2.71091799803428));
#66688=CARTESIAN_POINT('Ctrl Pts',(-7.74075411332836,-1.64302144571686,
2.70276385629693));
#66689=CARTESIAN_POINT('Ctrl Pts',(-7.80783294921315,-1.28566805199094,
2.68725779053315));
#66690=CARTESIAN_POINT('Ctrl Pts',(-7.83462354931685,-1.11080009069451,
2.67989048892087));
#66691=CARTESIAN_POINT('Ctrl Pts',(-7.8593221719404,-0.903329603047026,
2.67140403945952));
#66692=CARTESIAN_POINT('Ctrl Pts',(-7.86291938884934,-0.871463189056676,
2.67010755803925));
#66693=CARTESIAN_POINT('Ctrl Pts',(-7.86742142293673,-0.829281810804904,
2.66840053167805));
#66694=CARTESIAN_POINT('Ctrl Pts',(-7.86849987235438,-0.818985914177716,
2.66798458758142));
#66695=CARTESIAN_POINT('Ctrl Pts',(-7.87023453339471,-0.80210546403663,
2.66730380401011));
#66696=CARTESIAN_POINT('Ctrl Pts',(-7.87090269718427,-0.795522166759528,
2.66703859313565));
#66697=CARTESIAN_POINT('Ctrl Pts',(-7.87217935334179,-0.782784437686145,
2.66652601040819));
#66698=CARTESIAN_POINT('Ctrl Pts',(-7.8727888901592,-0.77663011676877,2.66627860627157));
#66699=CARTESIAN_POINT('Ctrl Pts',(-7.87417650102444,-0.762450289938069,
2.66570915865352));
#66700=CARTESIAN_POINT('Ctrl Pts',(-7.87494952392045,-0.754424290507175,
2.66538727226171));
#66701=CARTESIAN_POINT('Ctrl Pts',(-7.8769823814999,-0.732974318159018,
2.6645281539418));
#66702=CARTESIAN_POINT('Ctrl Pts',(-7.87822017326152,-0.719548256502081,
2.6639916063435));
#66703=CARTESIAN_POINT('Ctrl Pts',(-7.88647634114548,-0.627419536763525,
2.6603179848463));
#66704=CARTESIAN_POINT('Ctrl Pts',(-7.89234969238837,-0.548617474275349,
2.65721652641348));
#66705=CARTESIAN_POINT('Ctrl Pts',(-7.89925256520858,-0.432569512619185,
2.65270539816774));
#66706=CARTESIAN_POINT('Ctrl Pts',(-7.90120109106163,-0.395384414709395,
2.65126837136832));
#66707=CARTESIAN_POINT('Ctrl Pts',(-7.90409180081347,-0.331604948878667,
2.64881755839694));
#66708=CARTESIAN_POINT('Ctrl Pts',(-7.90516246252931,-0.30501720377632,
2.64780004328332));
#66709=CARTESIAN_POINT('Ctrl Pts',(-7.90941321556983,-0.184313441106155,
2.64319896469569));
#66710=CARTESIAN_POINT('Ctrl Pts',(-7.91104687283901,-0.090149221173572,
2.6396600503638));
#66711=CARTESIAN_POINT('Ctrl Pts',(-7.91090043088205,0.197783711785378,
2.62897232910267));
#66712=CARTESIAN_POINT('Ctrl Pts',(-7.90368344506989,0.391479553338397,
2.62196911778459));
#66713=CARTESIAN_POINT('Ctrl Pts',(-7.83360410443304,1.33702722556193,2.58830171568523));
#66714=CARTESIAN_POINT('Ctrl Pts',(-7.67054236727053,2.07737074208001,2.56390246919381));
#66715=CARTESIAN_POINT('Ctrl Pts',(-7.38098275117619,2.84776302298358,2.53195489733808));
#66716=CARTESIAN_POINT('Ctrl Pts',(-7.3559215824904,2.91188560715957,2.52924061533081));
#66717=CARTESIAN_POINT('Ctrl Pts',(-7.32639570807193,2.98461725333508,2.52609028782147));
#66718=CARTESIAN_POINT('Ctrl Pts',(-7.32274766067037,2.99355656649625,2.52570184461408));
#66719=CARTESIAN_POINT('Ctrl Pts',(-7.31738022512135,3.00664061305569,2.52513144800519));
#66720=CARTESIAN_POINT('Ctrl Pts',(-7.31567364939421,3.01079062548021,2.52495025584307));
#66721=CARTESIAN_POINT('Ctrl Pts',(-7.31264053572508,3.01814867866673,2.52462851035576));
#66722=CARTESIAN_POINT('Ctrl Pts',(-7.31131541343025,3.02135730700736,2.52448804183294));
#66723=CARTESIAN_POINT('Ctrl Pts',(-7.30854297254269,3.02805794318884,2.52419435281525));
#66724=CARTESIAN_POINT('Ctrl Pts',(-7.30709526607084,3.03154977879059,2.52404110936979));
#66725=CARTESIAN_POINT('Ctrl Pts',(-7.30330907022856,3.04066352943553,2.5236406315867));
#66726=CARTESIAN_POINT('Ctrl Pts',(-7.30096659568248,3.04628377582745,2.52339315911423));
#66727=CARTESIAN_POINT('Ctrl Pts',(-7.29077549824852,3.07065577093975,2.52231782254121));
#66728=CARTESIAN_POINT('Ctrl Pts',(-7.28286116320372,3.08937979100684,2.52148607870905));
#66729=CARTESIAN_POINT('Ctrl Pts',(-7.1875282475584,3.31251967234924,2.51150879781683));
#66730=CARTESIAN_POINT('Ctrl Pts',(-7.09160778362345,3.51318005866237,2.50188465827764));
#66731=CARTESIAN_POINT('Ctrl Pts',(-6.80248448454122,4.05778221343971,2.47446765944818));
#66732=CARTESIAN_POINT('Ctrl Pts',(-6.59182146172717,4.39172769546328,2.45617814284535));
#66733=CARTESIAN_POINT('Ctrl Pts',(-6.00621276690245,5.18237120887278,2.41113207155075));
#66734=CARTESIAN_POINT('Ctrl Pts',(-5.60336842861333,5.61551544528882,2.38493884658187));
#66735=CARTESIAN_POINT('Ctrl Pts',(-5.12639249907694,6.02540888216721,2.35932354004985));
#66736=CARTESIAN_POINT('Ctrl Pts',(-5.09652529637467,6.05069270515896,2.35773870909082));
#66737=CARTESIAN_POINT('Ctrl Pts',(-5.05753268577517,6.08320800186725,2.35569416201859));
#66738=CARTESIAN_POINT('Ctrl Pts',(-5.04857746838279,6.09064216720154,2.35522626205605));
#66739=CARTESIAN_POINT('Ctrl Pts',(-5.03481659835367,6.10201453812305,2.3545098065588));
#66740=CARTESIAN_POINT('Ctrl Pts',(-5.03002267565726,6.10596687553497,2.35426068242709));
#66741=CARTESIAN_POINT('Ctrl Pts',(-5.02099045769576,6.11339560899103,2.35379219067829));
#66742=CARTESIAN_POINT('Ctrl Pts',(-5.01675319759292,6.11687325378643,2.35357277296644));
#66743=CARTESIAN_POINT('Ctrl Pts',(-5.00704401041266,6.1248249964528,2.35307083560828));
#66744=CARTESIAN_POINT('Ctrl Pts',(-5.00156969125374,6.12929617356259,2.35278843311107));
#66745=CARTESIAN_POINT('Ctrl Pts',(-4.98649143065941,6.14157776550707,2.3520122516251));
#66746=CARTESIAN_POINT('Ctrl Pts',(-4.97687511952548,6.14937299927664,2.35151907985435));
#66747=CARTESIAN_POINT('Ctrl Pts',(-4.92582803772797,6.19055492798307,2.34891085951436));
#66748=CARTESIAN_POINT('Ctrl Pts',(-4.88407906257168,6.22354593642434,2.3468115819914));
#66749=CARTESIAN_POINT('Ctrl Pts',(-4.7672221738974,6.31398883347697,2.3410271497152));
#66750=CARTESIAN_POINT('Ctrl Pts',(-4.69141141161012,6.37051975503729,2.33737785952797));
#66751=CARTESIAN_POINT('Ctrl Pts',(-4.47404734589596,6.52661983411752,2.32718936707845));
#66752=CARTESIAN_POINT('Ctrl Pts',(-4.33021297689338,6.6229242418097,2.32076936232157));
#66753=CARTESIAN_POINT('Ctrl Pts',(-3.56005813576383,7.10275784842637,2.28781164904871));
#66754=CARTESIAN_POINT('Ctrl Pts',(-2.8858346125184,7.40236329522394,2.26409867194546));
#66755=CARTESIAN_POINT('Ctrl Pts',(-2.05456376408631,7.64066249596872,2.23273018666935));
#66756=CARTESIAN_POINT('Ctrl Pts',(-1.92823373080248,7.6735173137064,2.22789728491863));
#66757=CARTESIAN_POINT('Ctrl Pts',(-1.79187482110973,7.70540047150329,2.2225581134677));
#66758=CARTESIAN_POINT('Ctrl Pts',(-1.78259225512469,7.70755322081026,2.22219404569177));
#66759=CARTESIAN_POINT('Ctrl Pts',(-1.76496239083467,7.71160826644694,2.22150140456071));
#66760=CARTESIAN_POINT('Ctrl Pts',(-1.75661584453204,7.71351379528824,2.22117298126222));
#66761=CARTESIAN_POINT('Ctrl Pts',(-1.7378146952725,7.7177740267806,2.22043201837602));
#66762=CARTESIAN_POINT('Ctrl Pts',(-1.72735838194081,7.72012103935042,2.22001911755073));
#66763=CARTESIAN_POINT('Ctrl Pts',(-1.64157668157672,7.73919250462231,2.21662487028983));
#66764=CARTESIAN_POINT('Ctrl Pts',(-1.56601723034388,7.75483487634673,2.21359160729075));
#66765=CARTESIAN_POINT('Ctrl Pts',(-1.4805930848233,7.7712200889489,2.21010176978536));
#66766=CARTESIAN_POINT('Ctrl Pts',(-1.47093942835568,7.7730531163893,2.20970651942825));
#66767=CARTESIAN_POINT('Ctrl Pts',(-1.45689889186557,7.77569202791625,2.20913036254567));
#66768=CARTESIAN_POINT('Ctrl Pts',(-1.45251467405962,7.77651220121256,2.20895027174178));
#66769=CARTESIAN_POINT('Ctrl Pts',(-1.44478197119958,7.77795202171177,2.2086323081849));
#66770=CARTESIAN_POINT('Ctrl Pts',(-1.44143377180702,7.77857321607112,2.20849452446221));
#66771=CARTESIAN_POINT('Ctrl Pts',(-1.4345174880602,7.77985178135427,2.20820968349918));
#66772=CARTESIAN_POINT('Ctrl Pts',(-1.43094935118121,7.78050885981514,2.20806260938227));
#66773=CARTESIAN_POINT('Ctrl Pts',(-1.42181068094513,7.78218526234554,2.20768560566028));
#66774=CARTESIAN_POINT('Ctrl Pts',(-1.41623954809576,7.7832010517458,2.20745547124208));
#66775=CARTESIAN_POINT('Ctrl Pts',(-1.39291826733194,7.78742737206569,2.20649083398231));
#66776=CARTESIAN_POINT('Ctrl Pts',(-1.37515840835317,7.79058314353882,2.20575315620827));
#66777=CARTESIAN_POINT('Ctrl Pts',(-1.25363013962849,7.81174914723672,2.20068508373344));
#66778=CARTESIAN_POINT('Ctrl Pts',(-1.14952581524441,7.82774564309514,2.19624284960392));
#66779=CARTESIAN_POINT('Ctrl Pts',(-0.891369157628512,7.86215280926732,
2.18503411193041));
#66780=CARTESIAN_POINT('Ctrl Pts',(-0.737037383336073,7.87811890637888,
2.17816482037906));
#66781=CARTESIAN_POINT('Ctrl Pts',(-0.18858277653159,7.91860149865178,2.15339534770232));
#66782=CARTESIAN_POINT('Ctrl Pts',(0.206795517166995,7.91814653931338,2.1349170390916));
#66783=CARTESIAN_POINT('Ctrl Pts',(1.17516282775335,7.84443012758718,2.09022089405342));
#66784=CARTESIAN_POINT('Ctrl Pts',(1.74341202609434,7.73800952994934,2.06459980023237));
#66785=CARTESIAN_POINT('Ctrl Pts',(2.33278967875018,7.55933612796605,2.03952453445194));
#66786=CARTESIAN_POINT('Ctrl Pts',(2.37037352394977,7.5476353779152,2.03793133286367));
#66787=CARTESIAN_POINT('Ctrl Pts',(2.41872340293825,7.5321861335829,2.03588906901936));
#66788=CARTESIAN_POINT('Ctrl Pts',(2.42957048096277,7.52869431776472,2.03543137258639));
#66789=CARTESIAN_POINT('Ctrl Pts',(2.44677075590514,7.52311628131994,2.03470634970607));
#66790=CARTESIAN_POINT('Ctrl Pts',(2.45312889720443,7.52104542787811,2.03443850513224));
#66791=CARTESIAN_POINT('Ctrl Pts',(2.46501458808005,7.51715757022761,2.03393810814981));
#66792=CARTESIAN_POINT('Ctrl Pts',(2.47054277092266,7.51534252528196,2.03370548978492));
#66793=CARTESIAN_POINT('Ctrl Pts',(2.48296324597073,7.5112493775946,2.03318312711714));
#66794=CARTESIAN_POINT('Ctrl Pts',(2.48985441946781,7.50896788270431,2.03289349770266));
#66795=CARTESIAN_POINT('Ctrl Pts',(2.51005635140208,7.50224866169681,2.0320449826566));
#66796=CARTESIAN_POINT('Ctrl Pts',(2.52335848766041,7.49778499388771,2.0314869751491));
#66797=CARTESIAN_POINT('Ctrl Pts',(2.62192183698695,7.46441904520914,2.0273575211887));
#66798=CARTESIAN_POINT('Ctrl Pts',(2.70669762333801,7.43409809328792,2.02383445619594));
#66799=CARTESIAN_POINT('Ctrl Pts',(2.9788232352709,7.33149723114966,2.01260737217662));
#66800=CARTESIAN_POINT('Ctrl Pts',(3.16394797762751,7.25352873788172,2.00509866171235));
#66801=CARTESIAN_POINT('Ctrl Pts',(3.67797896795766,7.01360684268325,1.9844354395639));
#66802=CARTESIAN_POINT('Ctrl Pts',(3.99888278040356,6.83572690408658,1.97177831166398));
#66803=CARTESIAN_POINT('Ctrl Pts',(4.80589812982396,6.31204843409116,1.93883363853392));
#66804=CARTESIAN_POINT('Ctrl Pts',(5.26722033216891,5.93252200391318,1.91888323186619));
#66805=CARTESIAN_POINT('Ctrl Pts',(5.70277741203841,5.48299029916984,1.89410432302098));
#66806=CARTESIAN_POINT('Ctrl Pts',(5.72389170376333,5.46094465706556,1.89288631522391));
#66807=CARTESIAN_POINT('Ctrl Pts',(5.74930655088799,5.43409943644993,1.89139893042648));
#66808=CARTESIAN_POINT('Ctrl Pts',(5.75372977312431,5.42941582481192,1.89113927675374));
#66809=CARTESIAN_POINT('Ctrl Pts',(5.76097090209258,5.42172963374268,1.89071290170691));
#66810=CARTESIAN_POINT('Ctrl Pts',(5.76379220076254,5.41873024078939,1.89054645153968));
#66811=CARTESIAN_POINT('Ctrl Pts',(5.76884477963886,5.41335030771621,1.89024777440034));
#66812=CARTESIAN_POINT('Ctrl Pts',(5.77107693328892,5.41097058535856,1.89011561768633));
#66813=CARTESIAN_POINT('Ctrl Pts',(5.77576536774285,5.40596599508891,1.88983760041001));
#66814=CARTESIAN_POINT('Ctrl Pts',(5.77822132533042,5.40334084049854,1.88969171453592));
#66815=CARTESIAN_POINT('Ctrl Pts',(5.78478007051951,5.39632066179451,1.88930144978534));
#66816=CARTESIAN_POINT('Ctrl Pts',(5.78887963297001,5.39192263889081,1.88905681210221));
#66817=CARTESIAN_POINT('Ctrl Pts',(5.79788755943404,5.38223679351104,1.88851773595793));
#66818=CARTESIAN_POINT('Ctrl Pts',(5.80279370685935,5.37694692629812,1.88822312253327));
#66819=CARTESIAN_POINT('Ctrl Pts',(5.81737742326499,5.36117938077445,1.88734439219395));
#66820=CARTESIAN_POINT('Ctrl Pts',(5.82703385505538,5.35068228214799,1.88675863296099));
#66821=CARTESIAN_POINT('Ctrl Pts',(6.12759115350671,5.02218059617028,1.86840585500462));
#66822=CARTESIAN_POINT('Ctrl Pts',(6.39202193788916,4.68098840293117,1.84873902271576));
#66823=CARTESIAN_POINT('Ctrl Pts',(7.0010036513548,3.74674900432866,1.7969424353437));
#66824=CARTESIAN_POINT('Ctrl Pts',(7.29878758828355,3.12732228295483,1.76475584871739));
#66825=CARTESIAN_POINT('Ctrl Pts',(7.57441046011432,2.29140249793099,1.72711905801443));
#66826=CARTESIAN_POINT('Ctrl Pts',(7.62877695007623,2.10332806109193,1.71897514442353));
#66827=CARTESIAN_POINT('Ctrl Pts',(7.6806555245116,1.89520556203789,1.71030479795432));
#66828=CARTESIAN_POINT('Ctrl Pts',(7.68513118053164,1.87697420149655,1.70954809981223));
#66829=CARTESIAN_POINT('Ctrl Pts',(7.69132590388351,1.85134666988387,1.70848834289437));
#66830=CARTESIAN_POINT('Ctrl Pts',(7.69309926420538,1.84396376410596,1.7081834992438));
#66831=CARTESIAN_POINT('Ctrl Pts',(7.69615801959283,1.83114824703942,1.70765512933721));
#66832=CARTESIAN_POINT('Ctrl Pts',(7.69744829692394,1.82571681307334,1.70743144284098));
#66833=CARTESIAN_POINT('Ctrl Pts',(7.70012067210099,1.81441423480567,1.70696647050967));
#66834=CARTESIAN_POINT('Ctrl Pts',(7.70150180715093,1.80854286514025,1.70672521637794));
#66835=CARTESIAN_POINT('Ctrl Pts',(7.70473725186795,1.79471768837487,1.70615781159063));
#66836=CARTESIAN_POINT('Ctrl Pts',(7.70658596375103,1.78676257100049,1.70583184454492));
#66837=CARTESIAN_POINT('Ctrl Pts',(7.71258380128167,1.76077103421638,1.7047685190822));
#66838=CARTESIAN_POINT('Ctrl Pts',(7.71668196773315,1.74272285279694,1.70403282834968));
#66839=CARTESIAN_POINT('Ctrl Pts',(7.77957341712086,1.46117926570953,1.69259751136017));
#66840=CARTESIAN_POINT('Ctrl Pts',(7.82490656094049,1.19484758577534,1.68235009178677));
#66841=CARTESIAN_POINT('Ctrl Pts',(7.89337246717776,0.614396892602981,1.66092572130965));
#66842=CARTESIAN_POINT('Ctrl Pts',(7.91155649071522,0.300164557838142,1.64989621615588));
#66843=CARTESIAN_POINT('Ctrl Pts',(7.90981910850575,-0.659320240013322,
1.61671123026394));
#66844=CARTESIAN_POINT('Ctrl Pts',(7.82977573982341,-1.30167271186645,1.59527636254536));
#66845=CARTESIAN_POINT('Ctrl Pts',(7.66264358999745,-1.96710876236341,1.56825099224333));
#66846=CARTESIAN_POINT('Ctrl Pts',(7.65227916836112,-2.00704935099972,1.56660935769269));
#66847=CARTESIAN_POINT('Ctrl Pts',(7.63939039118805,-2.05516631254114,1.56460948267511));
#66848=CARTESIAN_POINT('Ctrl Pts',(7.63716448183387,-2.06342259311515,1.56426553800746));
#66849=CARTESIAN_POINT('Ctrl Pts',(7.63350075683849,-2.07692483803282,1.56370177716505));
#66850=CARTESIAN_POINT('Ctrl Pts',(7.63207090561242,-2.0821729704611,1.56348233532205));
#66851=CARTESIAN_POINT('Ctrl Pts',(7.629527042067,-2.09147215292516,1.56309295027046));
#66852=CARTESIAN_POINT('Ctrl Pts',(7.62841521134831,-2.09552380450841,1.5629231083048));
#66853=CARTESIAN_POINT('Ctrl Pts',(7.62606420325262,-2.10406450829294,1.56256469716655));
#66854=CARTESIAN_POINT('Ctrl Pts',(7.62482428896246,-2.10855335467245,1.56237609415065));
#66855=CARTESIAN_POINT('Ctrl Pts',(7.62157106104263,-2.12029058244908,1.56188235084967));
#66856=CARTESIAN_POINT('Ctrl Pts',(7.61955137380321,-2.12753718039163,1.56157692065343));
#66857=CARTESIAN_POINT('Ctrl Pts',(7.61510995586803,-2.143385456197,1.56090766672895));
#66858=CARTESIAN_POINT('Ctrl Pts',(7.61268398284403,-2.15198592704694,1.560543653489));
#66859=CARTESIAN_POINT('Ctrl Pts',(7.60552401597372,-2.1772055599211,1.55947384907795));
#66860=CARTESIAN_POINT('Ctrl Pts',(7.60075015419546,-2.19381327705722,1.55876631214438));
#66861=CARTESIAN_POINT('Ctrl Pts',(7.58408298194358,-2.25108899448655,1.55631596955899));
#66862=CARTESIAN_POINT('Ctrl Pts',(7.5719175037975,-2.29167658332965,1.55456173652297));
#66863=CARTESIAN_POINT('Ctrl Pts',(7.51736853738067,-2.46849044476569,1.54684697758201));
#66864=CARTESIAN_POINT('Ctrl Pts',(7.47163158996922,-2.60365003391587,1.54076086466285));
#66865=CARTESIAN_POINT('Ctrl Pts',(7.35115954333056,-2.93029025326666,1.52569466993713));
#66866=CARTESIAN_POINT('Ctrl Pts',(7.2725686335105,-3.12023868300716,1.516627475259));
#66867=CARTESIAN_POINT('Ctrl Pts',(6.87354471296583,-3.98740996724609,1.47429809241824));
#66868=CARTESIAN_POINT('Ctrl Pts',(6.46529365065728,-4.62009900714643,1.44117517092932));
#66869=CARTESIAN_POINT('Ctrl Pts',(5.94407549555546,-5.22053519497322,1.40883941943225));
#66870=CARTESIAN_POINT('Ctrl Pts',(5.91373322941831,-5.25488159456848,1.40698422770056));
#66871=CARTESIAN_POINT('Ctrl Pts',(5.87256887603593,-5.30067011224025,1.40450299228025));
#66872=CARTESIAN_POINT('Ctrl Pts',(5.86200880568694,-5.31234614903184,1.40386956960724));
#66873=CARTESIAN_POINT('Ctrl Pts',(5.8453983445093,-5.33060213234659,1.40287804094524));
#66874=CARTESIAN_POINT('Ctrl Pts',(5.83937155426294,-5.33720345790456,1.40251927010259));
#66875=CARTESIAN_POINT('Ctrl Pts',(5.82778764329796,-5.34984855793779,1.40183156962037));
#66876=CARTESIAN_POINT('Ctrl Pts',(5.82223227783044,-5.3558939227364,1.40150259109513));
#66877=CARTESIAN_POINT('Ctrl Pts',(5.80920940520938,-5.37002124461455,1.40073332371105));
#66878=CARTESIAN_POINT('Ctrl Pts',(5.80173442016159,-5.37809629887392,1.40029324620418));
#66879=CARTESIAN_POINT('Ctrl Pts',(5.78033645266236,-5.4011155023088,1.39903766976062));
#66880=CARTESIAN_POINT('Ctrl Pts',(5.76637237913592,-5.4160213963549,1.39822334255135));
#66881=CARTESIAN_POINT('Ctrl Pts',(5.67656728734826,-5.51114245201953,1.39301838556512));
#66882=CARTESIAN_POINT('Ctrl Pts',(5.59911086875452,-5.58981803066453,1.38867520781155));
#66883=CARTESIAN_POINT('Ctrl Pts',(5.36789261565527,-5.81504589609741,1.37611634827837));
#66884=CARTESIAN_POINT('Ctrl Pts',(5.20984355800252,-5.95706011680667,1.36803777709649));
#66885=CARTESIAN_POINT('Ctrl Pts',(4.74733624604546,-6.34014048954591,1.34560570135726));
#66886=CARTESIAN_POINT('Ctrl Pts',(4.43058417981132,-6.5654029178304,1.33164555352016));
#66887=CARTESIAN_POINT('Ctrl Pts',(3.73760325290378,-6.98515223639266,1.30241278465072));
#66888=CARTESIAN_POINT('Ctrl Pts',(3.35973445799983,-7.17454995580319,1.28717411846075));
#66889=CARTESIAN_POINT('Ctrl Pts',(2.90200442161702,-7.35985412200094,1.2679037073622));
#66890=CARTESIAN_POINT('Ctrl Pts',(2.83504904818616,-7.38590406187277,1.26506461942681));
#66891=CARTESIAN_POINT('Ctrl Pts',(2.7571310664331,-7.41500355789432,1.26172849785012));
#66892=CARTESIAN_POINT('Ctrl Pts',(2.74650399639461,-7.41894637242531,1.26127280229689));
#66893=CARTESIAN_POINT('Ctrl Pts',(2.73071053210617,-7.42476741783605,1.26059450114377));
#66894=CARTESIAN_POINT('Ctrl Pts',(2.72555056408974,-7.42666313639438,1.26037272079089));
#66895=CARTESIAN_POINT('Ctrl Pts',(2.71652082347185,-7.42996989104575,1.25998431246967));
#66896=CARTESIAN_POINT('Ctrl Pts',(2.71265191277623,-7.43138328753252,1.25981779712084));
#66897=CARTESIAN_POINT('Ctrl Pts',(2.7044871926356,-7.43435881022194,1.25946618591878));
#66898=CARTESIAN_POINT('Ctrl Pts',(2.70019113089328,-7.43592023563773,1.25928105648296));
#66899=CARTESIAN_POINT('Ctrl Pts',(2.6891100688137,-7.43993683454291,1.25880322557751));
#66900=CARTESIAN_POINT('Ctrl Pts',(2.68232306885573,-7.44238644642539,1.25851025474875));
#66901=CARTESIAN_POINT('Ctrl Pts',(2.66760772934499,-7.44767486668801,1.25787436586238));
#66902=CARTESIAN_POINT('Ctrl Pts',(2.65967819566742,-7.45051030548828,1.25753128269091));
#66903=CARTESIAN_POINT('Ctrl Pts',(2.63684564945331,-7.45863366061509,1.25654213423054));
#66904=CARTESIAN_POINT('Ctrl Pts',(2.62193135279596,-7.46388953814629,1.25589447110958));
#66905=CARTESIAN_POINT('Ctrl Pts',(2.57234896496281,-7.48119568585069,1.25373591182469));
#66906=CARTESIAN_POINT('Ctrl Pts',(2.53761431252072,-7.4930488896003,1.25221481697049));
#66907=CARTESIAN_POINT('Ctrl Pts',(2.38740440631949,-7.54314375160728,1.2455963752325));
#66908=CARTESIAN_POINT('Ctrl Pts',(2.27114407840564,-7.57895900227316,1.24037429642332));
#66909=CARTESIAN_POINT('Ctrl Pts',(2.05287139227233,-7.64072705638989,1.2304463449608));
#66910=CARTESIAN_POINT('Ctrl Pts',(1.95107447212419,-7.66735274599372,1.22576686669231));
#66911=CARTESIAN_POINT('Ctrl Pts',(0.927843377872795,-7.91328927259855,
1.17843672060966));
#66912=CARTESIAN_POINT('Ctrl Pts',(-0.0257557132769284,-7.96751163361469,
1.13318083180045));
#66913=CARTESIAN_POINT('Ctrl Pts',(-1.02127807460617,-7.84499730013908,
1.09208424949607));
#66914=CARTESIAN_POINT('Ctrl Pts',(-1.07620374946437,-7.8376512554759,1.08983249307969));
#66915=CARTESIAN_POINT('Ctrl Pts',(-1.14257068903076,-7.8280641765508,1.08713026245907));
#66916=CARTESIAN_POINT('Ctrl Pts',(-1.15408924000219,-7.8263742920518,1.08666194505183));
#66917=CARTESIAN_POINT('Ctrl Pts',(-1.17295832777921,-7.82356344940469,
1.08589587639087));
#66918=CARTESIAN_POINT('Ctrl Pts',(-1.18031106883719,-7.82245754649716,
1.08559763645871));
#66919=CARTESIAN_POINT('Ctrl Pts',(-1.19348177870301,-7.82045758838228,
1.08506390035953));
#66920=CARTESIAN_POINT('Ctrl Pts',(-1.19930032437965,-7.81956740363072,
1.08482827854389));
#66921=CARTESIAN_POINT('Ctrl Pts',(-1.21162604848919,-7.81766759853267,
1.0843295113037));
#66922=CARTESIAN_POINT('Ctrl Pts',(-1.21813297283708,-7.8166563454773,1.0840664192081));
#66923=CARTESIAN_POINT('Ctrl Pts',(-1.23545458614173,-7.8139422075249,1.08336662881469));
#66924=CARTESIAN_POINT('Ctrl Pts',(-1.24626703363144,-7.81222499286318,
1.08293039753233));
#66925=CARTESIAN_POINT('Ctrl Pts',(-1.29652321065315,-7.80413640082477,
1.08090552123602));
#66926=CARTESIAN_POINT('Ctrl Pts',(-1.33592221084362,-7.7974886538103,1.07932590098434));
#66927=CARTESIAN_POINT('Ctrl Pts',(-1.62809948587043,-7.7459104099924,1.06766791844162));
#66928=CARTESIAN_POINT('Ctrl Pts',(-1.87861681302469,-7.68899531425484,
1.05799268345513));
#66929=CARTESIAN_POINT('Ctrl Pts',(-2.51712944630752,-7.5108536480039,1.03386666648871));
#66930=CARTESIAN_POINT('Ctrl Pts',(-2.89934727401863,-7.37174803807389,
1.01997259875936));
#66931=CARTESIAN_POINT('Ctrl Pts',(-3.42574524311268,-7.13286363509513,
1.00036078557428));
#66932=CARTESIAN_POINT('Ctrl Pts',(-3.5799317212013,-7.05673878914083,0.99454802385252));
#66933=CARTESIAN_POINT('Ctrl Pts',(-3.91319750011234,-6.87846353217755,
0.981627354904344));
#66934=CARTESIAN_POINT('Ctrl Pts',(-4.09100892432498,-6.7742170113582,0.974496716787072));
#66935=CARTESIAN_POINT('Ctrl Pts',(-4.40109634795412,-6.57575525997807,
0.961305585218286));
#66936=CARTESIAN_POINT('Ctrl Pts',(-4.53492561757346,-6.4841846990211,0.955343457574303));
#66937=CARTESIAN_POINT('Ctrl Pts',(-4.74183583189245,-6.33306953341771,
0.945542051319331));
#66938=CARTESIAN_POINT('Ctrl Pts',(-4.81683176177043,-6.27621759073707,
0.941862203444714));
#66939=CARTESIAN_POINT('Ctrl Pts',(-4.89791869603541,-6.21243878340461,
0.937721386082936));
#66940=CARTESIAN_POINT('Ctrl Pts',(-4.90503482280005,-6.20682177739849,
0.937356599447361));
#66941=CARTESIAN_POINT('Ctrl Pts',(-4.91556323266419,-6.19848192409276,
0.936814802780212));
#66942=CARTESIAN_POINT('Ctrl Pts',(-4.91898296271878,-6.19576844870096,
0.936638494441916));
#66943=CARTESIAN_POINT('Ctrl Pts',(-4.92483821928573,-6.19111453705791,
0.936336054851823));
#66944=CARTESIAN_POINT('Ctrl Pts',(-4.92727485126152,-6.18917548928605,
0.936210028530215));
#66945=CARTESIAN_POINT('Ctrl Pts',(-4.93203049294346,-6.18538640806916,
0.935963732861911));
#66946=CARTESIAN_POINT('Ctrl Pts',(-4.93434960847619,-6.18353650767301,
0.935843473508284));
#66947=CARTESIAN_POINT('Ctrl Pts',(-4.93914824708803,-6.17970433522073,
0.935594323276705));
#66948=CARTESIAN_POINT('Ctrl Pts',(-4.94162761886262,-6.17772187411384,
0.935465418269891));
#66949=CARTESIAN_POINT('Ctrl Pts',(-4.94727535728616,-6.17320046847667,
0.935171392606627));
#66950=CARTESIAN_POINT('Ctrl Pts',(-4.95044296122101,-6.17066057828451,
0.935006201648206));
#66951=CARTESIAN_POINT('Ctrl Pts',(-4.96609302198877,-6.15809203266822,
0.93418865538541));
#66952=CARTESIAN_POINT('Ctrl Pts',(-4.9785468850579,-6.1480280002567,0.933533689045903));
#66953=CARTESIAN_POINT('Ctrl Pts',(-5.13541759084523,-6.02047075184343,
0.925229126891528));
#66954=CARTESIAN_POINT('Ctrl Pts',(-5.27566483766739,-5.89796009111895,
0.917220389129484));
#66955=CARTESIAN_POINT('Ctrl Pts',(-5.50066023271181,-5.68696886726174,
0.903577190709815));
#66956=CARTESIAN_POINT('Ctrl Pts',(-5.58791566751331,-5.60125652928248,
0.898072169212023));
#66957=CARTESIAN_POINT('Ctrl Pts',(-6.22182442970545,-4.94899951916871,
0.856684368956515));
#66958=CARTESIAN_POINT('Ctrl Pts',(-6.68329652895918,-4.30553807599008,
0.819208773506188));
#66959=CARTESIAN_POINT('Ctrl Pts',(-7.12258477876593,-3.44730283969861,
0.778240032815006));
#66960=CARTESIAN_POINT('Ctrl Pts',(-7.19776856344398,-3.28743729392084,
0.770917695881308));
#66961=CARTESIAN_POINT('Ctrl Pts',(-7.27415499052423,-3.10980231314302,
0.763108373812415));
#66962=CARTESIAN_POINT('Ctrl Pts',(-7.28071949563079,-3.09440218516111,
0.762433969287101));
#66963=CARTESIAN_POINT('Ctrl Pts',(-7.29036759828207,-3.07156736220434,
0.761437847649765));
#66964=CARTESIAN_POINT('Ctrl Pts',(-7.2934887917746,-3.06414866209062,0.761114824615793));
#66965=CARTESIAN_POINT('Ctrl Pts',(-7.29880023897846,-3.05146989770226,
0.760563794382481));
#66966=CARTESIAN_POINT('Ctrl Pts',(-7.30099613849812,-3.04621221370423,
0.760335591423101));
#66967=CARTESIAN_POINT('Ctrl Pts',(-7.30524696690901,-3.03600337433877,
0.759893071889591));
#66968=CARTESIAN_POINT('Ctrl Pts',(-7.30730254709344,-3.03105249409005,
0.759678732819961));
#66969=CARTESIAN_POINT('Ctrl Pts',(-7.31219067649834,-3.01924552490682,
0.759168203010356));
#66970=CARTESIAN_POINT('Ctrl Pts',(-7.31501861993959,-3.0123875281022,0.758872171771544));
#66971=CARTESIAN_POINT('Ctrl Pts',(-7.32340830906583,-2.99196035961901,
0.757991918077854));
#66972=CARTESIAN_POINT('Ctrl Pts',(-7.32894198962146,-2.97837965521888,
0.757408665433738));
#66973=CARTESIAN_POINT('Ctrl Pts',(-7.37410611594611,-2.86665025942511,
0.752626282645348));
#66974=CARTESIAN_POINT('Ctrl Pts',(-7.41180171080291,-2.76772852961935,
0.748494134567827));
#66975=CARTESIAN_POINT('Ctrl Pts',(-7.55602591054977,-2.36515028115023,
0.732061334349842));
#66976=CARTESIAN_POINT('Ctrl Pts',(-7.64597131931583,-2.05587154157563,
0.720324350296821));
#66977=CARTESIAN_POINT('Ctrl Pts',(-7.84623618187793,-1.1687019970341,0.688197761162855));
#66978=CARTESIAN_POINT('Ctrl Pts',(-7.91134728837762,-0.582879817310929,
0.668873487582277));
#66979=CARTESIAN_POINT('Ctrl Pts',(-7.91099860705843,0.00469458407978809,
0.647721152219829));
#66980=CARTESIAN_POINT('Origin',(0.,0.,183.));
#66981=CARTESIAN_POINT('',(-4.,-4.89858719658941E-16,184.));
#66982=CARTESIAN_POINT('Origin',(0.,0.,184.));
#66983=CARTESIAN_POINT('',(-4.,-4.89858719658941E-16,182.));
#66984=CARTESIAN_POINT('',(-4.,-4.89858719658941E-16,183.));
#66985=CARTESIAN_POINT('Origin',(0.,0.,182.));
#66986=CARTESIAN_POINT('Origin',(8.,0.,182.));
#66987=CARTESIAN_POINT('',(-5.,6.12323399573677E-16,182.));
#66988=CARTESIAN_POINT('Origin',(0.,0.,182.));
#66989=CARTESIAN_POINT('Origin',(4.,0.,184.));
#66990=CARTESIAN_POINT('',(-5.,-6.12323399573677E-16,184.));
#66991=CARTESIAN_POINT('Origin',(0.,0.,184.));
#66992=CARTESIAN_POINT('Origin',(0.,0.,158.));
#66993=CARTESIAN_POINT('',(-5.,-6.12323399573677E-16,185.));
#66994=CARTESIAN_POINT('Origin',(0.,0.,185.));
#66995=CARTESIAN_POINT('',(-5.,-6.12323399573677E-16,158.));
#66996=CARTESIAN_POINT('Origin',(0.,0.,158.));
#66997=CARTESIAN_POINT('',(-5.,-6.12323399573677E-16,158.));
#66998=CARTESIAN_POINT('',(-5.,-6.12323399573677E-16,158.));
#66999=CARTESIAN_POINT('Origin',(0.,0.,158.));
#67000=CARTESIAN_POINT('Origin',(0.,0.,185.));
#67001=CARTESIAN_POINT('Origin',(0.,0.,154.));
#67002=CARTESIAN_POINT('',(-10.,-1.22464679914735E-15,154.));
#67003=CARTESIAN_POINT('Origin',(0.,0.,154.));
#67004=CARTESIAN_POINT('',(6.04416524408958,-3.53101493938209,154.));
#67005=CARTESIAN_POINT('',(-6.07123506171349,-3.48426514564655,154.000000121761));
#67006=CARTESIAN_POINT('Origin',(0.,0.,154.));
#67007=CARTESIAN_POINT('Origin',(-1.40492233861576,-0.171210964340612,153.999999999995));
#67008=CARTESIAN_POINT('Origin',(1.19342779692842,-0.571021005665173,153.999999999995));
#67009=CARTESIAN_POINT('Origin',(0.,0.,154.));
#67010=CARTESIAN_POINT('',(-10.,-1.22464679914735E-15,158.));
#67011=CARTESIAN_POINT('Origin',(0.,0.,158.));
#67012=CARTESIAN_POINT('',(-10.,-1.22464679914735E-15,154.));
#67013=CARTESIAN_POINT('Origin',(0.,0.,158.));
#67014=CARTESIAN_POINT('Origin',(0.,18.,-5.));
#67015=CARTESIAN_POINT('',(-8.,18.,0.));
#67016=CARTESIAN_POINT('Origin',(0.,18.,0.));
#67017=CARTESIAN_POINT('',(-8.,18.,-10.));
#67018=CARTESIAN_POINT('',(-8.,18.,-5.));
#67019=CARTESIAN_POINT('Origin',(0.,18.,-10.));
#67020=CARTESIAN_POINT('Origin',(18.,0.,-5.));
#67021=CARTESIAN_POINT('',(10.,9.79717439317883E-16,0.));
#67022=CARTESIAN_POINT('Origin',(18.,0.,0.));
#67023=CARTESIAN_POINT('',(10.,9.79717439317883E-16,-10.));
#67024=CARTESIAN_POINT('',(10.,9.79717439317883E-16,-5.));
#67025=CARTESIAN_POINT('Origin',(18.,0.,-10.));
#67026=CARTESIAN_POINT('Origin',(-18.,0.,-5.));
#67027=CARTESIAN_POINT('',(-26.,9.79717439317883E-16,0.));
#67028=CARTESIAN_POINT('Origin',(-18.,0.,0.));
#67029=CARTESIAN_POINT('',(-26.,9.79717439317883E-16,-10.));
#67030=CARTESIAN_POINT('',(-26.,9.79717439317883E-16,-5.));
#67031=CARTESIAN_POINT('Origin',(-18.,0.,-10.));
#67032=CARTESIAN_POINT('Origin',(0.,-18.,-5.));
#67033=CARTESIAN_POINT('',(-8.,-18.,0.));
#67034=CARTESIAN_POINT('Origin',(0.,-18.,0.));
#67035=CARTESIAN_POINT('',(-8.,-18.,-10.));
#67036=CARTESIAN_POINT('',(-8.,-18.,-5.));
#67037=CARTESIAN_POINT('Origin',(0.,-18.,-10.));
#67038=CARTESIAN_POINT('Origin',(0.,0.,153.5));
#67039=CARTESIAN_POINT('Ctrl Pts',(-6.07123482803126,-3.48426499407615,
154.000000365283));
#67040=CARTESIAN_POINT('Ctrl Pts',(-6.37729082463053,-2.98510698007377,
153.983009074227));
#67041=CARTESIAN_POINT('Ctrl Pts',(-6.6197085761198,-2.44959580558649,153.965827313444));
#67042=CARTESIAN_POINT('Ctrl Pts',(-6.9846747189001,-1.27750436456966,153.928602162082));
#67043=CARTESIAN_POINT('Ctrl Pts',(-7.0919311032529,-0.639071943781941,
153.908394854784));
#67044=CARTESIAN_POINT('Ctrl Pts',(-7.13926079552257,1.02962958383913,153.860216444196));
#67045=CARTESIAN_POINT('Ctrl Pts',(-6.9390178381147,1.95420836025049,153.839610574055));
#67046=CARTESIAN_POINT('Ctrl Pts',(-6.36073513248416,3.46730423446295,153.798161280371));
#67047=CARTESIAN_POINT('Ctrl Pts',(-5.96341174680285,4.15209317811089,153.775889324813));
#67048=CARTESIAN_POINT('Ctrl Pts',(-4.9660733049039,5.37226764090361,153.726971778021));
#67049=CARTESIAN_POINT('Ctrl Pts',(-4.25430228608747,6.0418766964822,153.69407810596));
#67050=CARTESIAN_POINT('Ctrl Pts',(-2.49085845485886,6.97949242594648,153.642859236));
#67051=CARTESIAN_POINT('Ctrl Pts',(-1.63249269525403,7.24793969981517,153.623916701874));
#67052=CARTESIAN_POINT('Ctrl Pts',(0.0560132140757014,7.46364414088888,
153.580474698423));
#67053=CARTESIAN_POINT('Ctrl Pts',(0.876036956523461,7.43596342213082,153.556771317729));
#67054=CARTESIAN_POINT('Ctrl Pts',(2.26944149094137,7.16065895049613,153.512935028995));
#67055=CARTESIAN_POINT('Ctrl Pts',(3.1051275024235,6.92367809008591,153.484990573071));
#67056=CARTESIAN_POINT('Ctrl Pts',(4.80872094961789,5.91228941939438,153.436000484306));
#67057=CARTESIAN_POINT('Ctrl Pts',(5.51398732222406,5.28896519422956,153.416367441624));
#67058=CARTESIAN_POINT('Ctrl Pts',(6.71662248272036,3.7642603069226,153.367120384876));
#67059=CARTESIAN_POINT('Ctrl Pts',(7.18428961469687,2.85171462781057,153.336756402359));
#67060=CARTESIAN_POINT('Ctrl Pts',(7.6725689600507,1.12984169336891,153.28386581576));
#67061=CARTESIAN_POINT('Ctrl Pts',(7.76711987065858,0.359391098290495,153.263717416961));
#67062=CARTESIAN_POINT('Ctrl Pts',(7.71591129163788,-1.26410811526187,153.226979141127));
#67063=CARTESIAN_POINT('Ctrl Pts',(7.54993713581411,-2.10059887369074,153.208958867732));
#67064=CARTESIAN_POINT('Ctrl Pts',(7.05995918060561,-3.42583218192886,153.173305452414));
#67065=CARTESIAN_POINT('Ctrl Pts',(6.80641914608851,-3.93660409196822,153.157670685671));
#67066=CARTESIAN_POINT('Ctrl Pts',(6.1501911740556,-4.965772420327,153.122315830429));
#67067=CARTESIAN_POINT('Ctrl Pts',(5.73217936663422,-5.47174237691816,153.102402843541));
#67068=CARTESIAN_POINT('Ctrl Pts',(5.25622342069531,-5.91850150513378,153.0844112844));
#67069=CARTESIAN_POINT('Ctrl Pts',(-1.31596378579611,-7.79949774689402,
153.090263860954));
#67070=CARTESIAN_POINT('Ctrl Pts',(-1.1121036545036,-7.81524681765638,153.108651036666));
#67071=CARTESIAN_POINT('Ctrl Pts',(-0.90819989047042,-7.82301474609582,
153.127052284549));
#67072=CARTESIAN_POINT('Ctrl Pts',(-0.704669024892965,-7.82273003893546,
153.145595904417));
#67073=CARTESIAN_POINT('Ctrl Pts',(-0.505071248433598,-7.82245083353834,
153.163781182029));
#67074=CARTESIAN_POINT('Ctrl Pts',(-0.305831889755628,-7.81442791085797,
153.182103714959));
#67075=CARTESIAN_POINT('Ctrl Pts',(-0.107316191403576,-7.79856092090086,
153.200700723659));
#67076=CARTESIAN_POINT('Ctrl Pts',(0.0418228097860945,-7.78664051836476,
153.214672108922));
#67077=CARTESIAN_POINT('Ctrl Pts',(0.190553974279541,-7.77029230854503,
153.228798779438));
#67078=CARTESIAN_POINT('Ctrl Pts',(0.338731670168721,-7.74945715955899,
153.243143329143));
#67079=CARTESIAN_POINT('Ctrl Pts',(0.540870352871086,-7.7210345987635,153.26271164787));
#67080=CARTESIAN_POINT('Ctrl Pts',(0.741986038978563,-7.68426235743513,
153.282684506573));
#67081=CARTESIAN_POINT('Ctrl Pts',(0.941626984869757,-7.63924361945789,
153.302941831059));
#67082=CARTESIAN_POINT('Ctrl Pts',(1.07092990212845,-7.61008600288892,153.316062041145));
#67083=CARTESIAN_POINT('Ctrl Pts',(1.19961276752827,-7.57746829045134,153.329301877301));
#67084=CARTESIAN_POINT('Ctrl Pts',(1.32753676621016,-7.54141321421978,153.342633146228));
#67085=CARTESIAN_POINT('Ctrl Pts',(1.35930484500025,-7.53245945640804,153.34594377446));
#67086=CARTESIAN_POINT('Ctrl Pts',(1.3910260623527,-7.52329370259455,153.349260060887));
#67087=CARTESIAN_POINT('Ctrl Pts',(1.42269816996776,-7.51391628179592,153.35258161386));
#67088=CARTESIAN_POINT('Ctrl Pts',(1.44498487760559,-7.50731767338387,153.354918890587));
#67089=CARTESIAN_POINT('Ctrl Pts',(1.46724583341159,-7.50061464406909,153.357258626739));
#67090=CARTESIAN_POINT('Ctrl Pts',(1.48946890932793,-7.49381093413642,153.359599490312));
#67091=CARTESIAN_POINT('Ctrl Pts',(1.67899517349363,-7.43578648554704,153.379563204141));
#67092=CARTESIAN_POINT('Ctrl Pts',(1.86599674061145,-7.37037383453255,153.399630360127));
#67093=CARTESIAN_POINT('Ctrl Pts',(2.05003895801424,-7.29779065970799,153.419735608681));
#67094=CARTESIAN_POINT('Ctrl Pts',(2.23578121112045,-7.22453701921305,153.440026573539));
#67095=CARTESIAN_POINT('Ctrl Pts',(2.41850899147636,-7.1439790360393,153.460356086658));
#67096=CARTESIAN_POINT('Ctrl Pts',(2.59773797487726,-7.05633057828242,153.480688607584));
#67097=CARTESIAN_POINT('Ctrl Pts',(2.77608539636706,-6.96911323127816,153.500921120264));
#67098=CARTESIAN_POINT('Ctrl Pts',(2.95096799697956,-6.8748745111543,153.521156467461));
#67099=CARTESIAN_POINT('Ctrl Pts',(3.12187594854324,-6.77382454579522,153.54139366803));
#67100=CARTESIAN_POINT('Ctrl Pts',(3.28970994734263,-6.67459206650105,153.56126688203));
#67101=CARTESIAN_POINT('Ctrl Pts',(3.45371058847674,-6.56879099008516,153.581141863008));
#67102=CARTESIAN_POINT('Ctrl Pts',(3.61336928750934,-6.45662439871814,153.60105168054));
#67103=CARTESIAN_POINT('Ctrl Pts',(3.68030089588206,-6.40960227958922,153.609398210469));
#67104=CARTESIAN_POINT('Ctrl Pts',(3.74646915874975,-6.36146152991643,153.617751279783));
#67105=CARTESIAN_POINT('Ctrl Pts',(3.81183546444604,-6.31221736887221,153.626115154147));
#67106=CARTESIAN_POINT('Ctrl Pts',(3.84959742054882,-6.28376913659318,153.630946944061));
#67107=CARTESIAN_POINT('Ctrl Pts',(3.88709173129729,-6.25495266134965,153.635782366191));
#67108=CARTESIAN_POINT('Ctrl Pts',(3.92431278871413,-6.2257709286127,153.640621322474));
#67109=CARTESIAN_POINT('Ctrl Pts',(3.95252988483424,-6.20364840403291,153.644289710855));
#67110=CARTESIAN_POINT('Ctrl Pts',(3.98058993694438,-6.18131596302765,153.647960131348));
#67111=CARTESIAN_POINT('Ctrl Pts',(4.00849044342186,-6.15877490889018,153.651632561352));
#67112=CARTESIAN_POINT('Ctrl Pts',(4.0268583028332,-6.14393536059329,153.654050247858));
#67113=CARTESIAN_POINT('Ctrl Pts',(4.04515052636911,-6.12901062189163,153.65646795302));
#67114=CARTESIAN_POINT('Ctrl Pts',(4.06336326620589,-6.11400400376567,153.658885235115));
#67115=CARTESIAN_POINT('Ctrl Pts',(4.21292912360686,-5.99076731742344,153.67873633233));
#67116=CARTESIAN_POINT('Ctrl Pts',(4.35721037603448,-5.86195109305672,153.698567169177));
#67117=CARTESIAN_POINT('Ctrl Pts',(4.49593593538605,-5.7278629388539,153.71838934154));
#67118=CARTESIAN_POINT('Ctrl Pts',(4.63479042340091,-5.59365016589614,153.73822993622));
#67119=CARTESIAN_POINT('Ctrl Pts',(4.76807887264492,-5.4541553608342,153.758061800089));
#67120=CARTESIAN_POINT('Ctrl Pts',(4.89550039371483,-5.30967073548228,153.777913914657));
#67121=CARTESIAN_POINT('Ctrl Pts',(5.02145670136866,-5.16684753129144,153.797537750798));
#67122=CARTESIAN_POINT('Ctrl Pts',(5.14168023766823,-5.01914842940895,153.817181405182));
#67123=CARTESIAN_POINT('Ctrl Pts',(5.25585219203421,-4.86684331841067,153.836889910767));
#67124=CARTESIAN_POINT('Ctrl Pts',(5.36870538178194,-4.71629743622369,153.856370769554));
#67125=CARTESIAN_POINT('Ctrl Pts',(5.47564609616922,-4.56125128584607,153.875915068782));
#67126=CARTESIAN_POINT('Ctrl Pts',(5.57633788489941,-4.4019549671733,153.895582237819));
#67127=CARTESIAN_POINT('Ctrl Pts',(5.62032802259992,-4.33236173537188,153.904174412862));
#67128=CARTESIAN_POINT('Ctrl Pts',(5.66312508875151,-4.26195716942302,153.912790238856));
#67129=CARTESIAN_POINT('Ctrl Pts',(5.70469916221104,-4.19076149173311,153.921435568427));
#67130=CARTESIAN_POINT('Ctrl Pts',(5.73054731178932,-4.14649648777464,153.926810691751));
#67131=CARTESIAN_POINT('Ctrl Pts',(5.75592268161,-4.10192566619461,153.932197230444));
#67132=CARTESIAN_POINT('Ctrl Pts',(5.78081783980179,-4.05705380882406,153.937596690597));
#67133=CARTESIAN_POINT('Ctrl Pts',(5.79587442276576,-4.02991532518632,153.940862282209));
#67134=CARTESIAN_POINT('Ctrl Pts',(5.81075818838583,-4.00266131967346,153.944133246818));
#67135=CARTESIAN_POINT('Ctrl Pts',(5.82545270270185,-3.97532066537712,153.947406605795));
#67136=CARTESIAN_POINT('Ctrl Pts',(5.90369690306284,-3.82973928808508,153.964836331614));
#67137=CARTESIAN_POINT('Ctrl Pts',(5.97664922546305,-3.6815768948131,153.982348779896));
#67138=CARTESIAN_POINT('Ctrl Pts',(6.04416524408959,-3.53101493938209,154.));
#67139=CARTESIAN_POINT('Ctrl Pts',(4.60531350164922,-6.46554420335129,-0.676259423350488));
#67140=CARTESIAN_POINT('Ctrl Pts',(5.68236987471326,-5.69840091938804,-0.623235491717399));
#67141=CARTESIAN_POINT('Ctrl Pts',(7.42535730630537,-3.61951054181251,-0.517244370183029));
#67142=CARTESIAN_POINT('Ctrl Pts',(8.58296678012314,1.73151873861316,-0.305318868846102));
#67143=CARTESIAN_POINT('Ctrl Pts',(4.71465848402119,8.11444401416975,-0.0404829193397082));
#67144=CARTESIAN_POINT('Ctrl Pts',(-4.27978750802599,8.35543959967712,0.277320220067964));
#67145=CARTESIAN_POINT('Ctrl Pts',(-9.33794990612123,0.932116542185654,
0.595123359475637));
#67146=CARTESIAN_POINT('Ctrl Pts',(-5.83855067917698,-7.35186461183959,
0.912926498883309));
#67147=CARTESIAN_POINT('Ctrl Pts',(1.53223224477109,-8.62179203470423,1.17776244838971));
#67148=CARTESIAN_POINT('Ctrl Pts',(6.06593278951601,-5.59317548027687,1.38963120799482));
#67149=CARTESIAN_POINT('Ctrl Pts',(8.71699111872767,-0.828587516564991,
1.60149996759994));
#67150=CARTESIAN_POINT('Ctrl Pts',(6.8565807090538,6.41311451068115,1.86633591710633));
#67151=CARTESIAN_POINT('Ctrl Pts',(-1.68792736490162,9.23452166984993,2.184139056514));
#67152=CARTESIAN_POINT('Ctrl Pts',(-8.66924682276468,3.58420186719372,2.50194219592167));
#67153=CARTESIAN_POINT('Ctrl Pts',(-7.7163283608382,-5.3465045633832,2.81974533532935));
#67154=CARTESIAN_POINT('Ctrl Pts',(0.326212197437957,-9.38266708925739,
3.13754847473702));
#67155=CARTESIAN_POINT('Ctrl Pts',(6.75680014268004,-5.56896829319403,3.40238442424342));
#67156=CARTESIAN_POINT('Ctrl Pts',(8.24512830401543,-0.323374826084047,
3.61425318384852));
#67157=CARTESIAN_POINT('Ctrl Pts',(7.17220337466533,5.02266100663792,3.82612194345365));
#67158=CARTESIAN_POINT('Ctrl Pts',(1.06007560991606,9.3283081635453,4.09095789296003));
#67159=CARTESIAN_POINT('Ctrl Pts',(-7.27390854203853,5.93440838897662,4.40876103236771));
#67160=CARTESIAN_POINT('Ctrl Pts',(-8.92329103308646,-2.89418249863981,
4.72656417177538));
#67161=CARTESIAN_POINT('Ctrl Pts',(-2.40607174040283,-9.07401688178992,
5.04436731118306));
#67162=CARTESIAN_POINT('Ctrl Pts',(6.33339962621769,-6.93030482747814,5.36217045059073));
#67163=CARTESIAN_POINT('Ctrl Pts',(8.75483483974857,0.143116954380555,5.62700640009711));
#67164=CARTESIAN_POINT('Ctrl Pts',(6.4857259272773,5.10118745343669,5.83887515970225));
#67165=CARTESIAN_POINT('Ctrl Pts',(2.20189237340188,8.47462592794457,6.05074391930734));
#67166=CARTESIAN_POINT('Ctrl Pts',(-5.2429169905794,7.7879971588325,6.31557986881376));
#67167=CARTESIAN_POINT('Ctrl Pts',(-9.38545862533877,-0.200320147439794,
6.63338300822141));
#67168=CARTESIAN_POINT('Ctrl Pts',(-4.91519471530038,-7.99013595043972,
6.95118614762909));
#67169=CARTESIAN_POINT('Ctrl Pts',(4.05345806777821,-8.46737500993547,7.26898928703676));
#67170=CARTESIAN_POINT('Ctrl Pts',(9.3154477429652,-1.16769493639905,7.58679242644443));
#67171=CARTESIAN_POINT('Ctrl Pts',(6.57115862390735,5.78683757551102,7.85162837595083));
#67172=CARTESIAN_POINT('Ctrl Pts',(1.62843632194056,8.08918719373227,8.06349713555594));
#67173=CARTESIAN_POINT('Ctrl Pts',(-3.82014314373728,7.87871316550388,8.27536589516105));
#67174=CARTESIAN_POINT('Ctrl Pts',(-9.04164929613513,2.52777691600338,8.54020184466747));
#67175=CARTESIAN_POINT('Ctrl Pts',(-7.0140760084076,-6.23936692209582,8.85800498407512));
#67176=CARTESIAN_POINT('Ctrl Pts',(1.44062724585838,-9.26962808007599,9.1758081234828));
#67177=CARTESIAN_POINT('Ctrl Pts',(8.57686766441828,-3.81632059811431,9.49361126289047));
#67178=CARTESIAN_POINT('Ctrl Pts',(7.84800405600511,5.15266052317008,9.81141440229815));
#67179=CARTESIAN_POINT('Ctrl Pts',(1.24879103801572,8.66649500826888,10.0762503518046));
#67180=CARTESIAN_POINT('Ctrl Pts',(-4.00667033342535,7.21341438901849,10.2881191114097));
#67181=CARTESIAN_POINT('Ctrl Pts',(-8.01750035760689,3.51956002943052,10.4999878710148));
#67182=CARTESIAN_POINT('Ctrl Pts',(-8.52166878717728,-3.93982730735651,
10.7648238205212));
#67183=CARTESIAN_POINT('Ctrl Pts',(-1.292444002806,-9.29820145726888,11.0826269599288));
#67184=CARTESIAN_POINT('Ctrl Pts',(7.10833853462331,-6.12151410044222,11.4004300993365));
#67185=CARTESIAN_POINT('Ctrl Pts',(9.00356579477459,2.65758627696441,11.7182332387442));
#67186=CARTESIAN_POINT('Ctrl Pts',(2.63198810748128,9.01186533034181,12.0360363781519));
#67187=CARTESIAN_POINT('Ctrl Pts',(-4.67005731023871,7.40663077951727,12.3008723276583));
#67188=CARTESIAN_POINT('Ctrl Pts',(-7.72800462548672,2.89217890471641,12.5127410872634));
#67189=CARTESIAN_POINT('Ctrl Pts',(-8.38532598247424,-2.5206989016241,12.7246098468685));
#67190=CARTESIAN_POINT('Ctrl Pts',(-3.93134236556828,-8.52558650972633,
12.9894457963749));
#67191=CARTESIAN_POINT('Ctrl Pts',(5.04651945463183,-7.91578190922199,13.3072489357826));
#67192=CARTESIAN_POINT('Ctrl Pts',(9.38077626567956,-0.0494798745878378,
13.6250520751902));
#67193=CARTESIAN_POINT('Ctrl Pts',(5.12974155706928,7.86210616807101,13.9428552145979));
#67194=CARTESIAN_POINT('Ctrl Pts',(-3.84118794702279,8.56658352470727,14.2606583540055));
#67195=CARTESIAN_POINT('Ctrl Pts',(-8.35826877743383,2.60901472383387,14.525494303512));
#67196=CARTESIAN_POINT('Ctrl Pts',(-7.75808397367562,-2.81049592880473,
14.7373630631171));
#67197=CARTESIAN_POINT('Ctrl Pts',(-4.74792936837933,-7.35695463475806,
14.9492318227222));
#67198=CARTESIAN_POINT('Ctrl Pts',(2.53677627359465,-9.03912851263144,15.2140677722286));
#67199=CARTESIAN_POINT('Ctrl Pts',(8.97503017698373,-2.75241624079192,15.5318709116363));
#67200=CARTESIAN_POINT('Ctrl Pts',(7.17251833904147,6.0461882439137,15.8496740510439));
#67201=CARTESIAN_POINT('Ctrl Pts',(-1.19428616794719,9.31131797273588,16.1674771904516));
#67202=CARTESIAN_POINT('Ctrl Pts',(-8.4796337332461,4.02950243580197,16.4852803298593));
#67203=CARTESIAN_POINT('Ctrl Pts',(-8.05418178699415,-3.434788279801,16.7501162793657));
#67204=CARTESIAN_POINT('Ctrl Pts',(-4.08254108033916,-7.17074700681693,
16.9619850389708));
#67205=CARTESIAN_POINT('Ctrl Pts',(1.15729944866126,-8.67918618138446,17.1738537985759));
#67206=CARTESIAN_POINT('Ctrl Pts',(7.79321241317349,-5.23516173707155,17.4386897480823));
#67207=CARTESIAN_POINT('Ctrl Pts',(8.61664847138021,3.72563161906873,17.75649288749));
#67208=CARTESIAN_POINT('Ctrl Pts',(1.53833159092038,9.25391525361577,18.0742960268977));
#67209=CARTESIAN_POINT('Ctrl Pts',(-6.9478671948217,6.31301063546267,18.3920991663053));
#67210=CARTESIAN_POINT('Ctrl Pts',(-9.06781150631994,-2.43225669204367,
18.709902305713));
#67211=CARTESIAN_POINT('Ctrl Pts',(-3.90304244852039,-7.83797642443857,
18.9747382552194));
#67212=CARTESIAN_POINT('Ctrl Pts',(1.54301357886363,-8.105915334117,19.1866070148245));
#67213=CARTESIAN_POINT('Ctrl Pts',(6.50974814736132,-5.85583417139971,19.3984757744296));
#67214=CARTESIAN_POINT('Ctrl Pts',(9.32724733240242,1.06936211375347,19.663311723936));
#67215=CARTESIAN_POINT('Ctrl Pts',(4.14255413218105,8.42414429495918,19.9811148633437));
#67216=CARTESIAN_POINT('Ctrl Pts',(-4.83063397340052,8.04154133358492,20.2989180027513));
#67217=CARTESIAN_POINT('Ctrl Pts',(-9.38282324990462,0.299315387832322,
20.6167211421591));
#67218=CARTESIAN_POINT('Ctrl Pts',(-5.32478016722184,-7.73225674049304,
20.9345242815667));
#67219=CARTESIAN_POINT('Ctrl Pts',(2.11237174904617,-8.49738197204518,21.1993602310731));
#67220=CARTESIAN_POINT('Ctrl Pts',(6.4315530863595,-5.16932096176763,21.4112289906782));
#67221=CARTESIAN_POINT('Ctrl Pts',(8.75283793689736,-0.235463023461224,
21.6230977502834));
#67222=CARTESIAN_POINT('Ctrl Pts',(6.40615450560057,6.86310881310455,21.8879336997897));
#67223=CARTESIAN_POINT('Ctrl Pts',(-2.31021700157468,9.09889329786755,22.2057368391974));
#67224=CARTESIAN_POINT('Ctrl Pts',(-8.89226376341935,2.98815273480211,22.5235399786051));
#67225=CARTESIAN_POINT('Ctrl Pts',(-7.33610591228832,-5.85734682975425,
22.8413431180127));
#67226=CARTESIAN_POINT('Ctrl Pts',(0.961614183393465,-9.33897083689823,
23.1591462574204));
#67227=CARTESIAN_POINT('Ctrl Pts',(7.11881881475451,-5.09804212102095,23.4239822069268));
#67228=CARTESIAN_POINT('Ctrl Pts',(8.24808328779048,0.236381865002667,23.6358509665319));
#67229=CARTESIAN_POINT('Ctrl Pts',(6.81516466103088,5.49737623126183,23.8477197261371));
#67230=CARTESIAN_POINT('Ctrl Pts',(0.425183917852744,9.37871509142584,24.1125556756434));
#67231=CARTESIAN_POINT('Ctrl Pts',(-7.65952089614688,5.42758707731466,24.4303588150511));
#67232=CARTESIAN_POINT('Ctrl Pts',(-8.70653421947809,-3.49251678446689,
24.7481619544587));
#67233=CARTESIAN_POINT('Ctrl Pts',(-1.78532270905324,-9.21626739330421,
25.0659650938665));
#67234=CARTESIAN_POINT('Ctrl Pts',(6.78869681247535,-6.48495749549885,25.3837682332741));
#67235=CARTESIAN_POINT('Ctrl Pts',(8.72498645285493,0.736360090244496,25.6486041827805));
#67236=CARTESIAN_POINT('Ctrl Pts',(6.12494475337123,5.52917770347282,25.8604729423856));
#67237=CARTESIAN_POINT('Ctrl Pts',(1.62225132418204,8.60441255555522,26.0723417019908));
#67238=CARTESIAN_POINT('Ctrl Pts',(-5.75887431216354,7.41461022487644,26.3371776514971));
#67239=CARTESIAN_POINT('Ctrl Pts',(-9.35028086563414,-0.836187523286537,
26.6549807909049));
#67240=CARTESIAN_POINT('Ctrl Pts',(-4.36215842218694,-8.30499762218326,
26.9727839303124));
#67241=CARTESIAN_POINT('Ctrl Pts',(4.61821377210678,-8.17306939866945,27.2905870697202));
#67242=CARTESIAN_POINT('Ctrl Pts',(9.37318165779515,-0.533426414898873,
27.6083902091278));
#67243=CARTESIAN_POINT('Ctrl Pts',(6.16369419152492,6.21904242615925,27.8732261586342));
#67244=CARTESIAN_POINT('Ctrl Pts',(1.0762473331214,8.18098074721972,28.0850949182393));
#67245=CARTESIAN_POINT('Ctrl Pts',(-4.34552480206557,7.60158068954343,28.2969636778444));
#67246=CARTESIAN_POINT('Ctrl Pts',(-9.19222594893933,1.90894217664809,28.5617996273508));
#67247=CARTESIAN_POINT('Ctrl Pts',(-6.57491120082365,-6.70056001701554,
28.8796027667585));
#67248=CARTESIAN_POINT('Ctrl Pts',(2.06578740672041,-9.15062478713675,29.1974059061662));
#67249=CARTESIAN_POINT('Ctrl Pts',(8.81587626065388,-3.22603279542901,29.5152090455739));
#67250=CARTESIAN_POINT('Ctrl Pts',(7.48059838386803,5.67289396599397,29.8330121849815));
#67251=CARTESIAN_POINT('Ctrl Pts',(0.658334507932313,8.73122044508511,30.0978481344879));
#67252=CARTESIAN_POINT('Ctrl Pts',(-4.4865159400542,6.92516635381925,30.309716894093));
#67253=CARTESIAN_POINT('Ctrl Pts',(-8.2376758883841,2.96787983970747,30.5215856536982));
#67254=CARTESIAN_POINT('Ctrl Pts',(-8.23494234109841,-4.508525564852,30.7864216032046));
#67255=CARTESIAN_POINT('Ctrl Pts',(-0.659057717521624,-9.36443296549871,
31.1042247426122));
#67256=CARTESIAN_POINT('Ctrl Pts',(7.50701695534774,-5.62548735994027,31.4220278820199));
#67257=CARTESIAN_POINT('Ctrl Pts',(8.80266564433859,3.26190732460705,31.7398310214275));
#67258=CARTESIAN_POINT('Ctrl Pts',(2.01493291010401,9.1695759715441,32.0576341608353));
#67259=CARTESIAN_POINT('Ctrl Pts',(-5.16147639882758,7.07296091954089,32.3224701103416));
#67260=CARTESIAN_POINT('Ctrl Pts',(-7.90631023908158,2.3615699675903,32.5343388699467));
#67261=CARTESIAN_POINT('Ctrl Pts',(-8.19512929753748,-3.08341865169973,
32.7462076295519));
#67262=CARTESIAN_POINT('Ctrl Pts',(-3.34426672559207,-8.77251151029379,
33.0110435790582));
#67263=CARTESIAN_POINT('Ctrl Pts',(5.57159242753132,-7.55541657764941,33.3288467184659));
#67264=CARTESIAN_POINT('Ctrl Pts',(9.36254556394446,0.586644839566965,33.6466498578736));
#67265=CARTESIAN_POINT('Ctrl Pts',(4.58489192880254,8.19180858184234,33.9644529972813));
#67266=CARTESIAN_POINT('Ctrl Pts',(-4.41315836778878,8.28644141661275,34.2822561366889));
#67267=CARTESIAN_POINT('Ctrl Pts',(-8.51592577979034,2.03632583299158,34.5470920861953));
#67268=CARTESIAN_POINT('Ctrl Pts',(-7.54968252853129,-3.33002222617508,
34.7589608458004));
#67269=CARTESIAN_POINT('Ctrl Pts',(-4.2382072629376,-7.66193278366428,34.9708296054056));
#67270=CARTESIAN_POINT('Ctrl Pts',(3.14378643854585,-8.84633737537489,35.235665554912));
#67271=CARTESIAN_POINT('Ctrl Pts',(9.14099053016895,-2.13758133592746,35.5534686943197));
#67272=CARTESIAN_POINT('Ctrl Pts',(6.74608634709743,6.51856814049157,35.8712718337273));
#67273=CARTESIAN_POINT('Ctrl Pts',(-1.82283971500673,9.20892052380395,36.189074973135));
#67274=CARTESIAN_POINT('Ctrl Pts',(-8.73331966470392,3.44531649696147,36.5068781125426));
#67275=CARTESIAN_POINT('Ctrl Pts',(-7.80277237585837,-3.97295331404088,
36.7717140620491));
#67276=CARTESIAN_POINT('Ctrl Pts',(-3.58697481303287,-7.43104070767335,
36.9835828216541));
#67277=CARTESIAN_POINT('Ctrl Pts',(1.74307995654875,-8.58075096073092,37.1954515812593));
#67278=CARTESIAN_POINT('Ctrl Pts',(8.13022077659065,-4.69474048846503,37.4602875307657));
#67279=CARTESIAN_POINT('Ctrl Pts',(8.34422581050367,4.30126231049319,37.7780906701733));
#67280=CARTESIAN_POINT('Ctrl Pts',(0.90738208935135,9.33691969273868,38.0958938095811));
#67281=CARTESIAN_POINT('Ctrl Pts',(-7.35989821147914,5.82742311463735,38.4136969489886));
#67282=CARTESIAN_POINT('Ctrl Pts',(-8.88204073208721,-3.0414520485589,38.7315000883964));
#67283=CARTESIAN_POINT('Ctrl Pts',(-3.36265146813914,-8.08456491648306,
38.9963360379027));
#67284=CARTESIAN_POINT('Ctrl Pts',(2.08903913788005,-7.98264804365293,39.2082047975079));
#67285=CARTESIAN_POINT('Ctrl Pts',(6.89179100417881,-5.40100282722816,39.420073557113));
#67286=CARTESIAN_POINT('Ctrl Pts',(9.23328300362556,1.69928311505142,39.6849095066194));
#67287=CARTESIAN_POINT('Ctrl Pts',(3.56187020826584,8.68562274450209,40.002712646027));
#67288=CARTESIAN_POINT('Ctrl Pts',(-5.36473011593325,7.69552352916454,40.3205157854348));
#67289=CARTESIAN_POINT('Ctrl Pts',(-9.38152653210372,-0.337522988517498,
40.6383189248424));
#67290=CARTESIAN_POINT('Ctrl Pts',(-4.78828546141623,-8.07548143890686,
40.9561220642501));
#67291=CARTESIAN_POINT('Ctrl Pts',(2.68362839752818,-8.33461177314138,41.2209580137564));
#67292=CARTESIAN_POINT('Ctrl Pts',(6.76723069875256,-4.72137087912944,41.4328267733616));
#67293=CARTESIAN_POINT('Ctrl Pts',(8.74866168043804,0.358515810309832,41.6446955329666));
#67294=CARTESIAN_POINT('Ctrl Pts',(5.92609922447768,7.28164995806476,41.9095314824732));
#67295=CARTESIAN_POINT('Ctrl Pts',(-2.92180050089287,8.92132521956945,42.2273346218806));
#67296=CARTESIAN_POINT('Ctrl Pts',(-9.07439735351213,2.37838690614001,42.5451377612886));
#67297=CARTESIAN_POINT('Ctrl Pts',(-6.92210083284602,-6.34125239209545,
42.862940900696));
#67298=CARTESIAN_POINT('Ctrl Pts',(1.59257796183507,-9.25228477542799,43.1807440401039));
#67299=CARTESIAN_POINT('Ctrl Pts',(7.4480823495277,-4.60365985924904,43.4455799896102));
#67300=CARTESIAN_POINT('Ctrl Pts',(8.21307769156944,0.795052916902295,43.6574487492153));
#67301=CARTESIAN_POINT('Ctrl Pts',(6.42676406589048,5.94679059883447,43.8693175088204));
#67302=CARTESIAN_POINT('Ctrl Pts',(-0.211665554595585,9.38596163550319,
44.1341534583268));
#67303=CARTESIAN_POINT('Ctrl Pts',(-8.00988320686094,4.89578725567103,44.4519565977345));
#67304=CARTESIAN_POINT('Ctrl Pts',(-8.44970977156173,-4.07477807752771,
44.7697597371422));
#67305=CARTESIAN_POINT('Ctrl Pts',(-1.15635737635423,-9.31610430697805,
45.0875628765497));
#67306=CARTESIAN_POINT('Ctrl Pts',(7.21275197559268,-6.00976597453871,45.4053660159576));
#67307=CARTESIAN_POINT('Ctrl Pts',(8.65498527413781,1.3262144206215,45.6702019654639));
#67308=CARTESIAN_POINT('Ctrl Pts',(5.73597625169008,5.93172240993103,45.882070725069));
#67309=CARTESIAN_POINT('Ctrl Pts',(1.03514460450429,8.69460122333234,46.0939394846741));
#67310=CARTESIAN_POINT('Ctrl Pts',(-6.24832900639056,7.00710088110893,46.3587754341805));
#67311=CARTESIAN_POINT('Ctrl Pts',(-9.27207262988954,-1.46820672468048,
46.6765785735882));
#67312=CARTESIAN_POINT('Ctrl Pts',(-3.7890472542822,-8.5816392670365,46.9943817129958));
#67313=CARTESIAN_POINT('Ctrl Pts',(5.16171622086671,-7.84115090376312,47.3121848524036));
#67314=CARTESIAN_POINT('Ctrl Pts',(9.38777970915338,0.103296962915415,47.6299879918112));
#67315=CARTESIAN_POINT('Ctrl Pts',(5.72786412260422,6.62262692426425,47.8948239413177));
#67316=CARTESIAN_POINT('Ctrl Pts',(0.51910539873841,8.23512500775983,48.1066927009227));
#67317=CARTESIAN_POINT('Ctrl Pts',(-4.85090813224476,7.28946534922341,48.3185614605278));
#67318=CARTESIAN_POINT('Ctrl Pts',(-9.30049950644462,1.28132238752107,48.5833974100343));
#67319=CARTESIAN_POINT('Ctrl Pts',(-6.10548831459029,-7.13091679104062,
48.9012005494418));
#67320=CARTESIAN_POINT('Ctrl Pts',(2.68144070795267,-8.98950984951128,49.2190036888497));
#67321=CARTESIAN_POINT('Ctrl Pts',(9.0143137421148,-2.62089862433939,49.5368068282571));
#67322=CARTESIAN_POINT('Ctrl Pts',(7.0787666142288,6.167020459786,49.8546099676651));
#67323=CARTESIAN_POINT('Ctrl Pts',(0.0648482886750494,8.75576435752259,
50.1194459171712));
#67324=CARTESIAN_POINT('Ctrl Pts',(-4.9457143701813,6.60504834781795,50.3313146767765));
#67325=CARTESIAN_POINT('Ctrl Pts',(-8.41994121215125,2.40254131471727,50.5431834363815));
#67326=CARTESIAN_POINT('Ctrl Pts',(-7.91031826793559,-5.0564753564221,50.808019385888));
#67327=CARTESIAN_POINT('Ctrl Pts',(-0.022638414813296,-9.38756887285086,
51.1258225252955));
#67328=CARTESIAN_POINT('Ctrl Pts',(7.87114769895336,-5.10357183803536,51.4436256647034));
#67329=CARTESIAN_POINT('Ctrl Pts',(8.56125517505403,3.8512169074144,51.7614288041108));
#67330=CARTESIAN_POINT('Ctrl Pts',(1.38860488811382,9.28508775375044,52.0792319435187));
#67331=CARTESIAN_POINT('Ctrl Pts',(-5.62914210825904,6.70674093058861,52.344067893025));
#67332=CARTESIAN_POINT('Ctrl Pts',(-8.04823060738345,1.82009296433092,52.5559366526302));
#67333=CARTESIAN_POINT('Ctrl Pts',(-7.9672182071849,-3.63194835096917,52.7678054122352));
#67334=CARTESIAN_POINT('Ctrl Pts',(-2.74180059859255,-8.97906496288433,
53.0326413617416));
#67335=CARTESIAN_POINT('Ctrl Pts',(6.07102464627148,-7.16028083141352,53.3504445011493));
#67336=CARTESIAN_POINT('Ctrl Pts',(9.30122794725025,1.2200697840768,53.668247640557));
#67337=CARTESIAN_POINT('Ctrl Pts',(4.01894239268663,8.48381187230187,53.9860507799647));
#67338=CARTESIAN_POINT('Ctrl Pts',(-4.96481920736273,7.96816468004654,54.3038539193723));
#67339=CARTESIAN_POINT('Ctrl Pts',(-8.63439205486384,1.45426566620785,54.5686898688788));
#67340=CARTESIAN_POINT('Ctrl Pts',(-7.30653705711197,-3.83422359043915,
54.7805586284838));
#67341=CARTESIAN_POINT('Ctrl Pts',(-3.70898071026316,-7.93165032486322,
54.992427388089));
#67342=CARTESIAN_POINT('Ctrl Pts',(3.73632873703891,-8.61283493972319,55.2572633375954));
#67343=CARTESIAN_POINT('Ctrl Pts',(9.2648835760257,-1.5129091721029,55.575066477003));
#67344=CARTESIAN_POINT('Ctrl Pts',(6.28860851972772,6.96094925210161,55.8928696164107));
#67345=CARTESIAN_POINT('Ctrl Pts',(-2.44300446019104,9.0641431502283,56.2106727558183));
#67346=CARTESIAN_POINT('Ctrl Pts',(-8.9468144110687,2.84527503486617,56.5284758952261));
#67347=CARTESIAN_POINT('Ctrl Pts',(-7.51545420598724,-4.49283461332772,
56.7933118447323));
#67348=CARTESIAN_POINT('Ctrl Pts',(-3.07490110363451,-7.65713637800046,
57.0051806043376));
#67349=CARTESIAN_POINT('Ctrl Pts',(2.32083872106099,-8.44282668398626,57.2170493639426));
#67350=CARTESIAN_POINT('Ctrl Pts',(8.42981344693531,-4.13271380330264,57.4818853134491));
#67351=CARTESIAN_POINT('Ctrl Pts',(8.03340259441033,4.85709837212146,57.7996884528567));
#67352=CARTESIAN_POINT('Ctrl Pts',(0.272256768860956,9.37695514847626,58.1174915922644));
#67353=CARTESIAN_POINT('Ctrl Pts',(-7.73805859902398,5.31501749370731,58.435294731672));
#67354=CARTESIAN_POINT('Ctrl Pts',(-8.65539435078031,-3.63665048672807,
58.7530978710798));
#67355=CARTESIAN_POINT('Ctrl Pts',(-2.80678539320662,-8.29394782606501,
59.0179338205861));
#67356=CARTESIAN_POINT('Ctrl Pts',(2.62545083162156,-7.82264419740334,59.2298025801913));
#67357=CARTESIAN_POINT('Ctrl Pts',(7.24211748526434,-4.92131579098878,59.4416713397963));
#67358=CARTESIAN_POINT('Ctrl Pts',(9.09682663282309,2.32138392828507,59.7065072893028));
#67359=CARTESIAN_POINT('Ctrl Pts',(2.96479437493774,8.90712951262538,60.0243104287104));
#67360=CARTESIAN_POINT('Ctrl Pts',(-5.87413749527606,7.31409053070298,60.3421135681181));
#67361=CARTESIAN_POINT('Ctrl Pts',(-9.33705554795461,-0.97280806676027,
60.6599167075258));
#67362=CARTESIAN_POINT('Ctrl Pts',(-4.2297548202907,-8.38154235748808,60.9777198469334));
#67363=CARTESIAN_POINT('Ctrl Pts',(3.2425348504619,-8.13348526331403,61.2425557964399));
#67364=CARTESIAN_POINT('Ctrl Pts',(7.07176516832905,-4.25169280551155,61.4544245560449));
#67365=CARTESIAN_POINT('Ctrl Pts',(8.70422363414217,0.95084473593113,61.6662933156501));
#67366=CARTESIAN_POINT('Ctrl Pts',(5.41877173073039,7.66668057638876,61.9311292651565));
#67367=CARTESIAN_POINT('Ctrl Pts',(-3.5199377244256,8.70270074497046,62.2489324045641));
#67368=CARTESIAN_POINT('Ctrl Pts',(-9.21477010149155,1.75767561893064,62.5667355439718));
#67369=CARTESIAN_POINT('Ctrl Pts',(-6.47623989028538,-6.79597518563895,
62.8845386833795));
#67370=CARTESIAN_POINT('Ctrl Pts',(2.21621261480156,-9.12301922480348,63.2023418227871));
#67371=CARTESIAN_POINT('Ctrl Pts',(7.74306942726154,-4.08809131864914,63.4671777722936));
#67372=CARTESIAN_POINT('Ctrl Pts',(8.14027509050269,1.35006509449442,63.6790465318986));
#67373=CARTESIAN_POINT('Ctrl Pts',(6.00878717284279,6.36883753101665,63.8909152915039));
#67374=CARTESIAN_POINT('Ctrl Pts',(-0.847540931303655,9.35001350265893,
64.1557512410101));
#67375=CARTESIAN_POINT('Ctrl Pts',(-8.32338362417113,4.34145676993609,64.4735543804179));
#67376=CARTESIAN_POINT('Ctrl Pts',(-8.15399932582899,-4.63828703285015,
64.7913575198255));
#67377=CARTESIAN_POINT('Ctrl Pts',(-0.522070427691442,-9.37306803073971,
65.1091606592332));
#67378=CARTESIAN_POINT('Ctrl Pts',(7.60361368412317,-5.5069172022788,65.4269637986408));
#67379=CARTESIAN_POINT('Ctrl Pts',(8.54515340921122,1.90996544420299,65.6917997481474));
#67380=CARTESIAN_POINT('Ctrl Pts',(5.32061049305866,6.30696902557715,65.9036685077523));
#67381=CARTESIAN_POINT('Ctrl Pts',(0.443274096256249,8.74477689026912,66.1155372673576));
#67382=CARTESIAN_POINT('Ctrl Pts',(-6.70902857000643,6.56734449964217,66.3803732168638));
#67383=CARTESIAN_POINT('Ctrl Pts',(-9.15119384027104,-2.09346916341428,
66.6981763562716));
#67384=CARTESIAN_POINT('Ctrl Pts',(-3.19849869654243,-8.81878776776366,
67.0159794956792));
#67385=CARTESIAN_POINT('Ctrl Pts',(5.68146418679031,-7.47314703017458,67.333782635087));
#67386=CARTESIAN_POINT('Ctrl Pts',(9.35917471673265,0.739544962821455,67.6515857744945));
#67387=CARTESIAN_POINT('Ctrl Pts',(5.26567412914822,6.99573375351603,67.916421724001));
#67388=CARTESIAN_POINT('Ctrl Pts',(-0.0404254852931306,8.25137080060695,
68.1282904836061));
#67389=CARTESIAN_POINT('Ctrl Pts',(-5.33396733442199,6.94380351535604,68.3401592432112));
#67390=CARTESIAN_POINT('Ctrl Pts',(-9.36597168800007,0.647805887207846,
68.6049951927176));
#67391=CARTESIAN_POINT('Ctrl Pts',(-5.60796765815626,-7.52845672048098,
68.9227983321252));
#67392=CARTESIAN_POINT('Ctrl Pts',(3.28475388189587,-8.78702472589971,69.240601471533));
#67393=CARTESIAN_POINT('Ctrl Pts',(9.1712668885677,-2.00370294432065,69.5584046109406));
#67394=CARTESIAN_POINT('Ctrl Pts',(6.64435799900976,6.63276601102574,69.8762077503483));
#67395=CARTESIAN_POINT('Ctrl Pts',(-0.528936368355967,8.74001378982291,
70.1410436998546));
#67396=CARTESIAN_POINT('Ctrl Pts',(-5.38215236557387,6.25453357505922,70.3529124594599));
#67397=CARTESIAN_POINT('Ctrl Pts',(-8.56345754306331,1.82614616024865,70.5647812190648));
#67398=CARTESIAN_POINT('Ctrl Pts',(-7.54929048622397,-5.58115496543806,
70.8296171685713));
#67399=CARTESIAN_POINT('Ctrl Pts',(0.613885040667023,-9.36750274626135,
71.147420307979));
#67400=CARTESIAN_POINT('Ctrl Pts',(8.19905507261868,-4.55816934438155,71.4652234473866));
#67401=CARTESIAN_POINT('Ctrl Pts',(8.28044526515006,4.42280285549989,71.7830265867943));
#67402=CARTESIAN_POINT('Ctrl Pts',(0.755886643805071,9.35786935756555,72.100829726202));
#67403=CARTESIAN_POINT('Ctrl Pts',(-6.0709025814317,6.30965570102665,72.3656656757083));
#67404=CARTESIAN_POINT('Ctrl Pts',(-8.15311211898698,1.27024043376002,72.5775344353135));
#67405=CARTESIAN_POINT('Ctrl Pts',(-7.70264275461673,-4.16376518087617,
72.7894031949187));
#67406=CARTESIAN_POINT('Ctrl Pts',(-2.12671404881879,-9.14429302064248,
73.054239144425));
#67407=CARTESIAN_POINT('Ctrl Pts',(6.54251347660453,-6.73219860486695,73.3720422838326));
#67408=CARTESIAN_POINT('Ctrl Pts',(9.19711332143845,1.84788996034588,73.6898454232404));
#67409=CARTESIAN_POINT('Ctrl Pts',(3.43448286563956,8.73675319058521,74.007648562648));
#67410=CARTESIAN_POINT('Ctrl Pts',(-5.49360270115903,7.61325580989032,74.3254517020558));
#67411=CARTESIAN_POINT('Ctrl Pts',(-8.71317307193497,0.865446903682397,
74.590287651562));
#67412=CARTESIAN_POINT('Ctrl Pts',(-7.02969889960619,-4.32069156311902,
74.8021564111673));
#67413=CARTESIAN_POINT('Ctrl Pts',(-3.16284988407271,-8.16508048661717,
75.0140251707722));
#67414=CARTESIAN_POINT('Ctrl Pts',(4.31202586543046,-8.33924037179835,75.2788611202788));
#67415=CARTESIAN_POINT('Ctrl Pts',(9.34555270036502,-0.882038459310571,
75.5966642596863));
#67416=CARTESIAN_POINT('Ctrl Pts',(5.80326091633985,7.37269032199734,75.9144673990941));
#67417=CARTESIAN_POINT('Ctrl Pts',(-3.05394033905752,8.87503027579986,76.2322705385017));
#67418=CARTESIAN_POINT('Ctrl Pts',(-9.1152435335431,2.23719675377212,76.5500736779094));
#67419=CARTESIAN_POINT('Ctrl Pts',(-6.81651864177013,-6.44743929429287,
76.8678768173171));
#67420=CARTESIAN_POINT('Ctrl Pts',(1.72522542783871,-9.22718507141483,77.1856799567247));
#67421=CARTESIAN_POINT('Ctrl Pts',(8.69565483555478,-3.53865568029239,77.5034830961325));
#67422=CARTESIAN_POINT('Ctrl Pts',(7.8449010032873,3.88968983220228,77.7683190456387));
#67423=CARTESIAN_POINT('Ctrl Pts',(3.66594536676364,7.39228562561244,77.9801878052441));
#67424=CARTESIAN_POINT('Ctrl Pts',(-1.65140120025543,8.59891024493111,78.1920565648489));
#67425=CARTESIAN_POINT('Ctrl Pts',(-8.07972130758836,4.78115448994417,78.4568925143554));
#67426=CARTESIAN_POINT('Ctrl Pts',(-8.3896089253915,-4.21200557295021,78.7746956537631));
#67427=CARTESIAN_POINT('Ctrl Pts',(-1.00692323689734,-9.32671948478797,
79.0924987931708));
#67428=CARTESIAN_POINT('Ctrl Pts',(7.29733197467081,-5.90558436552824,79.4103019325784));
#67429=CARTESIAN_POINT('Ctrl Pts',(8.91397127598894,2.94654434612107,79.7281050719862));
#67430=CARTESIAN_POINT('Ctrl Pts',(3.44868801762181,8.04824184799615,79.9929410214924));
#67431=CARTESIAN_POINT('Ctrl Pts',(-2.0037815204154,8.00447422400582,80.2048097810977));
#67432=CARTESIAN_POINT('Ctrl Pts',(-6.83379386824274,5.47420081702346,80.4166785407027));
#67433=CARTESIAN_POINT('Ctrl Pts',(-9.25088187844766,-1.6007085938909,80.6815144902092));
#67434=CARTESIAN_POINT('Ctrl Pts',(-3.65430448618155,-8.64713927319536,
80.9993176296168));
#67435=CARTESIAN_POINT('Ctrl Pts',(5.28234787004528,-7.75230371152486,81.3171207690245));
#67436=CARTESIAN_POINT('Ctrl Pts',(9.38459283052847,0.237444624201594,81.6349239084322));
#67437=CARTESIAN_POINT('Ctrl Pts',(4.87414259099121,8.02395236752506,81.9527270478397));
#67438=CARTESIAN_POINT('Ctrl Pts',(-2.59458247415171,8.36276011106766,82.2175629973463));
#67439=CARTESIAN_POINT('Ctrl Pts',(-6.71648974456451,4.79327861061246,82.4294317569514));
#67440=CARTESIAN_POINT('Ctrl Pts',(-8.75198783567674,-0.265186070959599,
82.6413005165564));
#67441=CARTESIAN_POINT('Ctrl Pts',(-6.00342500595349,-7.21803064373623,
82.9061364660629));
#67442=CARTESIAN_POINT('Ctrl Pts',(2.82648341645369,-8.95198041368108,83.2239396054705));
#67443=CARTESIAN_POINT('Ctrl Pts',(9.04851439375484,-2.47503512383449,83.5417427448782));
#67444=CARTESIAN_POINT('Ctrl Pts',(6.98934009826024,6.2670636535728,83.8595458842859));
#67445=CARTESIAN_POINT('Ctrl Pts',(-1.49380661323534,9.26874424774865,84.1773490236935));
#67446=CARTESIAN_POINT('Ctrl Pts',(-7.39855811862921,4.68283595162349,84.4421849732));
#67447=CARTESIAN_POINT('Ctrl Pts',(-8.22109022443365,-0.707410652091151,
84.654053732805));
#67448=CARTESIAN_POINT('Ctrl Pts',(-6.48982435061033,-5.87790733872935,
84.8659224924102));
#67449=CARTESIAN_POINT('Ctrl Pts',(0.111547012188838,-9.38768530546449,
85.1307584419166));
#67450=CARTESIAN_POINT('Ctrl Pts',(7.95721132033966,-4.98093865088163,85.4485615813242));
#67451=CARTESIAN_POINT('Ctrl Pts',(8.49268893873445,3.98442545350508,85.7663647207319));
#67452=CARTESIAN_POINT('Ctrl Pts',(1.2556530401561,9.30324122460166,86.0841678601397));
#67453=CARTESIAN_POINT('Ctrl Pts',(-7.14824422597728,6.08635216003193,86.4019709995472));
#67454=CARTESIAN_POINT('Ctrl Pts',(-8.6686378048306,-1.23382875378166,86.6668069490537));
#67455=CARTESIAN_POINT('Ctrl Pts',(-5.79891511690275,-5.8702076432944,86.8786757086588));
#67456=CARTESIAN_POINT('Ctrl Pts',(-1.12781848653672,-8.68306629287317,
87.0905444682638));
#67457=CARTESIAN_POINT('Ctrl Pts',(6.17323898017392,-7.07334423195992,87.3553804177703));
#67458=CARTESIAN_POINT('Ctrl Pts',(9.28720448840491,1.36923140151558,87.6731835571779));
#67459=CARTESIAN_POINT('Ctrl Pts',(3.88035969589542,8.54073885768649,87.9909866965857));
#67460=CARTESIAN_POINT('Ctrl Pts',(-5.0777923921815,7.8957574850199,88.3087898359931));
#67461=CARTESIAN_POINT('Ctrl Pts',(-9.38834746436722,-0.00316519361544216,
88.6265929754011));
#67462=CARTESIAN_POINT('Ctrl Pts',(-5.79817233028434,-6.56115938027206,
88.8914289249072));
#67463=CARTESIAN_POINT('Ctrl Pts',(-0.606908062902263,-8.229120056945,89.1032976845126));
#67464=CARTESIAN_POINT('Ctrl Pts',(4.77288601530261,-7.34078836842037,89.3151664441175));
#67465=CARTESIAN_POINT('Ctrl Pts',(9.28630449027279,-1.38044450959777,89.580002393624));
#67466=CARTESIAN_POINT('Ctrl Pts',(6.18119623774963,7.06539276408422,89.8978055330316));
#67467=CARTESIAN_POINT('Ctrl Pts',(-2.58541006692869,9.01759759528832,90.2156086724394));
#67468=CARTESIAN_POINT('Ctrl Pts',(-8.98584767790854,2.71689222270035,90.5334118118469));
#67469=CARTESIAN_POINT('Ctrl Pts',(-7.14413868793919,-6.09117070337302,
90.8512149512548));
#67470=CARTESIAN_POINT('Ctrl Pts',(-0.158229698722761,-8.75457469826193,
91.1160509007609));
#67471=CARTESIAN_POINT('Ctrl Pts',(4.87498654891268,-6.65742145701708,91.3279196603662));
#67472=CARTESIAN_POINT('Ctrl Pts',(8.39383785726041,-2.49220801921283,91.5397884199713));
#67473=CARTESIAN_POINT('Ctrl Pts',(7.96379846267019,4.97181980527365,91.8046243694778));
#67474=CARTESIAN_POINT('Ctrl Pts',(0.12276077239064,9.3867934691835,92.1224275088853));
#67475=CARTESIAN_POINT('Ctrl Pts',(-7.81626756533493,5.18723172335875,92.4402306482931));
#67476=CARTESIAN_POINT('Ctrl Pts',(-8.60184359340913,-3.7596873054644,92.7580337877005));
#67477=CARTESIAN_POINT('Ctrl Pts',(-1.48755653318772,-9.26974938661827,
93.0758369271086));
#67478=CARTESIAN_POINT('Ctrl Pts',(5.55729080655709,-6.76639739273147,93.3406728766146));
#67479=CARTESIAN_POINT('Ctrl Pts',(8.02836053062309,-1.9058282972932,93.55254163622));
#67480=CARTESIAN_POINT('Ctrl Pts',(8.00550179241508,3.54676695550274,93.7644103958249));
#67481=CARTESIAN_POINT('Ctrl Pts',(2.83741137236831,8.94931141675683,94.0292463453314));
#67482=CARTESIAN_POINT('Ctrl Pts',(-5.99431095549163,7.22462441994161,94.347049484739));
#67483=CARTESIAN_POINT('Ctrl Pts',(-9.31371162891651,-1.120797616928,94.6648526241468));
#67484=CARTESIAN_POINT('Ctrl Pts',(-4.10919837457598,-8.44046506767997,
94.9826557635543));
#67485=CARTESIAN_POINT('Ctrl Pts',(4.87955190532278,-8.02066402072798,95.3004589029622));
#67486=CARTESIAN_POINT('Ctrl Pts',(8.61839038970218,-1.5462735449124,95.5652948524683));
#67487=CARTESIAN_POINT('Ctrl Pts',(7.3470155989771,3.7560772218923,95.7771636120737));
#67488=CARTESIAN_POINT('Ctrl Pts',(3.79336521223575,7.89164084025658,95.9890323716785));
#67489=CARTESIAN_POINT('Ctrl Pts',(-3.64425554288549,8.65219507803006,96.2538683211854));
#67490=CARTESIAN_POINT('Ctrl Pts',(-9.2482205837292,1.6116382581185,96.5716714605926));
#67491=CARTESIAN_POINT('Ctrl Pts',(-6.36249322888283,-6.89348181379674,
96.8894746000007));
#67492=CARTESIAN_POINT('Ctrl Pts',(2.34619137542456,-9.08968359571602,97.2072777394079));
#67493=CARTESIAN_POINT('Ctrl Pts',(8.91595908687415,-2.94053595307482,97.525080878816));
#67494=CARTESIAN_POINT('Ctrl Pts',(7.56294531793053,4.41242256623269,97.789916828322));
#67495=CARTESIAN_POINT('Ctrl Pts',(3.15639382722669,7.62390531918362,98.0017855879274));
#67496=CARTESIAN_POINT('Ctrl Pts',(-2.23065927072821,8.4670995035443,98.2136543475322));
#67497=CARTESIAN_POINT('Ctrl Pts',(-8.38525627827585,4.22238739077491,98.4784902970391));
#67498=CARTESIAN_POINT('Ctrl Pts',(-8.08474932180308,-4.77114139844422,
98.7962934364465));
#67499=CARTESIAN_POINT('Ctrl Pts',(-0.37225172720383,-9.37351802987116,
99.1140965758541));
#67500=CARTESIAN_POINT('Ctrl Pts',(7.68093084977082,-5.39724588298354,99.4318997152619));
#67501=CARTESIAN_POINT('Ctrl Pts',(8.69368894436464,3.54412904234188,99.7497028546694));
#67502=CARTESIAN_POINT('Ctrl Pts',(2.89508531527422,8.26354014949349,100.014538804176));
#67503=CARTESIAN_POINT('Ctrl Pts',(-2.54186864664432,7.8502011497564,100.226407563781));
#67504=CARTESIAN_POINT('Ctrl Pts',(-7.18921699219222,4.99827708557477,100.438276323386));
#67505=CARTESIAN_POINT('Ctrl Pts',(-9.12106806867608,-2.22422917360528,
100.703112272893));
#67506=CARTESIAN_POINT('Ctrl Pts',(-3.05962523352364,-8.87500170539302,
101.0209154123));
#67507=CARTESIAN_POINT('Ctrl Pts',(5.79579453715258,-7.37632545972848,101.338718551708));
#67508=CARTESIAN_POINT('Ctrl Pts',(9.34690000800457,0.873167842231912,101.656521691115));
#67509=CARTESIAN_POINT('Ctrl Pts',(4.31890805017312,8.3359529379843,101.974324830524));
#67510=CARTESIAN_POINT('Ctrl Pts',(-3.15560227365146,8.16760607984566,102.23916078003));
#67511=CARTESIAN_POINT('Ctrl Pts',(-7.02601626638363,4.32687528511553,102.451029539635));
#67512=CARTESIAN_POINT('Ctrl Pts',(-8.71386983768246,-0.857955265112621,
102.66289829924));
#67513=CARTESIAN_POINT('Ctrl Pts',(-5.50023293227864,-7.60845029035593,
102.927734248746));
#67514=CARTESIAN_POINT('Ctrl Pts',(3.42691836949006,-8.7397478412821,103.245537388154));
#67515=CARTESIAN_POINT('Ctrl Pts',(9.19549938924046,-1.85585629486889,103.563340527562));
#67516=CARTESIAN_POINT('Ctrl Pts',(6.54835438700928,6.72651593787452,103.881143666969));
#67517=CARTESIAN_POINT('Ctrl Pts',(-2.11878448355848,9.14613746028187,104.198946806377));
#67518=CARTESIAN_POINT('Ctrl Pts',(-7.69902724331096,4.17044293711862,104.463782755883));
#67519=CARTESIAN_POINT('Ctrl Pts',(-8.15421127793089,-1.26316774155096,
104.675651515489));
#67520=CARTESIAN_POINT('Ctrl Pts',(-6.07637259690935,-6.3043882215911,104.887520275093));
#67521=CARTESIAN_POINT('Ctrl Pts',(0.7477696280061,-9.35852118198021,105.1523562246));
#67522=CARTESIAN_POINT('Ctrl Pts',(8.27660614921521,-4.4299833511106,105.470159364008));
#67523=CARTESIAN_POINT('Ctrl Pts',(8.20300544916199,4.55105627362975,105.787962503416));
#67524=CARTESIAN_POINT('Ctrl Pts',(0.622009718693708,9.36696673156227,106.105765642823));
#67525=CARTESIAN_POINT('Ctrl Pts',(-7.5444468647533,5.58770074673416,106.423568782231));
#67526=CARTESIAN_POINT('Ctrl Pts',(-8.56503821645671,-1.81871799233499,
106.688404731737));
#67527=CARTESIAN_POINT('Ctrl Pts',(-5.3875751976612,-6.24986302233706,106.900273491342));
#67528=CARTESIAN_POINT('Ctrl Pts',(-0.53651679449818,-8.73955173416969,
107.112142250947));
#67529=CARTESIAN_POINT('Ctrl Pts',(6.6386025863016,-6.63852648042387,107.376978200454));
#67530=CARTESIAN_POINT('Ctrl Pts',(9.17300134601047,1.99574751570282,107.694781339861));
#67531=CARTESIAN_POINT('Ctrl Pts',(3.2923740484798,8.78417239867384,108.012584479269));
#67532=CARTESIAN_POINT('Ctrl Pts',(-5.60143576160796,7.53331794423434,108.330387618677));
#67533=CARTESIAN_POINT('Ctrl Pts',(-9.36653003787306,-0.639682092731105,
108.648190758084));
#67534=CARTESIAN_POINT('Ctrl Pts',(-5.33998801752543,-6.93917450117029,
108.913026707591));
#67535=CARTESIAN_POINT('Ctrl Pts',(-0.0475822746342192,-8.25133263391868,
109.124895467196));
#67536=CARTESIAN_POINT('Ctrl Pts',(5.25960441743795,-7.00029829057828,109.336764226801));
#67537=CARTESIAN_POINT('Ctrl Pts',(9.35852975395092,-0.747662339933337,
109.601600176307));
#67538=CARTESIAN_POINT('Ctrl Pts',(5.6879438639411,7.46821641632047,109.919403315715));
#67539=CARTESIAN_POINT('Ctrl Pts',(-3.19084854132404,8.82155865995665,110.237206455123));
#67540=CARTESIAN_POINT('Ctrl Pts',(-9.14937463317463,2.10140563960524,110.55500959453));
#67541=CARTESIAN_POINT('Ctrl Pts',(-6.71472221522252,-6.56152297127247,
110.872812733938));
#67542=CARTESIAN_POINT('Ctrl Pts',(0.435689170539254,-8.74515807356746,
111.137648683444));
#67543=CARTESIAN_POINT('Ctrl Pts',(5.31513815892038,-6.31158147059979,111.34951744305));
#67544=CARTESIAN_POINT('Ctrl Pts',(8.54349359153895,-1.91737634186406,111.561386202655));
#67545=CARTESIAN_POINT('Ctrl Pts',(7.60838723404739,5.50032015676579,111.826222152161));
#67546=CARTESIAN_POINT('Ctrl Pts',(-0.513940525685185,9.37351732149688,
112.144025291569));
#67547=CARTESIAN_POINT('Ctrl Pts',(-8.14997325281275,4.64535763781033,112.461828430977));
#67548=CARTESIAN_POINT('Ctrl Pts',(-8.32714604435014,-4.33423587226256,
112.779631570384));
#67549=CARTESIAN_POINT('Ctrl Pts',(-0.855650321852643,-9.34927487331794,
113.097434709792));
#67550=CARTESIAN_POINT('Ctrl Pts',(6.00326091836658,-6.37404684098099,113.362270659298));
#67551=CARTESIAN_POINT('Ctrl Pts',(8.13910105320298,-1.35712503262605,113.574139418903));
#67552=CARTESIAN_POINT('Ctrl Pts',(7.74661230987278,4.08137385025368,113.786008178509));
#67553=CARTESIAN_POINT('Ctrl Pts',(2.22412460764706,9.12109356710027,114.050844128015));
#67554=CARTESIAN_POINT('Ctrl Pts',(-6.47034298326984,6.80158977880867,114.368647267423));
#67555=CARTESIAN_POINT('Ctrl Pts',(-9.21629115066875,-1.74968255144495,
114.68645040683));
#67556=CARTESIAN_POINT('Ctrl Pts',(-3.52748466476459,-8.69964446286136,
115.004253546238));
#67557=CARTESIAN_POINT('Ctrl Pts',(5.41212001747173,-7.67137764985019,115.322056685646));
#67558=CARTESIAN_POINT('Ctrl Pts',(8.70339564743194,-0.958393963497642,
115.586892635152));
#67559=CARTESIAN_POINT('Ctrl Pts',(7.0754502027632,4.2455575295418,115.798761394757));
#67560=CARTESIAN_POINT('Ctrl Pts',(3.24958818761061,8.13066979995796,116.010630154362));
#67561=CARTESIAN_POINT('Ctrl Pts',(-4.22248352081092,8.38520787140186,116.275466103869));
#67562=CARTESIAN_POINT('Ctrl Pts',(-9.33620827337083,0.980906171142857,
116.593269243276));
#67563=CARTESIAN_POINT('Ctrl Pts',(-5.88047914271609,-7.30899286200274,
116.911072382684));
#67564=CARTESIAN_POINT('Ctrl Pts',(2.9570676846459,-8.90969766876333,117.228875522091));
#67565=CARTESIAN_POINT('Ctrl Pts',(9.09480976491298,-2.32927316349603,117.546678661499));
#67566=CARTESIAN_POINT('Ctrl Pts',(7.24638325133705,4.91503250851395,117.811514611005));
#67567=CARTESIAN_POINT('Ctrl Pts',(2.63223479371206,7.82036407715153,118.023383370611));
#67568=CARTESIAN_POINT('Ctrl Pts',(-2.79959060385439,8.29637916417864,118.235252130216));
#67569=CARTESIAN_POINT('Ctrl Pts',(-8.65223685596117,3.64415635209118,118.500088079723));
#67570=CARTESIAN_POINT('Ctrl Pts',(-7.74266565467541,-5.30830390993709,
118.81789121913));
#67571=CARTESIAN_POINT('Ctrl Pts',(0.264123589339781,-9.37718776255869,
119.135694358538));
#67572=CARTESIAN_POINT('Ctrl Pts',(8.02918678132282,-4.86406429552229,119.453497497945));
#67573=CARTESIAN_POINT('Ctrl Pts',(8.43339477442419,4.12540067252307,119.771300637353));
#67574=CARTESIAN_POINT('Ctrl Pts',(2.32816071136047,8.44081053495957,120.036136586859));
#67575=CARTESIAN_POINT('Ctrl Pts',(-3.06825855014793,7.6598005050964,120.248005346464));
#67576=CARTESIAN_POINT('Ctrl Pts',(-7.51155453092633,4.49935143258734,120.45987410607));
#67577=CARTESIAN_POINT('Ctrl Pts',(-8.94927888749763,-2.83751396893987,
120.724710055576));
#67578=CARTESIAN_POINT('Ctrl Pts',(-2.45086530172317,-9.06202080736714,
121.042513194984));
#67579=CARTESIAN_POINT('Ctrl Pts',(6.28256859347107,-6.96640104164675,121.360316334391));
#67580=CARTESIAN_POINT('Ctrl Pts',(9.26619230882614,1.50487273089625,121.678119473799));
#67581=CARTESIAN_POINT('Ctrl Pts',(3.7437976511162,8.60959100524735,121.995922613207));
#67582=CARTESIAN_POINT('Ctrl Pts',(-3.70209981932849,7.93486431596248,122.260758562713));
#67583=CARTESIAN_POINT('Ctrl Pts',(-7.30320870515385,3.8405594536989,122.472627322318));
#67584=CARTESIAN_POINT('Ctrl Pts',(-8.63565016053205,-1.44677610220397,
122.684496081923));
#67585=CARTESIAN_POINT('Ctrl Pts',(-4.97172850631308,-7.96385546011813,
122.94933203143));
#67586=CARTESIAN_POINT('Ctrl Pts',(4.01158246931131,-8.4872945001489,123.267135170837));
#67587=CARTESIAN_POINT('Ctrl Pts',(9.30016622434986,-1.22813672047871,123.584938310245));
#67588=CARTESIAN_POINT('Ctrl Pts',(6.07723281321958,7.15501245102138,123.902741449653));
#67589=CARTESIAN_POINT('Ctrl Pts',(-2.73401159915763,8.9814396789051,124.22054458906));
#67590=CARTESIAN_POINT('Ctrl Pts',(-7.96406504960543,3.63885733035252,124.485380538567));
#67591=CARTESIAN_POINT('Ctrl Pts',(-8.04980623286806,-1.81311166829539,
124.697249298172));
#67592=CARTESIAN_POINT('Ctrl Pts',(-5.63495706479247,-6.70185598643782,
124.909118057777));
#67593=CARTESIAN_POINT('Ctrl Pts',(1.38055096962363,-9.28628866396099,125.173954007283));
#67594=CARTESIAN_POINT('Ctrl Pts',(8.55791161203055,-3.85864104070546,125.491757146691));
#67595=CARTESIAN_POINT('Ctrl Pts',(7.87557130771675,5.09674289932255,125.809560286099));
#67596=CARTESIAN_POINT('Ctrl Pts',(-0.0144961233994668,9.38758497712538,
126.127363425506));
#67597=CARTESIAN_POINT('Ctrl Pts',(-7.90592957204853,5.0633344479649,126.445166564914));
#67598=CARTESIAN_POINT('Ctrl Pts',(-8.42202188284641,-2.39523739739133,
126.71000251442));
#67599=CARTESIAN_POINT('Ctrl Pts',(-4.95144138099217,-6.60075621114956,
126.921871274026));
#67600=CARTESIAN_POINT('Ctrl Pts',(0.0572539753503746,-8.75581731006953,
127.13374003363));
#67601=CARTESIAN_POINT('Ctrl Pts',(7.07341500278416,-6.17315788948633,127.398575983137));
#67602=CARTESIAN_POINT('Ctrl Pts',(9.01658358087113,2.61307909744599,127.716379122545));
#67603=CARTESIAN_POINT('Ctrl Pts',(2.68923672680319,8.98718072767756,128.034182261952));
#67604=CARTESIAN_POINT('Ctrl Pts',(-6.09930103632042,7.1362096878304,128.35198540136));
#67605=CARTESIAN_POINT('Ctrl Pts',(-9.30160735966655,-1.273255142042,128.669788540768));
#67606=CARTESIAN_POINT('Ctrl Pts',(-4.85722880598274,-7.28525518505279,
128.934624490274));
#67607=CARTESIAN_POINT('Ctrl Pts',(0.51196248970237,-8.23557215483952,129.146493249879));
#67608=CARTESIAN_POINT('Ctrl Pts',(5.7221178502404,-6.62759248090642,129.358362009484));
#67609=CARTESIAN_POINT('Ctrl Pts',(9.38768658363369,-0.111439389827381,
129.623197958991));
#67610=CARTESIAN_POINT('Ctrl Pts',(5.168515280694,7.8366709535093,129.941001098399));
#67611=CARTESIAN_POINT('Ctrl Pts',(-3.78160256705032,8.58492245914921,130.258804237806));
#67612=CARTESIAN_POINT('Ctrl Pts',(-9.27079569704023,1.4762482799598,130.576607377214));
#67613=CARTESIAN_POINT('Ctrl Pts',(-6.25440424642379,-7.00167877386955,
130.894410516621));
#67614=CARTESIAN_POINT('Ctrl Pts',(1.02760297588888,-8.69549578281488,131.159246466128));
#67615=CARTESIAN_POINT('Ctrl Pts',(5.73082923046837,-5.93669526248734,131.371115225733));
#67616=CARTESIAN_POINT('Ctrl Pts',(8.65383173005065,-1.3337208002335,131.582983985338));
#67617=CARTESIAN_POINT('Ctrl Pts',(7.21796181708323,6.00350775274488,131.847819934845));
#67618=CARTESIAN_POINT('Ctrl Pts',(-1.14827664309823,9.31710376626014,132.165623074252));
#67619=CARTESIAN_POINT('Ctrl Pts',(-8.44617234530928,4.08210537811788,132.48342621366));
#67620=CARTESIAN_POINT('Ctrl Pts',(-8.01412654203442,-4.88883806324193,
132.801229353067));
#67621=CARTESIAN_POINT('Ctrl Pts',(-0.219806363843781,-9.38577451745743,
133.119032492475));
#67622=CARTESIAN_POINT('Ctrl Pts',(6.4216037154782,-5.95236259869669,133.383868441981));
#67623=CARTESIAN_POINT('Ctrl Pts',(8.21238501522175,-0.802176208942004,
133.595737201587));
#67624=CARTESIAN_POINT('Ctrl Pts',(7.45207252009975,4.59719805318194,133.807605961192));
#67625=CARTESIAN_POINT('Ctrl Pts',(1.60060230738995,9.25089997695995,134.072441910698));
#67626=CARTESIAN_POINT('Ctrl Pts',(-6.91659816072736,6.34725387261032,134.390245050106));
#67627=CARTESIAN_POINT('Ctrl Pts',(-9.07645682777433,-2.37051535710585,
134.708048189513));
#67628=CARTESIAN_POINT('Ctrl Pts',(-2.92953728957566,-8.91878764795583,
135.025851328922));
#67629=CARTESIAN_POINT('Ctrl Pts',(5.91978127567269,-7.28678720550658,135.343654468329));
#67630=CARTESIAN_POINT('Ctrl Pts',(8.7483474319312,-0.366103803899804,135.608490417835));
#67631=CARTESIAN_POINT('Ctrl Pts',(6.77132322176431,4.7154995636545,135.82035917744));
#67632=CARTESIAN_POINT('Ctrl Pts',(2.69085639145085,8.33228100015807,136.032227937046));
#67633=CARTESIAN_POINT('Ctrl Pts',(-4.78127941297109,8.07963150801064,136.297063886552));
#67634=CARTESIAN_POINT('Ctrl Pts',(-9.38123025361558,0.345659903649954,
136.61486702596));
#67635=CARTESIAN_POINT('Ctrl Pts',(-5.37140278988185,-7.69086755012565,
136.932670165367));
#67636=CARTESIAN_POINT('Ctrl Pts',(3.55433541669274,-8.68870885609521,137.250473304775));
#67637=CARTESIAN_POINT('Ctrl Pts',(9.23180566187414,-1.70729093933327,137.568276444182));
#67638=CARTESIAN_POINT('Ctrl Pts',(6.89647295730047,5.39502321906315,137.833112393689));
#67639=CARTESIAN_POINT('Ctrl Pts',(2.0959620806498,7.98083311847255,138.044981153294));
#67640=CARTESIAN_POINT('Ctrl Pts',(-3.35563807741036,8.08747846231697,138.256849912899));
#67641=CARTESIAN_POINT('Ctrl Pts',(-8.87939939579868,3.04915471893925,138.521685862406));
#67642=CARTESIAN_POINT('Ctrl Pts',(-7.36494984302657,-5.82103733453466,
138.839489001813));
#67643=CARTESIAN_POINT('Ctrl Pts',(0.89928339557674,-9.33770319613803,139.157292141221));
#67644=CARTESIAN_POINT('Ctrl Pts',(8.34049198343126,-4.30849803465926,139.475095280629));
#67645=CARTESIAN_POINT('Ctrl Pts',(8.13428968912092,4.68768699718746,139.792898420036));
#67646=CARTESIAN_POINT('Ctrl Pts',(1.75052179242454,8.57923587735251,140.057734369543));
#67647=CARTESIAN_POINT('Ctrl Pts',(-3.58052817041019,7.43414906558445,140.269603129148));
#67648=CARTESIAN_POINT('Ctrl Pts',(-7.79932351038639,3.97971953350241,140.481471888753));
#67649=CARTESIAN_POINT('Ctrl Pts',(-8.73630466580453,-3.43774037943266,
140.746307838259));
#67650=CARTESIAN_POINT('Ctrl Pts',(-1.83082636208119,-9.20733602472795,
141.064110977667));
#67651=CARTESIAN_POINT('Ctrl Pts',(6.74042994684304,-6.52441688861351,141.381914117074));
#67652=CARTESIAN_POINT('Ctrl Pts',(9.14284111731162,2.12965211805653,141.699717256482));
#67653=CARTESIAN_POINT('Ctrl Pts',(3.15145810322174,8.84360729305531,142.01752039589));
#67654=CARTESIAN_POINT('Ctrl Pts',(-4.23156011172795,7.66560589945927,142.282356345396));
#67655=CARTESIAN_POINT('Ctrl Pts',(-7.54679140282833,3.33656917066706,142.494225105002));
#67656=CARTESIAN_POINT('Ctrl Pts',(-8.51768877835491,-2.02893880145877,
142.706093864606));
#67657=CARTESIAN_POINT('Ctrl Pts',(-4.42034393072991,-8.28261055852364,
142.970929814113));
#67658=CARTESIAN_POINT('Ctrl Pts',(4.57778506083285,-8.19578219435772,143.288732953521));
#67659=CARTESIAN_POINT('Ctrl Pts',(9.3620332174066,-0.59476519788765,143.606536092929));
#67660=CARTESIAN_POINT('Ctrl Pts',(5.57814350230469,7.55058122980996,143.924339232336));
#67661=CARTESIAN_POINT('Ctrl Pts',(-3.33665665318324,8.77540885145237,144.242142371744));
#67662=CARTESIAN_POINT('Ctrl Pts',(-8.19245181991234,3.09052551540061,144.50697832125));
#67663=CARTESIAN_POINT('Ctrl Pts',(-7.90835556671305,-2.35471156201695,
144.718847080855));
#67664=CARTESIAN_POINT('Ctrl Pts',(-5.1676091709004,-7.06848146653319,144.93071584046));
#67665=CARTESIAN_POINT('Ctrl Pts',(2.00697894421316,-9.17132016854132,145.195551789967));
#67666=CARTESIAN_POINT('Ctrl Pts',(8.79983312769516,-3.2695410673115,145.513354929374));
#67667=CARTESIAN_POINT('Ctrl Pts',(7.51189338113173,5.61897405460601,145.831158068782));
#67668=CARTESIAN_POINT('Ctrl Pts',(-0.650935249830781,9.36500107153992,
146.14896120819));
#67669=CARTESIAN_POINT('Ctrl Pts',(-8.23102879335794,4.51566643132572,146.466764347598));
#67670=CARTESIAN_POINT('Ctrl Pts',(-8.24024695947341,-2.9607338092988,146.731600297104));
#67671=CARTESIAN_POINT('Ctrl Pts',(-4.49252079448732,-6.92127236495981,
146.943469056709));
#67672=CARTESIAN_POINT('Ctrl Pts',(0.650761301820232,-8.73178820528528,
147.155337816314));
#67673=CARTESIAN_POINT('Ctrl Pts',(7.4756751106369,-5.67938002490987,147.420173765821));
#67674=CARTESIAN_POINT('Ctrl Pts',(8.81867118648771,3.21838501357198,147.737976905228));
#67675=CARTESIAN_POINT('Ctrl Pts',(2.0737231238013,9.14882984880614,148.055780044636));
#67676=CARTESIAN_POINT('Ctrl Pts',(-6.56909649240655,6.70625973837498,148.373583184043));
#67677=CARTESIAN_POINT('Ctrl Pts',(-9.193879243756,-1.90096763361108,148.691386323451));
#67678=CARTESIAN_POINT('Ctrl Pts',(-4.35211456730083,-7.59781044961311,
148.956222272958));
#67679=CARTESIAN_POINT('Ctrl Pts',(1.06914875867794,-8.18190888238425,149.168091032563));
#67680=CARTESIAN_POINT('Ctrl Pts',(6.15830368944283,-6.22439167206857,149.379959792168));
#67681=CARTESIAN_POINT('Ctrl Pts',(9.3736282979707,0.525308135358659,149.644795741674));
#67682=CARTESIAN_POINT('Ctrl Pts',(4.62532190065374,8.1690410535072,149.962598881082));
#67683=CARTESIAN_POINT('Ctrl Pts',(-4.35499181730632,8.30881398094853,150.28040202049));
#67684=CARTESIAN_POINT('Ctrl Pts',(-9.34947948145903,0.844229048237673,
150.598205159897));
#67685=CARTESIAN_POINT('Ctrl Pts',(-5.76544724662711,-7.40947736302889,
150.916008299305));
#67686=CARTESIAN_POINT('Ctrl Pts',(1.61503940058015,-8.60605247318171,151.180844248811));
#67687=CARTESIAN_POINT('Ctrl Pts',(6.11981070531535,-5.53417288230174,151.392713008416));
#67688=CARTESIAN_POINT('Ctrl Pts',(8.72516264438353,-0.744694817129546,
151.604581768021));
#67689=CARTESIAN_POINT('Ctrl Pts',(6.79258094058841,6.48069683519393,151.869417717528));
#67690=CARTESIAN_POINT('Ctrl Pts',(-1.77440860364534,9.21507589793784,152.187220856935));
#67691=CARTESIAN_POINT('Ctrl Pts',(-8.70886625593951,3.50508210372682,152.505023996343));
#67692=CARTESIAN_POINT('Ctrl Pts',(-7.6538609868877,-5.43052651898935,152.822827135751));
#67693=CARTESIAN_POINT('Ctrl Pts',(-0.9466795259243,-8.7045547712713,153.087663085258));
#67694=CARTESIAN_POINT('Ctrl Pts',(4.27613052328954,-7.06725396548898,153.299535285551));
#67695=CARTESIAN_POINT('Ctrl Pts',(6.18792442894812,-5.14458818350946,153.405473106043));
#67696=CARTESIAN_POINT('Ctrl Pts',(6.85423122541137,-4.00395918922165,153.458443736632));
#67697=CARTESIAN_POINT('Ctrl Pts',(4.37750802528476,-6.14572094339974,-0.44955678837992));
#67698=CARTESIAN_POINT('Ctrl Pts',(5.40128695262251,-5.41652500898836,-0.396532856746831));
#67699=CARTESIAN_POINT('Ctrl Pts',(7.05805613175304,-3.44046858888462,-0.290541735212461));
#67700=CARTESIAN_POINT('Ctrl Pts',(8.15840353697748,1.64586779412391,-0.078616233875533));
#67701=CARTESIAN_POINT('Ctrl Pts',(4.48144417158412,7.71305662036539,0.186219715630859));
#67702=CARTESIAN_POINT('Ctrl Pts',(-4.06808443251202,7.94213116854575,0.504022855038533));
#67703=CARTESIAN_POINT('Ctrl Pts',(-8.87604082525919,0.88600865987949,0.821825994446204));
#67704=CARTESIAN_POINT('Ctrl Pts',(-5.54974215001441,-6.98819881157078,
1.13962913385388));
#67705=CARTESIAN_POINT('Ctrl Pts',(1.45643916438736,-8.1953082696198,1.40446508336027));
#67706=CARTESIAN_POINT('Ctrl Pts',(5.76587662434617,-5.31650462948363,1.61633384296539));
#67707=CARTESIAN_POINT('Ctrl Pts',(8.28579825562455,-0.787600779429617,
1.8282026025705));
#67708=CARTESIAN_POINT('Ctrl Pts',(6.51741451893584,6.09588472696246,2.0930385520769));
#67709=CARTESIAN_POINT('Ctrl Pts',(-1.60443270220511,8.77772874853394,2.41084169148457));
#67710=CARTESIAN_POINT('Ctrl Pts',(-8.24041566903942,3.40690648579429,2.72864483089224));
#67711=CARTESIAN_POINT('Ctrl Pts',(-7.33463407283986,-5.0820354846744,3.04644797029991));
#67712=CARTESIAN_POINT('Ctrl Pts',(0.310075852972152,-8.91854603754864,
3.36425110970758));
#67713=CARTESIAN_POINT('Ctrl Pts',(6.42256967722955,-5.29349487006409,3.62908705921399));
#67714=CARTESIAN_POINT('Ctrl Pts',(7.83727650840871,-0.30737883443838,3.84095581881909));
#67715=CARTESIAN_POINT('Ctrl Pts',(6.81742465965292,4.77421110570834,4.05282457842421));
#67716=CARTESIAN_POINT('Ctrl Pts',(1.00763813107558,8.86687601910892,4.3176605279306));
#67717=CARTESIAN_POINT('Ctrl Pts',(-6.91409890044602,5.64085818235034,4.63546366733828));
#67718=CARTESIAN_POINT('Ctrl Pts',(-8.48189338148272,-2.75101947129031,
4.95326680674595));
#67719=CARTESIAN_POINT('Ctrl Pts',(-2.28705349793356,-8.62516345681626,
5.27106994615362));
#67720=CARTESIAN_POINT('Ctrl Pts',(6.02011300233425,-6.5874918155073,5.5888730855613));
#67721=CARTESIAN_POINT('Ctrl Pts',(8.32177000704095,0.136037560988745,5.85370903506768));
#67722=CARTESIAN_POINT('Ctrl Pts',(6.16490436238276,4.84885317968135,6.0655777946728));
#67723=CARTESIAN_POINT('Ctrl Pts',(2.09297402488047,8.05542185077758,6.27744655427792));
#67724=CARTESIAN_POINT('Ctrl Pts',(-4.98357195312415,7.40275771703265,6.54228250378431));
#67725=CARTESIAN_POINT('Ctrl Pts',(-8.9211994880889,-0.190411152840623,
6.86008564319199));
#67726=CARTESIAN_POINT('Ctrl Pts',(-4.67206071950657,-7.59489755336788,
7.17788878259965));
#67727=CARTESIAN_POINT('Ctrl Pts',(3.85295055711175,-8.04852960516554,7.49569192200733));
#67728=CARTESIAN_POINT('Ctrl Pts',(8.85465174940877,-1.10993398241913,7.813495061415));
#67729=CARTESIAN_POINT('Ctrl Pts',(6.24611106307449,5.50058707593904,8.07833101092139));
#67730=CARTESIAN_POINT('Ctrl Pts',(1.54788443075806,7.68904914853577,8.29019977052652));
#67731=CARTESIAN_POINT('Ctrl Pts',(-3.63117674040154,7.48898638465389,8.50206853013162));
#67732=CARTESIAN_POINT('Ctrl Pts',(-8.59439695939712,2.40273843072248,8.76690447963802));
#67733=CARTESIAN_POINT('Ctrl Pts',(-6.6671191886872,-5.93073170032617,9.0847076190457));
#67734=CARTESIAN_POINT('Ctrl Pts',(1.3693654792293,-8.81109859239982,9.40251075845336));
#67735=CARTESIAN_POINT('Ctrl Pts',(8.15260611885662,-3.62754328002339,9.72031389786104));
#67736=CARTESIAN_POINT('Ctrl Pts',(7.45979632555549,4.89778009329165,10.0381170372687));
#67737=CARTESIAN_POINT('Ctrl Pts',(1.18701860120112,8.23779997522517,10.3029529867751));
#67738=CARTESIAN_POINT('Ctrl Pts',(-3.80847721506004,6.85659713857236,10.5148217463803));
#67739=CARTESIAN_POINT('Ctrl Pts',(-7.62090835848221,3.34546220768456,10.7266905059854));
#67740=CARTESIAN_POINT('Ctrl Pts',(-8.10013769775553,-3.74494063216588,
10.9915264554918));
#67741=CARTESIAN_POINT('Ctrl Pts',(-1.22851223754719,-8.83825856488072,
11.3093295948994));
#67742=CARTESIAN_POINT('Ctrl Pts',(6.75671894445668,-5.81870856174881,11.6271327343071));
#67743=CARTESIAN_POINT('Ctrl Pts',(8.55819728856564,2.52612666892943,11.9449358737148));
#67744=CARTESIAN_POINT('Ctrl Pts',(2.50179473315566,8.56608628103863,12.2627390131224));
#67745=CARTESIAN_POINT('Ctrl Pts',(-4.43904923015306,7.04025592743055,12.5275749626288));
#67746=CARTESIAN_POINT('Ctrl Pts',(-7.3457327618181,2.74911498672665,12.739443722234));
#67747=CARTESIAN_POINT('Ctrl Pts',(-7.97053919776979,-2.39601053592402,
12.9513124818391));
#67748=CARTESIAN_POINT('Ctrl Pts',(-3.73687540473799,-8.10386162705828,
13.2161484313455));
#67749=CARTESIAN_POINT('Ctrl Pts',(4.79688937669392,-7.52422149363303,13.5339515707531));
#67750=CARTESIAN_POINT('Ctrl Pts',(8.91674874505521,-0.0470323134403838,
13.8517547101608));
#67751=CARTESIAN_POINT('Ctrl Pts',(4.87599483198481,7.47320086548901,14.1695578495685));
#67752=CARTESIAN_POINT('Ctrl Pts',(-3.65118054584055,8.14283069225432,14.4873609889762));
#67753=CARTESIAN_POINT('Ctrl Pts',(-7.94482039878572,2.47995774610828,14.7521969384825));
#67754=CARTESIAN_POINT('Ctrl Pts',(-7.37432421124854,-2.67147252385011,
14.9640656980877));
#67755=CARTESIAN_POINT('Ctrl Pts',(-4.51306928532146,-6.99303705247811,
15.1759344576928));
#67756=CARTESIAN_POINT('Ctrl Pts',(2.41129262796859,-8.59200086844431,15.4407704071992));
#67757=CARTESIAN_POINT('Ctrl Pts',(8.53107320768763,-2.616265793562,15.7585735466068));
#67758=CARTESIAN_POINT('Ctrl Pts',(6.817724044067,5.74710875831507,16.0763766860145));
#67759=CARTESIAN_POINT('Ctrl Pts',(-1.13520985765706,8.85072626153168,16.3941798254222));
#67760=CARTESIAN_POINT('Ctrl Pts',(-8.0601819410273,3.83017990942736,16.7119829648299));
#67761=CARTESIAN_POINT('Ctrl Pts',(-7.65577531194065,-3.26488375972616,
16.9768189143363));
#67762=CARTESIAN_POINT('Ctrl Pts',(-3.88059495544502,-6.81604033219195,
17.1886876739414));
#67763=CARTESIAN_POINT('Ctrl Pts',(1.1000527157068,-8.24986336942072,17.4005564335465));
#67764=CARTESIAN_POINT('Ctrl Pts',(7.40771499469042,-4.97620031936837,17.6653923830529));
#67765=CARTESIAN_POINT('Ctrl Pts',(8.19041913672562,3.54134030308396,17.9831955224606));
#67766=CARTESIAN_POINT('Ctrl Pts',(1.46223680155422,8.79616301333324,18.3009986618682));
#67767=CARTESIAN_POINT('Ctrl Pts',(-6.60418544645305,6.00073256914073,18.6188018012759));
#67768=CARTESIAN_POINT('Ctrl Pts',(-8.61926503515426,-2.31194319022132,
18.9366049406836));
#67769=CARTESIAN_POINT('Ctrl Pts',(-3.70997536547946,-7.45026471871834,
19.20144089019));
#67770=CARTESIAN_POINT('Ctrl Pts',(1.46668719125818,-7.70494981822022,19.4133096497951));
#67771=CARTESIAN_POINT('Ctrl Pts',(6.18773830434186,-5.56617070061853,19.6251784094002));
#67772=CARTESIAN_POINT('Ctrl Pts',(8.86586766281804,1.01646527065157,19.8900143589066));
#67773=CARTESIAN_POINT('Ctrl Pts',(3.93763941419164,8.00743733171186,20.2078174983143));
#67774=CARTESIAN_POINT('Ctrl Pts',(-4.5916828416135,7.6437601285613,20.5256206377219));
#67775=CARTESIAN_POINT('Ctrl Pts',(-8.91869447358585,0.284509515337135,
20.8434237771296));
#67776=CARTESIAN_POINT('Ctrl Pts',(-5.06138570295972,-7.34977454259096,
21.1612269165373));
#67777=CARTESIAN_POINT('Ctrl Pts',(2.00788160904171,-8.07705224915103,21.4260628660437));
#67778=CARTESIAN_POINT('Ctrl Pts',(6.11341122390523,-4.91361641011203,21.6379316256488));
#67779=CARTESIAN_POINT('Ctrl Pts',(8.31987188256932,-0.223815658693506,
21.8498003852539));
#67780=CARTESIAN_POINT('Ctrl Pts',(6.08926900404114,6.52361970515354,22.1146363347603));
#67781=CARTESIAN_POINT('Ctrl Pts',(-2.19594028960663,8.64880934128916,22.432439474168));
#67782=CARTESIAN_POINT('Ctrl Pts',(-8.45240090026003,2.84034139536688,22.7502426135756));
#67783=CARTESIAN_POINT('Ctrl Pts',(-6.97321962856273,-5.56760853412987,
23.0680457529833));
#67784=CARTESIAN_POINT('Ctrl Pts',(0.914047176923553,-8.8770112548876,23.385848892391));
#67785=CARTESIAN_POINT('Ctrl Pts',(6.76668080923863,-4.84586343362311,23.6506848418974));
#67786=CARTESIAN_POINT('Ctrl Pts',(7.8400853215732,0.224689049010087,23.8625536015025));
#67787=CARTESIAN_POINT('Ctrl Pts',(6.47804714849922,5.2254441661226,24.0744223611076));
#67788=CARTESIAN_POINT('Ctrl Pts',(0.404151858925233,8.91478952841686,24.339258310614));
#67789=CARTESIAN_POINT('Ctrl Pts',(-7.28063663433841,5.15910718789769,24.6570614500217));
#67790=CARTESIAN_POINT('Ctrl Pts',(-8.27585861517074,-3.31975667823038,
24.9748645894293));
#67791=CARTESIAN_POINT('Ctrl Pts',(-1.69701030859419,-8.76037743422127,
25.292667728837));
#67792=CARTESIAN_POINT('Ctrl Pts',(6.45288855301478,-6.16417394169035,25.6104708682447));
#67793=CARTESIAN_POINT('Ctrl Pts',(8.2933980942229,0.699935455727023,25.8753068177511));
#67794=CARTESIAN_POINT('Ctrl Pts',(5.82196951471606,5.25567255334745,26.0871755773562));
#67795=CARTESIAN_POINT('Ctrl Pts',(1.54200537880764,8.1787884801584,26.2990443369613));
#67796=CARTESIAN_POINT('Ctrl Pts',(-5.47400703753924,7.04784066321128,26.5638802864678));
#67797=CARTESIAN_POINT('Ctrl Pts',(-8.88776182410288,-0.794824845804046,
26.8816834258753));
#67798=CARTESIAN_POINT('Ctrl Pts',(-4.14638080422807,-7.89418434338091,
27.1994865652831));
#67799=CARTESIAN_POINT('Ctrl Pts',(4.38977017365657,-7.76878205383336,27.5172897046907));
#67800=CARTESIAN_POINT('Ctrl Pts',(8.90952981045906,-0.507040055206927,
27.8350928440984));
#67801=CARTESIAN_POINT('Ctrl Pts',(5.8588021812506,5.91141257166313,28.0999287936048));
#67802=CARTESIAN_POINT('Ctrl Pts',(1.02300990719647,7.77630206126733,28.3117975532099));
#67803=CARTESIAN_POINT('Ctrl Pts',(-4.13056997928662,7.22556248590099,28.523666312815));
#67804=CARTESIAN_POINT('Ctrl Pts',(-8.73752521892493,1.81451484140921,28.7885022623214));
#67805=CARTESIAN_POINT('Ctrl Pts',(-6.24967801580441,-6.36911151388161,
29.1063054017291));
#67806=CARTESIAN_POINT('Ctrl Pts',(1.96360159806944,-8.69798189150852,29.4241085411368));
#67807=CARTESIAN_POINT('Ctrl Pts',(8.37979196576129,-3.06645453056966,29.7419116805444));
#67808=CARTESIAN_POINT('Ctrl Pts',(7.11056466570447,5.39227977722585,30.0597148199521));
#67809=CARTESIAN_POINT('Ctrl Pts',(0.625769470583524,8.29932371709461,30.3245507694585));
#67810=CARTESIAN_POINT('Ctrl Pts',(-4.26458687907389,6.5826075205137,30.5364195290636));
#67811=CARTESIAN_POINT('Ctrl Pts',(-7.83019273241325,2.8210713150692,30.7482882886687));
#67812=CARTESIAN_POINT('Ctrl Pts',(-7.82759440220744,-4.28550778036562,
31.0131242381751));
#67813=CARTESIAN_POINT('Ctrl Pts',(-0.626456906038276,-8.90121387914958,
31.3309273775828));
#67814=CARTESIAN_POINT('Ctrl Pts',(7.13567642164131,-5.34721817645243,31.6487305169904));
#67815=CARTESIAN_POINT('Ctrl Pts',(8.36723482303544,3.10055449777475,31.9665336563982));
#67816=CARTESIAN_POINT('Ctrl Pts',(1.9152626593684,8.7159956405836,32.2843367958058));
#67817=CARTESIAN_POINT('Ctrl Pts',(-4.90615988468414,6.72309131109787,32.5491727453122));
#67818=CARTESIAN_POINT('Ctrl Pts',(-7.51521834715023,2.24475304052566,32.7610415049173));
#67819=CARTESIAN_POINT('Ctrl Pts',(-7.78975074234866,-2.93089490830397,
32.9729102645224));
#67820=CARTESIAN_POINT('Ctrl Pts',(-3.17883992582329,-8.33857228709058,
33.2377462140288));
#67821=CARTESIAN_POINT('Ctrl Pts',(5.2959891995192,-7.18168191832974,33.5555493534365));
#67822=CARTESIAN_POINT('Ctrl Pts',(8.89941983940671,0.557625988388055,33.8733524928441));
#67823=CARTESIAN_POINT('Ctrl Pts',(4.35809662169856,7.7865942884825,34.1911556322519));
#67824=CARTESIAN_POINT('Ctrl Pts',(-4.19485799716548,7.87654603520225,34.5089587716595));
#67825=CARTESIAN_POINT('Ctrl Pts',(-8.09467877277286,1.9355973643979,34.7737947211659));
#67826=CARTESIAN_POINT('Ctrl Pts',(-7.17623150848824,-3.16530004184014,
34.9856634807711));
#67827=CARTESIAN_POINT('Ctrl Pts',(-4.02856098714868,-7.28292921593141,
35.1975322403761));
#67828=CARTESIAN_POINT('Ctrl Pts',(2.98827655480704,-8.40874629734028,35.4623681898826));
#67829=CARTESIAN_POINT('Ctrl Pts',(8.6888242006846,-2.03184418376158,35.7801713292902));
#67830=CARTESIAN_POINT('Ctrl Pts',(6.41238584802353,6.19612200953295,36.0979744686979));
#67831=CARTESIAN_POINT('Ctrl Pts',(-1.73267150616142,8.75339398343433,36.4157776081056));
#67832=CARTESIAN_POINT('Ctrl Pts',(-8.30131909715377,3.27489119029515,36.7335807475132));
#67833=CARTESIAN_POINT('Ctrl Pts',(-7.41680206625722,-3.77642803471834,
36.9984166970196));
#67834=CARTESIAN_POINT('Ctrl Pts',(-3.40954226567329,-7.0634583991753,37.2102854566248));
#67835=CARTESIAN_POINT('Ctrl Pts',(1.65685712726635,-8.15629732484478,37.4221542162298));
#67836=CARTESIAN_POINT('Ctrl Pts',(7.72805297274963,-4.46251143543848,37.6869901657363));
#67837=CARTESIAN_POINT('Ctrl Pts',(7.93147207832679,4.08849696688301,38.0047933051439));
#67838=CARTESIAN_POINT('Ctrl Pts',(0.862497716326057,8.8750615721968,38.3225964445516));
#67839=CARTESIAN_POINT('Ctrl Pts',(-6.9958350228475,5.53916501925954,38.6403995839592));
#67840=CARTESIAN_POINT('Ctrl Pts',(-8.44268355926215,-2.89100421639401,
38.958202723367));
#67841=CARTESIAN_POINT('Ctrl Pts',(-3.19631525253309,-7.68465551588802,
39.2230386728733));
#67842=CARTESIAN_POINT('Ctrl Pts',(1.98570316394913,-7.58778004181559,39.4349074324785));
#67843=CARTESIAN_POINT('Ctrl Pts',(6.55088310895129,-5.13383794877675,39.6467761920836));
#67844=CARTESIAN_POINT('Ctrl Pts',(8.77655135391446,1.6152267311884,39.91161214159));
#67845=CARTESIAN_POINT('Ctrl Pts',(3.38567948004545,8.25598154285045,40.2294152809976));
#67846=CARTESIAN_POINT('Ctrl Pts',(-5.0993594958464,7.314858368627,40.5472184204053));
#67847=CARTESIAN_POINT('Ctrl Pts',(-8.91746189895706,-0.320827146821168,
40.865021559813));
#67848=CARTESIAN_POINT('Ctrl Pts',(-4.55142913228414,-7.67602135971745,
41.1828246992206));
#67849=CARTESIAN_POINT('Ctrl Pts',(2.55088059539345,-7.92233360692975,41.4476606487271));
#67850=CARTESIAN_POINT('Ctrl Pts',(6.43248427759269,-4.487824532757,41.6595294083321));
#67851=CARTESIAN_POINT('Ctrl Pts',(8.31590220794029,0.340781542072778,41.8713981679373));
#67852=CARTESIAN_POINT('Ctrl Pts',(5.63296003724804,6.92145738120303,42.1362341174436));
#67853=CARTESIAN_POINT('Ctrl Pts',(-2.77727132720888,8.48002480848681,42.4540372568513));
#67854=CARTESIAN_POINT('Ctrl Pts',(-8.62552510820369,2.26073811590348,42.771840396259));
#67855=CARTESIAN_POINT('Ctrl Pts',(-6.57969363796116,-6.02757732493426,
43.0896435356667));
#67856=CARTESIAN_POINT('Ctrl Pts',(1.51379983280753,-8.79461318803933,43.4074466750743));
#67857=CARTESIAN_POINT('Ctrl Pts',(7.07965706273086,-4.37593618161517,43.6722826245808));
#67858=CARTESIAN_POINT('Ctrl Pts',(7.80681130486786,0.755724995272883,43.8841513841859));
#67859=CARTESIAN_POINT('Ctrl Pts',(6.10885909612371,5.6526278963992,44.096020143791));
#67860=CARTESIAN_POINT('Ctrl Pts',(-0.201195350454262,8.92167761645756,
44.3608560932973));
#67861=CARTESIAN_POINT('Ctrl Pts',(-7.61366799612502,4.65361326522414,44.6786592327051));
#67862=CARTESIAN_POINT('Ctrl Pts',(-8.03173819178576,-3.87321595570929,
44.9964623721127));
#67863=CARTESIAN_POINT('Ctrl Pts',(-1.09915724375289,-8.8552758359632,45.3142655115205));
#67864=CARTESIAN_POINT('Ctrl Pts',(6.85596749195023,-5.71248814531507,45.632068650928));
#67865=CARTESIAN_POINT('Ctrl Pts',(8.22685957920027,1.26061217492319,45.8969046004345));
#67866=CARTESIAN_POINT('Ctrl Pts',(5.45224164774619,5.6383050673828,46.1087733600396));
#67867=CARTESIAN_POINT('Ctrl Pts',(0.983940357573422,8.26451589412118,46.3206421196447));
#67868=CARTESIAN_POINT('Ctrl Pts',(-5.93925046802993,6.6604890915795,46.5854780691511));
#67869=CARTESIAN_POINT('Ctrl Pts',(-8.81342222062257,-1.3955807173089,46.9032812085587));
#67870=CARTESIAN_POINT('Ctrl Pts',(-3.60161903372427,-8.15714169037575,
47.2210843479665));
#67871=CARTESIAN_POINT('Ctrl Pts',(4.9063878437363,-7.45328216991178,47.5388874873741));
#67872=CARTESIAN_POINT('Ctrl Pts',(8.92340575765604,0.0981872969094068,
47.8566906267818));
#67873=CARTESIAN_POINT('Ctrl Pts',(5.44453079154443,6.29503344322871,48.1215265762882));
#67874=CARTESIAN_POINT('Ctrl Pts',(0.493427439442421,7.82776803311762,48.3333953358933));
#67875=CARTESIAN_POINT('Ctrl Pts',(-4.61095412314837,6.92888617785462,48.5452640954984));
#67876=CARTESIAN_POINT('Ctrl Pts',(-8.84044293923562,1.21794076176243,48.8101000450048));
#67877=CARTESIAN_POINT('Ctrl Pts',(-5.80347550407464,-6.77818034955503,
49.1279031844124));
#67878=CARTESIAN_POINT('Ctrl Pts',(2.54880112161379,-8.5448366317567,49.4457063238202));
#67879=CARTESIAN_POINT('Ctrl Pts',(8.56841358018594,-2.49125380007206,49.7635094632278));
#67880=CARTESIAN_POINT('Ctrl Pts',(6.72860982250429,5.86196391301944,50.0813126026355));
#67881=CARTESIAN_POINT('Ctrl Pts',(0.0616405167643138,8.32265354548276,
50.3461485521419));
#67882=CARTESIAN_POINT('Ctrl Pts',(-4.70107069550896,6.2783244049762,50.558017311747));
#67883=CARTESIAN_POINT('Ctrl Pts',(-8.00344215772086,2.28369770754799,50.7698860713521));
#67884=CARTESIAN_POINT('Ctrl Pts',(-7.51902811568601,-4.8063528019244,51.0347220208585));
#67885=CARTESIAN_POINT('Ctrl Pts',(-0.0215185877121976,-8.92320535053807,
51.3525251602661));
#67886=CARTESIAN_POINT('Ctrl Pts',(7.48179514989205,-4.85111961880997,51.6703282996739));
#67887=CARTESIAN_POINT('Ctrl Pts',(8.13776591363277,3.66071341577086,51.9881314390816));
#67888=CARTESIAN_POINT('Ctrl Pts',(1.31991644857489,8.82579354108318,52.3059345784892));
#67889=CARTESIAN_POINT('Ctrl Pts',(-5.35069213975294,6.37498668367476,52.5707705279956));
#67890=CARTESIAN_POINT('Ctrl Pts',(-7.65011851213803,1.73006062568215,52.7826392876008));
#67891=CARTESIAN_POINT('Ctrl Pts',(-7.57311345441759,-3.45229115196891,
52.9945080472057));
#67892=CARTESIAN_POINT('Ctrl Pts',(-2.60617526250377,-8.53490840971108,
53.2593439967123));
#67893=CARTESIAN_POINT('Ctrl Pts',(5.77071660837816,-6.80609187443695,53.5771471361199));
#67894=CARTESIAN_POINT('Ctrl Pts',(8.84113534714055,1.15971806681325,53.8949502755276));
#67895=CARTESIAN_POINT('Ctrl Pts',(3.82014222720046,8.06415340512867,54.2127534149352));
#67896=CARTESIAN_POINT('Ctrl Pts',(-4.71923049680223,7.57401310925028,54.530556554343));
#67897=CARTESIAN_POINT('Ctrl Pts',(-8.20728501981211,1.38232926432565,54.7953925038493));
#67898=CARTESIAN_POINT('Ctrl Pts',(-6.94511342020426,-3.64456068666602,
55.0072612634544));
#67899=CARTESIAN_POINT('Ctrl Pts',(-3.52551304465861,-7.53930496553799,
55.2191300230596));
#67900=CARTESIAN_POINT('Ctrl Pts',(3.55150827964952,-8.18679424442952,55.4839659725659));
#67901=CARTESIAN_POINT('Ctrl Pts',(8.80658877899636,-1.43807192279932,55.8017691119736));
#67902=CARTESIAN_POINT('Ctrl Pts',(5.97753752336905,6.6166203894183,56.1195722513813));
#67903=CARTESIAN_POINT('Ctrl Pts',(-2.32215931151299,8.61577813719931,56.4373753907889));
#67904=CARTESIAN_POINT('Ctrl Pts',(-8.50425315695961,2.70453125391184,56.7551785301966));
#67905=CARTESIAN_POINT('Ctrl Pts',(-7.14369631700244,-4.27059299417418,
57.020014479703));
#67906=CARTESIAN_POINT('Ctrl Pts',(-2.92279868749432,-7.278370068269,57.2318832393081));
#67907=CARTESIAN_POINT('Ctrl Pts',(2.20603659733405,-8.02519558158345,57.4437519989132));
#67908=CARTESIAN_POINT('Ctrl Pts',(8.0128260545997,-3.92828584496743,57.7085879484197));
#67909=CARTESIAN_POINT('Ctrl Pts',(7.63602397855986,4.61683815791143,58.0263910878273));
#67910=CARTESIAN_POINT('Ctrl Pts',(0.25878937236362,8.91311664243787,58.3441942272349));
#67911=CARTESIAN_POINT('Ctrl Pts',(-7.3552894075989,5.0521059478154,58.6619973666427));
#67912=CARTESIAN_POINT('Ctrl Pts',(-8.22724842054307,-3.45676069286183,
58.9798005060503));
#67913=CARTESIAN_POINT('Ctrl Pts',(-2.66794553283229,-7.88368113417099,
59.2446364555568));
#67914=CARTESIAN_POINT('Ctrl Pts',(2.49558082881807,-7.43569091242558,59.4565052151618));
#67915=CARTESIAN_POINT('Ctrl Pts',(6.88388041345025,-4.67787901134262,59.668373974767));
#67916=CARTESIAN_POINT('Ctrl Pts',(8.64684490546638,2.20655483545132,59.9332099242733));
#67917=CARTESIAN_POINT('Ctrl Pts',(2.81813847525576,8.4665313034189,60.2510130636811));
#67918=CARTESIAN_POINT('Ctrl Pts',(-5.58356863609584,6.95229325524742,60.5688162030886));
#67919=CARTESIAN_POINT('Ctrl Pts',(-8.87519070722709,-0.92468734599234,
60.8866193424964));
#67920=CARTESIAN_POINT('Ctrl Pts',(-4.02052665126542,-7.96694273278701,
61.204422481904));
#67921=CARTESIAN_POINT('Ctrl Pts',(3.08214029839192,-7.73115597905461,61.4692584314104));
#67922=CARTESIAN_POINT('Ctrl Pts',(6.72195470866535,-4.04137945668859,61.6811271910155));
#67923=CARTESIAN_POINT('Ctrl Pts',(8.27366232476659,0.903810448701441,61.8929959506206));
#67924=CARTESIAN_POINT('Ctrl Pts',(5.15072789940744,7.28744215533195,62.1578319001271));
#67925=CARTESIAN_POINT('Ctrl Pts',(-3.3458212196969,8.27221476651291,62.4756350395347));
#67926=CARTESIAN_POINT('Ctrl Pts',(-8.75895420713288,1.67073080366058,62.7934381789424));
#67927=CARTESIAN_POINT('Ctrl Pts',(-6.15588755971667,-6.45980689569075,
63.11124131835));
#67928=CARTESIAN_POINT('Ctrl Pts',(2.10658590420723,-8.67174186015929,63.4290444577578));
#67929=CARTESIAN_POINT('Ctrl Pts',(7.36005237125288,-3.88587064682533,63.693880407264));
#67930=CARTESIAN_POINT('Ctrl Pts',(7.73760994206874,1.28328305634092,63.9057491668694));
#67931=CARTESIAN_POINT('Ctrl Pts',(5.71155776081948,6.05379794313175,64.1176179264742));
#67932=CARTESIAN_POINT('Ctrl Pts',(-0.805616648510092,8.88750768644881,
64.3824538759809));
#67933=CARTESIAN_POINT('Ctrl Pts',(-7.9116608672323,4.1267031755862,64.7002570153883));
#67934=CARTESIAN_POINT('Ctrl Pts',(-7.75065529723538,-4.40885049467406,
65.0180601547962));
#67935=CARTESIAN_POINT('Ctrl Pts',(-0.496245800892245,-8.90942180405585,
65.3358632942037));
#67936=CARTESIAN_POINT('Ctrl Pts',(7.22749491679466,-5.23451318545963,65.6536664336115));
#67937=CARTESIAN_POINT('Ctrl Pts',(8.12246063437796,1.81548749222381,65.9185023831178));
#67938=CARTESIAN_POINT('Ctrl Pts',(5.05742228502824,5.99498981226798,66.1303711427229));
#67939=CARTESIAN_POINT('Ctrl Pts',(0.42134719233992,8.31220958199092,66.3422399023281));
#67940=CARTESIAN_POINT('Ctrl Pts',(-6.37716116319796,6.2424856074841,66.6070758518344));
#67941=CARTESIAN_POINT('Ctrl Pts',(-8.69852279597928,-1.98991405476493,
66.9248789912421));
#67942=CARTESIAN_POINT('Ctrl Pts',(-3.04028242767115,-8.38255945286813,
67.2426821306498));
#67943=CARTESIAN_POINT('Ctrl Pts',(5.4004260652692,-7.10348189911743,67.5604852700574));
#67944=CARTESIAN_POINT('Ctrl Pts',(8.89621573381947,0.702962786061858,67.8782884094652));
#67945=CARTESIAN_POINT('Ctrl Pts',(5.00520339182766,6.64968424794669,68.1431243589715));
#67946=CARTESIAN_POINT('Ctrl Pts',(-0.0384258066755255,7.84321021496693,
68.3549931185767));
#67947=CARTESIAN_POINT('Ctrl Pts',(-5.07011841966402,6.60032278010828,68.5668618781817));
#67948=CARTESIAN_POINT('Ctrl Pts',(-8.90267648752489,0.615761656414104,
68.8316978276883));
#67949=CARTESIAN_POINT('Ctrl Pts',(-5.33056510057982,-7.1560556518278,69.1495009670957));
#67950=CARTESIAN_POINT('Ctrl Pts',(3.12227093202969,-8.35236759500319,69.4673041065036));
#67951=CARTESIAN_POINT('Ctrl Pts',(8.71760291505868,-1.90458819272834,69.7851072459112));
#67952=CARTESIAN_POINT('Ctrl Pts',(6.31568957316768,6.30467099204083,70.1029103853189));
#67953=CARTESIAN_POINT('Ctrl Pts',(-0.502772112368008,8.30768209207719,
70.3677463348252));
#67954=CARTESIAN_POINT('Ctrl Pts',(-5.11591994012307,5.94514812280067,70.5796150944303));
#67955=CARTESIAN_POINT('Ctrl Pts',(-8.1398593397655,1.73581439547418,70.7914838540355));
#67956=CARTESIAN_POINT('Ctrl Pts',(-7.17585885886399,-5.30507871892191,
71.0563198035419));
#67957=CARTESIAN_POINT('Ctrl Pts',(0.583518731386589,-8.90413181077787,
71.3741229429495));
#67958=CARTESIAN_POINT('Ctrl Pts',(7.79348232585873,-4.3326958910605,71.6919260823573));
#67959=CARTESIAN_POINT('Ctrl Pts',(7.87084648811618,4.20402541266067,72.0097292217649));
#67960=CARTESIAN_POINT('Ctrl Pts',(0.718496112866162,8.89497494527636,72.3275323611726));
#67961=CARTESIAN_POINT('Ctrl Pts',(-5.7706005815723,5.99754358919117,72.5923683106789));
#67962=CARTESIAN_POINT('Ctrl Pts',(-7.74981197678148,1.20740698561282,72.8042370702841));
#67963=CARTESIAN_POINT('Ctrl Pts',(-7.32162543595896,-3.95780124157864,
73.0161058298892));
#67964=CARTESIAN_POINT('Ctrl Pts',(-2.02151445560857,-8.69196333085375,
73.2809417793956));
#67965=CARTESIAN_POINT('Ctrl Pts',(6.21888287064807,-6.3991850739513,73.5987449188032));
#67966=CARTESIAN_POINT('Ctrl Pts',(8.74217083367641,1.75648262129356,73.916548058211));
#67967=CARTESIAN_POINT('Ctrl Pts',(3.26459345311881,8.30458278096055,74.2343511976185));
#67968=CARTESIAN_POINT('Ctrl Pts',(-5.22185729667213,7.23666008718191,74.5521543370264));
#67969=CARTESIAN_POINT('Ctrl Pts',(-8.28216907153752,0.822636887797858,
74.8169902865326));
#67970=CARTESIAN_POINT('Ctrl Pts',(-6.68196928121076,-4.10696513615418,
75.0288590461378));
#67971=CARTESIAN_POINT('Ctrl Pts',(-3.00639701191772,-7.76118831963662,
75.2407278057428));
#67972=CARTESIAN_POINT('Ctrl Pts',(4.09872809405852,-7.92673324829183,75.5055637552494));
#67973=CARTESIAN_POINT('Ctrl Pts',(8.88326754126994,-0.838407728998665,
75.8233668946569));
#67974=CARTESIAN_POINT('Ctrl Pts',(5.51619802321942,7.00799436149701,76.1411700340646));
#67975=CARTESIAN_POINT('Ctrl Pts',(-2.90287476372161,8.43601988074216,76.4589731734724));
#67976=CARTESIAN_POINT('Ctrl Pts',(-8.66435079961945,2.12653204614075,76.77677631288));
#67977=CARTESIAN_POINT('Ctrl Pts',(-6.47933415350991,-6.12851160799295,
77.0945794522877));
#67978=CARTESIAN_POINT('Ctrl Pts',(1.63988578694652,-8.77075506074561,77.4123825916953));
#67979=CARTESIAN_POINT('Ctrl Pts',(8.26551738858123,-3.36361327706695,77.7301857311031));
#67980=CARTESIAN_POINT('Ctrl Pts',(7.45684676779562,3.69728324689203,77.9950216806093));
#67981=CARTESIAN_POINT('Ctrl Pts',(3.48460647847746,7.02662036791392,78.2068904402145));
#67982=CARTESIAN_POINT('Ctrl Pts',(-1.56971333319493,8.17355834568325,78.4187591998196));
#67983=CARTESIAN_POINT('Ctrl Pts',(-7.68005149993975,4.54465089995841,78.683595149326));
#67984=CARTESIAN_POINT('Ctrl Pts',(-7.97461028152683,-4.00365538448797,
79.0013982887337));
#67985=CARTESIAN_POINT('Ctrl Pts',(-0.957114982245634,-8.86536592560338,
79.3192014281413));
#67986=CARTESIAN_POINT('Ctrl Pts',(6.9363636744491,-5.61345996202913,79.6370045675491));
#67987=CARTESIAN_POINT('Ctrl Pts',(8.4730346335444,2.800791198554,79.9548077069567));
#67988=CARTESIAN_POINT('Ctrl Pts',(3.27809593601825,7.65012919672485,80.2196436564631));
#67989=CARTESIAN_POINT('Ctrl Pts',(-1.90466288199341,7.60852657288711,80.4315124160682));
#67990=CARTESIAN_POINT('Ctrl Pts',(-6.49575484723515,5.20341514208813,80.6433811756733));
#67991=CARTESIAN_POINT('Ctrl Pts',(-8.79327968646819,-1.52152827671527,
80.9082171251798));
#67992=CARTESIAN_POINT('Ctrl Pts',(-3.47354142326441,-8.21940168690237,
81.2260202645873));
#67993=CARTESIAN_POINT('Ctrl Pts',(5.02105235293711,-7.36882987433891,81.5438234039952));
#67994=CARTESIAN_POINT('Ctrl Pts',(8.92037652050399,0.225699237984256,81.8616265434027));
#67995=CARTESIAN_POINT('Ctrl Pts',(4.6330392710093,7.62704121462448,82.1794296828104));
#67996=CARTESIAN_POINT('Ctrl Pts',(-2.46623939907536,7.94908956504783,82.4442656323168));
#67997=CARTESIAN_POINT('Ctrl Pts',(-6.38425326485288,4.55617529140441,82.656134391922));
#67998=CARTESIAN_POINT('Ctrl Pts',(-8.31906383227824,-0.252068432127678,
82.8680031515269));
#67999=CARTESIAN_POINT('Ctrl Pts',(-5.70646083775828,-6.86098504659725,
83.1328391010336));
#68000=CARTESIAN_POINT('Ctrl Pts',(2.68666917777219,-8.50916361916542,83.4506422404409));
#68001=CARTESIAN_POINT('Ctrl Pts',(8.60092246953097,-2.35260555303574,83.7684453798489));
#68002=CARTESIAN_POINT('Ctrl Pts',(6.64360685990785,5.95705839106529,84.0862485192562));
#68003=CARTESIAN_POINT('Ctrl Pts',(-1.41991428712019,8.81025847953791,84.4040516586642));
#68004=CARTESIAN_POINT('Ctrl Pts',(-7.03258258710037,4.45119576593135,84.6688876081705));
#68005=CARTESIAN_POINT('Ctrl Pts',(-7.81442749145392,-0.672418024438525,
84.8807563677757));
#68006=CARTESIAN_POINT('Ctrl Pts',(-6.16880005396275,-5.58715200125982,
85.0926251273807));
#68007=CARTESIAN_POINT('Ctrl Pts',(0.106029250967578,-8.92331602372033,
85.3574610768872));
#68008=CARTESIAN_POINT('Ctrl Pts',(7.5636015661477,-4.73455257929366,85.6752642162948));
#68009=CARTESIAN_POINT('Ctrl Pts',(8.07259136044653,3.78733269572646,85.9930673557024));
#68010=CARTESIAN_POINT('Ctrl Pts',(1.19354116897602,8.84304903613462,86.3108704951103));
#68011=CARTESIAN_POINT('Ctrl Pts',(-6.79465066921202,5.78528593454319,86.6286736345177));
#68012=CARTESIAN_POINT('Ctrl Pts',(-8.23983677665961,-1.17279643819476,
86.8935095840243));
#68013=CARTESIAN_POINT('Ctrl Pts',(-5.51206719219005,-5.57983317735208,
87.1053783436294));
#68014=CARTESIAN_POINT('Ctrl Pts',(-1.07203005270189,-8.25355154812431,
87.3172471032343));
#68015=CARTESIAN_POINT('Ctrl Pts',(5.86787482937588,-6.72345566266486,87.582083052741));
#68016=CARTESIAN_POINT('Ctrl Pts',(8.82780556978323,1.30150128681965,87.8998861921484));
#68017=CARTESIAN_POINT('Ctrl Pts',(3.6884146331611,8.11826445213714,88.2176893315562));
#68018=CARTESIAN_POINT('Ctrl Pts',(-4.82661537364263,7.50518759341862,88.5354924709639));
#68019=CARTESIAN_POINT('Ctrl Pts',(-8.923945428409,-0.00300862480821861,
88.8532956103715));
#68020=CARTESIAN_POINT('Ctrl Pts',(-5.51136114809949,-6.23660643993697,
89.1181315598778));
#68021=CARTESIAN_POINT('Ctrl Pts',(-0.576886875348588,-7.82206012194633,
89.3300003194832));
#68022=CARTESIAN_POINT('Ctrl Pts',(4.53679143195664,-6.9776704632971,89.5418690790879));
#68023=CARTESIAN_POINT('Ctrl Pts',(8.82695009077069,-1.31215972963913,89.8067050285948));
#68024=CARTESIAN_POINT('Ctrl Pts',(5.87543847491016,6.71589752043862,90.1245081680019));
#68025=CARTESIAN_POINT('Ctrl Pts',(-2.45752071223338,8.57153499496415,90.4423113074101));
#68026=CARTESIAN_POINT('Ctrl Pts',(-8.54135561236971,2.58249899913411,90.7601144468174));
#68027=CARTESIAN_POINT('Ctrl Pts',(-6.79074821486224,-5.78986612482438,
91.0779175862253));
#68028=CARTESIAN_POINT('Ctrl Pts',(-0.150402741474938,-8.32152273365876,
91.3427535357315));
#68029=CARTESIAN_POINT('Ctrl Pts',(4.63384148188355,-6.32810683688797,91.5546222953368));
#68030=CARTESIAN_POINT('Ctrl Pts',(7.97863002593425,-2.36892897755592,91.7664910549419));
#68031=CARTESIAN_POINT('Ctrl Pts',(7.56986287027127,4.72588480459817,92.0313270044481));
#68032=CARTESIAN_POINT('Ctrl Pts',(0.11668831364906,8.92246830282663,92.349130143856));
#68033=CARTESIAN_POINT('Ctrl Pts',(-7.42962970550756,4.93064120170904,92.6669332832636));
#68034=CARTESIAN_POINT('Ctrl Pts',(-8.1763465937579,-3.57371139800513,92.9847364226712));
#68035=CARTESIAN_POINT('Ctrl Pts',(-1.41397337222863,-8.81121389841784,
93.3025395620791));
#68036=CARTESIAN_POINT('Ctrl Pts',(5.28239501954281,-6.43169219171388,93.5673755115852));
#68037=CARTESIAN_POINT('Ctrl Pts',(7.63123132444705,-1.81155499256043,93.7792442711905));
#68038=CARTESIAN_POINT('Ctrl Pts',(7.60950331181201,3.37132332162994,93.9911130307955));
#68039=CARTESIAN_POINT('Ctrl Pts',(2.69705657370164,8.5066266462856,94.2559489803021));
#68040=CARTESIAN_POINT('Ctrl Pts',(-5.69779762101329,6.86725265644592,94.5737521197095));
#68041=CARTESIAN_POINT('Ctrl Pts',(-8.85300151361534,-1.06535647596267,
94.8915552591175));
#68042=CARTESIAN_POINT('Ctrl Pts',(-3.90593362552959,-8.02295078449604,
95.2093583985248));
#68043=CARTESIAN_POINT('Ctrl Pts',(4.63818100932635,-7.62391552850421,95.5271615379327));
#68044=CARTESIAN_POINT('Ctrl Pts',(8.19207488967919,-1.46978590050783,95.791997487439));
#68045=CARTESIAN_POINT('Ctrl Pts',(6.98358965896691,3.57027989007352,96.0038662470443));
#68046=CARTESIAN_POINT('Ctrl Pts',(3.60572340047096,7.50127458174534,96.2157350066492));
#68047=CARTESIAN_POINT('Ctrl Pts',(-3.46398955889884,8.2242074023509,96.4805709561558));
#68048=CARTESIAN_POINT('Ctrl Pts',(-8.79075003479858,1.53191729645467,96.7983740955633));
#68049=CARTESIAN_POINT('Ctrl Pts',(-6.0477674669237,-6.55249028133353,97.1161772349711));
#68050=CARTESIAN_POINT('Ctrl Pts',(2.23013516258891,-8.64005520434183,97.4339803743786));
#68051=CARTESIAN_POINT('Ctrl Pts',(8.47492411579095,-2.79508001542504,97.7517835137864));
#68052=CARTESIAN_POINT('Ctrl Pts',(7.1888382435156,4.19415859261561,98.0166194632927));
#68053=CARTESIAN_POINT('Ctrl Pts',(3.00026030903199,7.24678281007098,98.2284882228979));
#68054=CARTESIAN_POINT('Ctrl Pts',(-2.12031794486745,8.04826772691589,98.440356982503));
#68055=CARTESIAN_POINT('Ctrl Pts',(-7.97047294154431,4.01352365748019,98.7051929320094));
#68056=CARTESIAN_POINT('Ctrl Pts',(-7.68483079945345,-4.53513311395154,
99.022996071417));
#68057=CARTESIAN_POINT('Ctrl Pts',(-0.353838000969954,-8.90984954362422,
99.3407992108247));
#68058=CARTESIAN_POINT('Ctrl Pts',(7.3009875276655,-5.13026684475196,99.6586023502325));
#68059=CARTESIAN_POINT('Ctrl Pts',(8.26364874175473,3.36881589493082,99.97640548964));
#68060=CARTESIAN_POINT('Ctrl Pts',(2.75187762938652,7.85477759738149,100.241241439146));
#68061=CARTESIAN_POINT('Ctrl Pts',(-2.41613310275605,7.46188473832575,100.453110198751));
#68062=CARTESIAN_POINT('Ctrl Pts',(-6.83359668512604,4.75103335459544,100.664978958356));
#68063=CARTESIAN_POINT('Ctrl Pts',(-8.66988721951361,-2.11420591758654,
100.929814907864));
#68064=CARTESIAN_POINT('Ctrl Pts',(-2.90827845038575,-8.43599272359275,
101.247618047271));
#68065=CARTESIAN_POINT('Ctrl Pts',(5.50910097438566,-7.0114496842646,101.565421186678));
#68066=CARTESIAN_POINT('Ctrl Pts',(8.88454820327112,0.829975904011698,101.883224326085));
#68067=CARTESIAN_POINT('Ctrl Pts',(4.10526984608823,7.92360842999213,102.201027465493));
#68068=CARTESIAN_POINT('Ctrl Pts',(-2.99950791027979,7.76358898239801,102.465863415));
#68069=CARTESIAN_POINT('Ctrl Pts',(-6.67846881235397,4.11284297544998,102.677732174605));
#68070=CARTESIAN_POINT('Ctrl Pts',(-8.28283137121611,-0.815515829056787,
102.88960093421));
#68071=CARTESIAN_POINT('Ctrl Pts',(-5.22815955816402,-7.23209227647307,
103.154436883716));
#68072=CARTESIAN_POINT('Ctrl Pts',(3.25740314075584,-8.30742929889158,103.472240023124));
#68073=CARTESIAN_POINT('Ctrl Pts',(8.74063673591143,-1.76405489477698,103.790043162533));
#68074=CARTESIAN_POINT('Ctrl Pts',(6.22443485579875,6.39378350457737,104.107846301939));
#68075=CARTESIAN_POINT('Ctrl Pts',(-2.01397713256718,8.69371653382717,104.425649441348));
#68076=CARTESIAN_POINT('Ctrl Pts',(-7.31818876878027,3.9641486773256,104.690485390853));
#68077=CARTESIAN_POINT('Ctrl Pts',(-7.75085676495864,-1.20068414971929,
104.902354150459));
#68078=CARTESIAN_POINT('Ctrl Pts',(-5.77580001840686,-5.99253666979313,
105.114222910065));
#68079=CARTESIAN_POINT('Ctrl Pts',(0.710780611675296,-8.89559452668069,
105.37905885957));
#68080=CARTESIAN_POINT('Ctrl Pts',(7.86719727708827,-4.21085071937526,105.696861998978));
#68081=CARTESIAN_POINT('Ctrl Pts',(7.79723729390108,4.32593467398078,106.014665138385));
#68082=CARTESIAN_POINT('Ctrl Pts',(0.591241515787013,8.90362231046995,106.332468277793));
#68083=CARTESIAN_POINT('Ctrl Pts',(-7.17125483096129,5.31130070796763,106.650271417201));
#68084=CARTESIAN_POINT('Ctrl Pts',(-8.141361823899,-1.728753667763,106.915107366707));
#68085=CARTESIAN_POINT('Ctrl Pts',(-5.12107452753105,-5.94070860266393,
107.126976126312));
#68086=CARTESIAN_POINT('Ctrl Pts',(-0.509977566734008,-8.3072428923724,
107.338844885917));
#68087=CARTESIAN_POINT('Ctrl Pts',(6.31021885650242,-6.31014651526292,107.603680835425));
#68088=CARTESIAN_POINT('Ctrl Pts',(8.71925157619185,1.89702628568087,107.921483974831));
#68089=CARTESIAN_POINT('Ctrl Pts',(3.12951416104503,8.3496563604001,108.239287114239));
#68090=CARTESIAN_POINT('Ctrl Pts',(-5.32435630946186,7.16067641130234,108.557090253647));
#68091=CARTESIAN_POINT('Ctrl Pts',(-8.90320721817968,-0.608039711858129,
108.874893393056));
#68092=CARTESIAN_POINT('Ctrl Pts',(-5.07584128491461,-6.59592274377136,
109.139729342561));
#68093=CARTESIAN_POINT('Ctrl Pts',(-0.0452285797699074,-7.84317393622409,
109.351598102166));
#68094=CARTESIAN_POINT('Ctrl Pts',(4.99943392320907,-6.65402299657202,109.563466861771));
#68095=CARTESIAN_POINT('Ctrl Pts',(8.89560267463199,-0.710678630693007,
109.828302811278));
#68096=CARTESIAN_POINT('Ctrl Pts',(5.40658522006346,7.09879518197837,110.146105950685));
#68097=CARTESIAN_POINT('Ctrl Pts',(-3.0330106934329,8.38519328068666,110.463909090093));
#68098=CARTESIAN_POINT('Ctrl Pts',(-8.6967935774011,1.99745794688234,110.7817122295));
#68099=CARTESIAN_POINT('Ctrl Pts',(-6.38257316774903,-6.23695204562081,
111.099515368908));
#68100=CARTESIAN_POINT('Ctrl Pts',(0.414137460974179,-8.31257190975582,
111.364351318415));
#68101=CARTESIAN_POINT('Ctrl Pts',(5.05222064422742,-5.99937409904855,111.57622007802));
#68102=CARTESIAN_POINT('Ctrl Pts',(8.1208829209,-1.8225318039691,111.788088837625));
#68103=CARTESIAN_POINT('Ctrl Pts',(7.23203233929537,5.22824246802203,112.052924787131));
#68104=CARTESIAN_POINT('Ctrl Pts',(-0.488518050920525,8.90984887029028,
112.370727926539));
#68105=CARTESIAN_POINT('Ctrl Pts',(-7.74682837710603,4.41557134656612,112.688531065946));
#68106=CARTESIAN_POINT('Ctrl Pts',(-7.91523717632062,-4.11983946532877,
113.006334205354));
#68107=CARTESIAN_POINT('Ctrl Pts',(-0.813324901639997,-8.88680559399253,
113.324137344762));
#68108=CARTESIAN_POINT('Ctrl Pts',(5.7063048668929,-6.05874957045746,113.588973294268));
#68109=CARTESIAN_POINT('Ctrl Pts',(7.7364939794529,-1.28999376904755,113.800842053873));
#68110=CARTESIAN_POINT('Ctrl Pts',(7.36342000237286,3.87948546331845,114.012710813478));
#68111=CARTESIAN_POINT('Ctrl Pts',(2.11410652406723,8.66991145663782,114.277546762985));
#68112=CARTESIAN_POINT('Ctrl Pts',(-6.15028234787188,6.46514375856746,114.595349902392));
#68113=CARTESIAN_POINT('Ctrl Pts',(-8.76040001640918,-1.66313311958161,
114.9131530418));
#68114=CARTESIAN_POINT('Ctrl Pts',(-3.35299484466143,-8.26930966581624,
115.230956181208));
#68115=CARTESIAN_POINT('Ctrl Pts',(5.14440521840749,-7.29190688433863,115.548759320616));
#68116=CARTESIAN_POINT('Ctrl Pts',(8.27287529507401,-0.910986247753953,
115.813595270122));
#68117=CARTESIAN_POINT('Ctrl Pts',(6.72545745995588,4.03554766699847,116.025464029727));
#68118=CARTESIAN_POINT('Ctrl Pts',(3.08884473663849,7.72847978482084,116.237332789332));
#68119=CARTESIAN_POINT('Ctrl Pts',(-4.01361503236695,7.97042692915515,116.50216873884));
#68120=CARTESIAN_POINT('Ctrl Pts',(-8.87438534375087,0.932384871234997,
116.819971878246));
#68121=CARTESIAN_POINT('Ctrl Pts',(-5.58959658892818,-6.94744774676236,
117.137775017654));
#68122=CARTESIAN_POINT('Ctrl Pts',(2.81079399181202,-8.46897242368175,117.455578157061));
#68123=CARTESIAN_POINT('Ctrl Pts',(8.64492780352305,-2.21405382340118,117.773381296471));
#68124=CARTESIAN_POINT('Ctrl Pts',(6.88793517002941,4.6719065364063,118.038217245975));
#68125=CARTESIAN_POINT('Ctrl Pts',(2.50202921685677,7.43352358012588,118.250086005581));
#68126=CARTESIAN_POINT('Ctrl Pts',(-2.66110663942737,7.88599220422133,118.461954765186));
#68127=CARTESIAN_POINT('Ctrl Pts',(-8.22424711370316,3.46389527465665,118.726790714692));
#68128=CARTESIAN_POINT('Ctrl Pts',(-7.35966857159775,-5.04572445677769,
119.0445938541));
#68129=CARTESIAN_POINT('Ctrl Pts',(0.251058507001858,-8.91333775008066,
119.362396993508));
#68130=CARTESIAN_POINT('Ctrl Pts',(7.63201670400195,-4.62345950640031,119.680200132915));
#68131=CARTESIAN_POINT('Ctrl Pts',(8.01623022889107,3.92133446398752,119.998003272323));
#68132=CARTESIAN_POINT('Ctrl Pts',(2.21299639959071,8.02327916296338,120.262839221829));
#68133=CARTESIAN_POINT('Ctrl Pts',(-2.91648471317105,7.28090241221048,120.474707981436));
#68134=CARTESIAN_POINT('Ctrl Pts',(-7.13998954245359,4.27678745381348,120.686576741039));
#68135=CARTESIAN_POINT('Ctrl Pts',(-8.50659572611224,-2.6971540952516,120.951412690547));
#68136=CARTESIAN_POINT('Ctrl Pts',(-2.32963131029981,-8.61376077770682,
121.269215829955));
#68137=CARTESIAN_POINT('Ctrl Pts',(5.97179636684307,-6.62180250188054,121.587018969362));
#68138=CARTESIAN_POINT('Ctrl Pts',(8.80783277429343,1.43043301051482,121.904822108769));
#68139=CARTESIAN_POINT('Ctrl Pts',(3.55860773798312,8.1837107737389,122.222625248177));
#68140=CARTESIAN_POINT('Ctrl Pts',(-3.51897252243771,7.54235997402486,122.487461197683));
#68141=CARTESIAN_POINT('Ctrl Pts',(-6.94194970780889,3.65058314143714,122.699329957288));
#68142=CARTESIAN_POINT('Ctrl Pts',(-8.20848089228814,-1.37521017753044,
122.911198716893));
#68143=CARTESIAN_POINT('Ctrl Pts',(-4.72579802181384,-7.56991704829477,
123.1760346664));
#68144=CARTESIAN_POINT('Ctrl Pts',(3.81314636825754,-8.06746376203405,123.493837805807));
#68145=CARTESIAN_POINT('Ctrl Pts',(8.84012614320339,-1.16738596582406,123.811640945215));
#68146=CARTESIAN_POINT('Ctrl Pts',(5.77661768343671,6.80108409864888,124.129444084624));
#68147=CARTESIAN_POINT('Ctrl Pts',(-2.59877155208799,8.53716565852516,124.44724722403));
#68148=CARTESIAN_POINT('Ctrl Pts',(-7.57011627027233,3.45885837322116,124.712083173537));
#68149=CARTESIAN_POINT('Ctrl Pts',(-7.65161619806151,-1.72342466497812,
124.923951933143));
#68150=CARTESIAN_POINT('Ctrl Pts',(-5.35621945486108,-6.37034337715102,
125.135820692747));
#68151=CARTESIAN_POINT('Ctrl Pts',(1.31226092353452,-8.82693504732008,125.400656642255));
#68152=CARTESIAN_POINT('Ctrl Pts',(8.13458774259943,-3.66777030843524,125.718459781661));
#68153=CARTESIAN_POINT('Ctrl Pts',(7.48599994134832,4.84462847895318,126.036262921069));
#68154=CARTESIAN_POINT('Ctrl Pts',(-0.0137790611847593,8.92322065820189,
126.354066060476));
#68155=CARTESIAN_POINT('Ctrl Pts',(-7.51485651011302,4.81287260307762,126.671869199884));
#68156=CARTESIAN_POINT('Ctrl Pts',(-8.00541990639399,-2.27675508427092,
126.93670514939));
#68157=CARTESIAN_POINT('Ctrl Pts',(-4.70651441519925,-6.27424458224373,
127.148573908996));
#68158=CARTESIAN_POINT('Ctrl Pts',(0.0544218621563285,-8.32270387869009,
127.360442668602));
#68159=CARTESIAN_POINT('Ctrl Pts',(6.72352293275359,-5.86779774990415,127.625278618107));
#68160=CARTESIAN_POINT('Ctrl Pts',(8.57057113957244,2.4838210722627,127.943081757516));
#68161=CARTESIAN_POINT('Ctrl Pts',(2.55621150422421,8.54262272177712,128.260884896923));
#68162=CARTESIAN_POINT('Ctrl Pts',(-5.79759428441931,6.78321142901773,128.578688036331));
#68163=CARTESIAN_POINT('Ctrl Pts',(-8.84149599162147,-1.21027256896321,
128.896491175739));
#68164=CARTESIAN_POINT('Ctrl Pts',(-4.61696213975944,-6.9248842727855,129.161327125244));
#68165=CARTESIAN_POINT('Ctrl Pts',(0.486637860052813,-7.82819306171326,
129.373195884849));
#68166=CARTESIAN_POINT('Ctrl Pts',(5.43906876308912,-6.29975337468319,129.585064644454));
#68167=CARTESIAN_POINT('Ctrl Pts',(8.92331723866387,-0.105926952232459,
129.849900593961));
#68168=CARTESIAN_POINT('Ctrl Pts',(4.9128505826903,7.44902382394148,130.167703733368));
#68169=CARTESIAN_POINT('Ctrl Pts',(-3.59454260383601,8.16026247679319,130.485506872776));
#68170=CARTESIAN_POINT('Ctrl Pts',(-8.81220845226687,1.40322449069441,130.803310012184));
#68171=CARTESIAN_POINT('Ctrl Pts',(-5.94502519150861,-6.6553351931643,131.121113151591));
#68172=CARTESIAN_POINT('Ctrl Pts',(0.976771781583879,-8.26536620351122,
131.385949101099));
#68173=CARTESIAN_POINT('Ctrl Pts',(5.44734922800118,-5.64303193385323,131.597817860703));
#68174=CARTESIAN_POINT('Ctrl Pts',(8.22576309608399,-1.26774724552918,131.809686620308));
#68175=CARTESIAN_POINT('Ctrl Pts',(6.86091962450978,5.70653949141333,132.074522569815));
#68176=CARTESIAN_POINT('Ctrl Pts',(-1.0914762303603,8.8562258562012,132.392325709222));
#68177=CARTESIAN_POINT('Ctrl Pts',(-8.02837574712145,3.88018080557894,132.71012884863));
#68178=CARTESIAN_POINT('Ctrl Pts',(-7.6177014313671,-4.64700782009627,133.027931988037));
#68179=CARTESIAN_POINT('Ctrl Pts',(-0.208933468132588,-8.92149975435394,
133.345735127445));
#68180=CARTESIAN_POINT('Ctrl Pts',(6.10395400652709,-5.65792427288009,133.610571076951));
#68181=CARTESIAN_POINT('Ctrl Pts',(7.80615289230366,-0.762495928036403,
133.822439836557));
#68182=CARTESIAN_POINT('Ctrl Pts',(7.08344985635885,4.36979401389729,134.034308596162));
#68183=CARTESIAN_POINT('Ctrl Pts',(1.52142724776122,8.79329688972305,134.299144545668));
#68184=CARTESIAN_POINT('Ctrl Pts',(-6.57446315987215,6.03328193746754,134.616947685076));
#68185=CARTESIAN_POINT('Ctrl Pts',(-8.62748270894221,-2.25325593926971,
134.934750824484));
#68186=CARTESIAN_POINT('Ctrl Pts',(-2.78462540951867,-8.4776127598606,135.252553963892));
#68187=CARTESIAN_POINT('Ctrl Pts',(5.62695461077901,-6.92634051063592,135.5703571033));
#68188=CARTESIAN_POINT('Ctrl Pts',(8.31560350398447,-0.347994189556737,
135.835193052805));
#68189=CARTESIAN_POINT('Ctrl Pts',(6.43637436071595,4.48224364654699,136.047061812411));
#68190=CARTESIAN_POINT('Ctrl Pts',(2.55775105087846,7.92011812747601,136.258930572016));
#68191=CARTESIAN_POINT('Ctrl Pts',(-4.54476964356802,7.67996614236977,136.523766521522));
#68192=CARTESIAN_POINT('Ctrl Pts',(-8.91718027611874,0.328561563009237,
136.84156966093));
#68193=CARTESIAN_POINT('Ctrl Pts',(-5.10570210069917,-7.31043270127474,
137.159372800337));
#68194=CARTESIAN_POINT('Ctrl Pts',(3.37851740289849,-8.25891499749212,137.477175939745));
#68195=CARTESIAN_POINT('Ctrl Pts',(8.77514709004157,-1.62283844210692,137.794979079154));
#68196=CARTESIAN_POINT('Ctrl Pts',(6.55533346555773,5.12815412666026,138.05981502866));
#68197=CARTESIAN_POINT('Ctrl Pts',(1.99228365787784,7.58605489334511,138.271683788265));
#68198=CARTESIAN_POINT('Ctrl Pts',(-3.18964878472523,7.68742494087226,138.483552547869));
#68199=CARTESIAN_POINT('Ctrl Pts',(-8.44017287876276,2.89832586809018,138.748388497376));
#68200=CARTESIAN_POINT('Ctrl Pts',(-7.00063677144394,-5.5330951168216,139.066191636784));
#68201=CARTESIAN_POINT('Ctrl Pts',(0.854799630846115,-8.87580631898063,
139.383994776191));
#68202=CARTESIAN_POINT('Ctrl Pts',(7.92792294796447,-4.09537477022881,139.7017979156));
#68203=CARTESIAN_POINT('Ctrl Pts',(7.73192061330253,4.45580685068717,140.019601055006));
#68204=CARTESIAN_POINT('Ctrl Pts',(1.66393084684311,8.15485718626432,140.284437004514));
#68205=CARTESIAN_POINT('Ctrl Pts',(-3.40341451132808,7.06641299970321,140.496305764118));
#68206=CARTESIAN_POINT('Ctrl Pts',(-7.41352380164428,3.78285955778124,140.708174523723));
#68207=CARTESIAN_POINT('Ctrl Pts',(-8.30415644281345,-3.26768983141359,
140.973010473231));
#68208=CARTESIAN_POINT('Ctrl Pts',(-1.74026308741985,-8.75188786285867,
141.290813612637));
#68209=CARTESIAN_POINT('Ctrl Pts',(6.40700924608265,-6.20168144470193,141.608616752046));
#68210=CARTESIAN_POINT('Ctrl Pts',(8.69058324707021,2.02430719092564,141.926419891452));
#68211=CARTESIAN_POINT('Ctrl Pts',(2.99556873452046,8.40615126070251,142.24422303086));
#68212=CARTESIAN_POINT('Ctrl Pts',(-4.02224264253235,7.28642063814767,142.509058980366));
#68213=CARTESIAN_POINT('Ctrl Pts',(-7.17348339460544,3.17152313654336,142.720927739972));
#68214=CARTESIAN_POINT('Ctrl Pts',(-8.09635456321866,-1.92857573822395,
142.932796499578));
#68215=CARTESIAN_POINT('Ctrl Pts',(-4.20168812055101,-7.87290467353922,
143.197632449083));
#68216=CARTESIAN_POINT('Ctrl Pts',(4.35134130057544,-7.79037134311117,143.515435588491));
#68217=CARTESIAN_POINT('Ctrl Pts',(8.89893283649567,-0.565344666760167,
143.8332387279));
#68218=CARTESIAN_POINT('Ctrl Pts',(5.30221622019615,7.17708575479655,144.151041867307));
#68219=CARTESIAN_POINT('Ctrl Pts',(-3.17160629166672,8.3413263089766,144.468845006715));
#68220=CARTESIAN_POINT('Ctrl Pts',(-7.78720570827248,2.93765022536944,144.73368095622));
#68221=CARTESIAN_POINT('Ctrl Pts',(-7.51716250103231,-2.23823389140988,
144.945549715825));
#68222=CARTESIAN_POINT('Ctrl Pts',(-4.91198929433456,-6.71883343777705,
145.15741847543));
#68223=CARTESIAN_POINT('Ctrl Pts',(1.90770214269294,-8.71765355949647,145.422254424937));
#68224=CARTESIAN_POINT('Ctrl Pts',(8.36454241906866,-3.10781063135707,145.740057564344));
#68225=CARTESIAN_POINT('Ctrl Pts',(7.14031163116602,5.34102705691939,146.057860703752));
#68226=CARTESIAN_POINT('Ctrl Pts',(-0.618736222637683,8.90175388337603,
146.37566384316));
#68227=CARTESIAN_POINT('Ctrl Pts',(-7.82387444120206,4.29229541822987,146.693466982568));
#68228=CARTESIAN_POINT('Ctrl Pts',(-7.83263662343708,-2.81427876870812,
146.958302932074));
#68229=CARTESIAN_POINT('Ctrl Pts',(-4.27029469863186,-6.57890615089385,
147.170171691679));
#68230=CARTESIAN_POINT('Ctrl Pts',(0.618570879103147,-8.2998633925873,147.382040451284));
#68231=CARTESIAN_POINT('Ctrl Pts',(7.10588492607867,-5.39844499810615,147.646876400792));
#68232=CARTESIAN_POINT('Ctrl Pts',(8.3824486383776,3.05918505229256,147.964679540198));
#68233=CARTESIAN_POINT('Ctrl Pts',(1.97114476862672,8.69627574122246,148.282482679606));
#68234=CARTESIAN_POINT('Ctrl Pts',(-6.24415093653934,6.37452929401478,148.600285819015));
#68235=CARTESIAN_POINT('Ctrl Pts',(-8.73909673220554,-1.80693476545242,
148.918088958421));
#68236=CARTESIAN_POINT('Ctrl Pts',(-4.13683377657115,-7.22197874387156,
149.182924907929));
#68237=CARTESIAN_POINT('Ctrl Pts',(1.01626246935375,-7.77718428549169,149.394793667533));
#68238=CARTESIAN_POINT('Ctrl Pts',(5.85367832461859,-5.91649721289159,149.606662427138));
#68239=CARTESIAN_POINT('Ctrl Pts',(8.909954357225,0.499323352786752,149.871498376644));
#68240=CARTESIAN_POINT('Ctrl Pts',(4.39652669300149,7.76495297395151,150.189301516052));
#68241=CARTESIAN_POINT('Ctrl Pts',(-4.13956870112755,7.8978119229406,150.50710465546));
#68242=CARTESIAN_POINT('Ctrl Pts',(-8.88700008103003,0.802468590361602,
150.824907794867));
#68243=CARTESIAN_POINT('Ctrl Pts',(-5.4802548365995,-7.04296170243578,151.142710934275));
#68244=CARTESIAN_POINT('Ctrl Pts',(1.53515019871226,-8.18034727796208,151.407546883781));
#68245=CARTESIAN_POINT('Ctrl Pts',(5.817089426409,-5.26042064170382,151.619415643387));
#68246=CARTESIAN_POINT('Ctrl Pts',(8.29356557029805,-0.707857898752759,
151.831284402991));
#68247=CARTESIAN_POINT('Ctrl Pts',(6.45658054965811,6.16012403831793,152.096120352499));
#68248=CARTESIAN_POINT('Ctrl Pts',(-1.68663607804514,8.75924487711618,152.413923491905));
#68249=CARTESIAN_POINT('Ctrl Pts',(-8.27807529560295,3.33170044403166,152.731726631313));
#68250=CARTESIAN_POINT('Ctrl Pts',(-7.27525669696981,-5.1619012277632,153.049529770721));
#68251=CARTESIAN_POINT('Ctrl Pts',(-0.899851274104358,-8.27397708193549,
153.314365720227));
#68252=CARTESIAN_POINT('Ctrl Pts',(4.06460834341926,-6.71766665604379,153.526237920521));
#68253=CARTESIAN_POINT('Ctrl Pts',(5.88183385080656,-4.89010705830048,153.632175741013));
#68254=CARTESIAN_POINT('Ctrl Pts',(6.51518125436024,-3.80590017975039,153.685146371603));
#68255=CARTESIAN_POINT('Ctrl Pts',(4.14970254892029,-5.82589768344819,-0.222854153409353));
#68256=CARTESIAN_POINT('Ctrl Pts',(5.12020403053176,-5.13464909858868,-0.169830221776262));
#68257=CARTESIAN_POINT('Ctrl Pts',(6.69075495720071,-3.26142663595671,-0.0638391002418928));
#68258=CARTESIAN_POINT('Ctrl Pts',(7.73384029383181,1.56021684963465,0.148086401095035));
#68259=CARTESIAN_POINT('Ctrl Pts',(4.24822985914703,7.31166922656103,0.412922350601427));
#68260=CARTESIAN_POINT('Ctrl Pts',(-3.85638135699804,7.5288227374144,0.730725490009101));
#68261=CARTESIAN_POINT('Ctrl Pts',(-8.41413174439718,0.839900777573334,
1.04852862941677));
#68262=CARTESIAN_POINT('Ctrl Pts',(-5.26093362085182,-6.62453301130198,
1.36633176882444));
#68263=CARTESIAN_POINT('Ctrl Pts',(1.38064608400363,-7.76882450453534,1.63116771833084));
#68264=CARTESIAN_POINT('Ctrl Pts',(5.46582045917633,-5.03983377869041,1.84303647793595));
#68265=CARTESIAN_POINT('Ctrl Pts',(7.85460539252143,-0.74661404229422,2.05490523754107));
#68266=CARTESIAN_POINT('Ctrl Pts',(6.17824832881788,5.77865494324373,2.31974118704746));
#68267=CARTESIAN_POINT('Ctrl Pts',(-1.52093803950862,8.32093582721797,2.63754432645514));
#68268=CARTESIAN_POINT('Ctrl Pts',(-7.81158451531416,3.22961110439484,2.9553474658628));
#68269=CARTESIAN_POINT('Ctrl Pts',(-6.95293978484151,-4.81756640596561,
3.27315060527048));
#68270=CARTESIAN_POINT('Ctrl Pts',(0.293939508506351,-8.4544249858399,3.59095374467815));
#68271=CARTESIAN_POINT('Ctrl Pts',(6.08833921177905,-5.01802144693415,3.85578969418455));
#68272=CARTESIAN_POINT('Ctrl Pts',(7.42942471280202,-0.291382842792715,
4.06765845378966));
#68273=CARTESIAN_POINT('Ctrl Pts',(6.46264594464048,4.52576120477877,4.27952721339478));
#68274=CARTESIAN_POINT('Ctrl Pts',(0.955200652235128,8.40544387467254,4.54436316290117));
#68275=CARTESIAN_POINT('Ctrl Pts',(-6.55428925885352,5.34730797572404,4.86216630230884));
#68276=CARTESIAN_POINT('Ctrl Pts',(-8.04049572987898,-2.60785644394081,
5.17996944171652));
#68277=CARTESIAN_POINT('Ctrl Pts',(-2.16803525546429,-8.17631003184262,
5.49777258112419));
#68278=CARTESIAN_POINT('Ctrl Pts',(5.70682637845079,-6.24467880353645,5.81557572053187));
#68279=CARTESIAN_POINT('Ctrl Pts',(7.88870517433334,0.128958167596947,6.08041167003825));
#68280=CARTESIAN_POINT('Ctrl Pts',(5.84408279748823,4.59651890592599,6.29228042964337));
#68281=CARTESIAN_POINT('Ctrl Pts',(1.98405567635904,7.6362177736106,6.50414918924849));
#68282=CARTESIAN_POINT('Ctrl Pts',(-4.7242269156689,7.01751827523279,6.76898513875488));
#68283=CARTESIAN_POINT('Ctrl Pts',(-8.45694035083907,-0.180502158241452,
7.08678827816255));
#68284=CARTESIAN_POINT('Ctrl Pts',(-4.42892672371275,-7.19965915629606,
7.40459141757022));
#68285=CARTESIAN_POINT('Ctrl Pts',(3.65244304644529,-7.62968420039558,7.7223945569779));
#68286=CARTESIAN_POINT('Ctrl Pts',(8.39385575585232,-1.05217302843921,8.04019769638557));
#68287=CARTESIAN_POINT('Ctrl Pts',(5.92106350224164,5.21433657636706,8.30503364589196));
#68288=CARTESIAN_POINT('Ctrl Pts',(1.46733253957555,7.28891110333928,8.51690240549708));
#68289=CARTESIAN_POINT('Ctrl Pts',(-3.44221033706579,7.09925960380392,8.72877116510219));
#68290=CARTESIAN_POINT('Ctrl Pts',(-8.14714462265909,2.27769994544157,8.9936071146086));
#68291=CARTESIAN_POINT('Ctrl Pts',(-6.3201623689668,-5.62209647855652,9.31141025401626));
#68292=CARTESIAN_POINT('Ctrl Pts',(1.29810371260021,-8.35256910472367,9.62921339342394));
#68293=CARTESIAN_POINT('Ctrl Pts',(7.72834457329497,-3.43876596193245,9.9470165328316));
#68294=CARTESIAN_POINT('Ctrl Pts',(7.07158859510588,4.64289966341321,10.2648196722393));
#68295=CARTESIAN_POINT('Ctrl Pts',(1.1252461643865,7.80910494218149,10.5296556217457));
#68296=CARTESIAN_POINT('Ctrl Pts',(-3.61028409669472,6.49977988812623,10.7415243813508));
#68297=CARTESIAN_POINT('Ctrl Pts',(-7.22431635935756,3.17136438593861,10.9533931409559));
#68298=CARTESIAN_POINT('Ctrl Pts',(-7.67860660833376,-3.55005395697526,
11.2182290904623));
#68299=CARTESIAN_POINT('Ctrl Pts',(-1.16458047228838,-8.37831567249255,
11.53603222987));
#68300=CARTESIAN_POINT('Ctrl Pts',(6.40509935429006,-5.51590302305541,11.8538353692777));
#68301=CARTESIAN_POINT('Ctrl Pts',(8.1128287823567,2.39466706089449,12.1716385086853));
#68302=CARTESIAN_POINT('Ctrl Pts',(2.37160135883004,8.12030723173545,12.489441648093));
#68303=CARTESIAN_POINT('Ctrl Pts',(-4.2080411500674,6.67388107534385,12.7542775975994));
#68304=CARTESIAN_POINT('Ctrl Pts',(-6.96346089814949,2.60605106873689,12.9661463572045));
#68305=CARTESIAN_POINT('Ctrl Pts',(-7.55575241306533,-2.27132217022394,
13.1780151168096));
#68306=CARTESIAN_POINT('Ctrl Pts',(-3.5424084439077,-7.68213674439024,13.442851066316));
#68307=CARTESIAN_POINT('Ctrl Pts',(4.54725929875602,-7.13266107804405,13.7606542057237));
#68308=CARTESIAN_POINT('Ctrl Pts',(8.45272122443086,-0.044584752292944,
14.0784573451314));
#68309=CARTESIAN_POINT('Ctrl Pts',(4.62224810690034,7.08429556290701,14.3962604845391));
#68310=CARTESIAN_POINT('Ctrl Pts',(-3.46117314465833,7.71907785980134,14.7140636239467));
#68311=CARTESIAN_POINT('Ctrl Pts',(-7.53137202013759,2.35090076838269,14.9788995734532));
#68312=CARTESIAN_POINT('Ctrl Pts',(-6.99056444882148,-2.53244911889549,
15.1907683330582));
#68313=CARTESIAN_POINT('Ctrl Pts',(-4.2782092022636,-6.62911947019817,15.4026370926634));
#68314=CARTESIAN_POINT('Ctrl Pts',(2.28580898234256,-8.14487322425717,15.6674730421697));
#68315=CARTESIAN_POINT('Ctrl Pts',(8.08711623839152,-2.48011534633209,15.9852761815774));
#68316=CARTESIAN_POINT('Ctrl Pts',(6.46292974909255,5.44802927271645,16.3030793209851));
#68317=CARTESIAN_POINT('Ctrl Pts',(-1.07613354736694,8.3901345503275,16.6208824603928));
#68318=CARTESIAN_POINT('Ctrl Pts',(-7.64073014880849,3.63085738305271,16.9386855998004));
#68319=CARTESIAN_POINT('Ctrl Pts',(-7.25736883688716,-3.09497923965129,
17.2035215493068));
#68320=CARTESIAN_POINT('Ctrl Pts',(-3.67864883055087,-6.461333657567,17.415390308912));
#68321=CARTESIAN_POINT('Ctrl Pts',(1.04280598275233,-7.82054055745697,17.6272590685171));
#68322=CARTESIAN_POINT('Ctrl Pts',(7.02221757620737,-4.7172389016652,17.8920950180235));
#68323=CARTESIAN_POINT('Ctrl Pts',(7.76418980207104,3.35704898709919,18.2098981574311));
#68324=CARTESIAN_POINT('Ctrl Pts',(1.38614201218807,8.3384107730507,18.5277012968388));
#68325=CARTESIAN_POINT('Ctrl Pts',(-6.26050369808442,5.68845450281879,18.8455044362465));
#68326=CARTESIAN_POINT('Ctrl Pts',(-8.17071856398859,-2.19162968839898,
19.1633075756542));
#68327=CARTESIAN_POINT('Ctrl Pts',(-3.51690828243854,-7.06255301299811,
19.4281435251605));
#68328=CARTESIAN_POINT('Ctrl Pts',(1.39036080365274,-7.30398430232345,19.6400122847657));
#68329=CARTESIAN_POINT('Ctrl Pts',(5.86572846132239,-5.27650722983735,19.8518810443708));
#68330=CARTESIAN_POINT('Ctrl Pts',(8.40448799323367,0.96356842754967,20.1167169938771));
#68331=CARTESIAN_POINT('Ctrl Pts',(3.73272469620222,7.59073036846454,20.4345201332849));
#68332=CARTESIAN_POINT('Ctrl Pts',(-4.35273170982645,7.24597892353766,20.7523232726925));
#68333=CARTESIAN_POINT('Ctrl Pts',(-8.45456569726709,0.269703642841959,
21.0701264121002));
#68334=CARTESIAN_POINT('Ctrl Pts',(-4.7979912386976,-6.96729234468889,21.3879295515078));
#68335=CARTESIAN_POINT('Ctrl Pts',(1.90339146903726,-7.65672252625688,21.6527655010143));
#68336=CARTESIAN_POINT('Ctrl Pts',(5.79526936145095,-4.65791185845644,21.8646342606193));
#68337=CARTESIAN_POINT('Ctrl Pts',(7.88690582824129,-0.212168293925783,
22.0765030202245));
#68338=CARTESIAN_POINT('Ctrl Pts',(5.7723835024817,6.18413059720254,22.3413389697309));
#68339=CARTESIAN_POINT('Ctrl Pts',(-2.08166357763857,8.19872538471076,22.6591421091385));
#68340=CARTESIAN_POINT('Ctrl Pts',(-8.0125380371007,2.69253005593165,22.9769452485462));
#68341=CARTESIAN_POINT('Ctrl Pts',(-6.61033334483714,-5.27787023850547,
23.2947483879539));
#68342=CARTESIAN_POINT('Ctrl Pts',(0.866480170453653,-8.415051672877,23.6125515273616));
#68343=CARTESIAN_POINT('Ctrl Pts',(6.41454280372272,-4.59368474622524,23.8773874768679));
#68344=CARTESIAN_POINT('Ctrl Pts',(7.43208735535594,0.212996233017501,24.0892562364731));
#68345=CARTESIAN_POINT('Ctrl Pts',(6.14092963596756,4.95351210098338,24.3011249960782));
#68346=CARTESIAN_POINT('Ctrl Pts',(0.383119799997728,8.45086396540785,24.5659609455846));
#68347=CARTESIAN_POINT('Ctrl Pts',(-6.90175237252995,4.89062729848073,24.8837640849922));
#68348=CARTESIAN_POINT('Ctrl Pts',(-7.84518301086339,-3.14699657199386,
25.2015672244));
#68349=CARTESIAN_POINT('Ctrl Pts',(-1.60869790813515,-8.30448747513831,
25.5193703638076));
#68350=CARTESIAN_POINT('Ctrl Pts',(6.11708029355421,-5.84339038788187,25.8371735032153));
#68351=CARTESIAN_POINT('Ctrl Pts',(7.86180973559087,0.663510821209555,26.1020094527216));
#68352=CARTESIAN_POINT('Ctrl Pts',(5.5189942760609,4.98216740322208,26.3138782123268));
#68353=CARTESIAN_POINT('Ctrl Pts',(1.46175943343325,7.7531644047616,26.5257469719319));
#68354=CARTESIAN_POINT('Ctrl Pts',(-5.18913976291492,6.68107110154611,26.7905829214383));
#68355=CARTESIAN_POINT('Ctrl Pts',(-8.42524278257166,-0.753462168321561,
27.108386060846));
#68356=CARTESIAN_POINT('Ctrl Pts',(-3.93060318626917,-7.48337106457854,
27.4261892002536));
#68357=CARTESIAN_POINT('Ctrl Pts',(4.16132657520632,-7.36449470899731,27.7439923396613));
#68358=CARTESIAN_POINT('Ctrl Pts',(8.44587796312302,-0.480653695514949,
28.061795479069));
#68359=CARTESIAN_POINT('Ctrl Pts',(5.55391017097628,5.60378271716701,28.3266314285754));
#68360=CARTESIAN_POINT('Ctrl Pts',(0.96977248127154,7.37162337531496,28.5385001881804));
#68361=CARTESIAN_POINT('Ctrl Pts',(-3.91561515650766,6.84954428225856,28.7503689477857));
#68362=CARTESIAN_POINT('Ctrl Pts',(-8.28282448891055,1.72008750617031,29.015204897292));
#68363=CARTESIAN_POINT('Ctrl Pts',(-5.92444483078517,-6.03766301074766,
29.3330080366997));
#68364=CARTESIAN_POINT('Ctrl Pts',(1.86141578941846,-8.2453389958803,29.6508111761073));
#68365=CARTESIAN_POINT('Ctrl Pts',(7.9437076708687,-2.90687626571029,29.968614315515));
#68366=CARTESIAN_POINT('Ctrl Pts',(6.74053094754093,5.11166558845771,30.2864174549227));
#68367=CARTESIAN_POINT('Ctrl Pts',(0.593204433234717,7.86742698910412,30.5512534044291));
#68368=CARTESIAN_POINT('Ctrl Pts',(-4.04265781809357,6.24004868720817,30.7631221640342));
#68369=CARTESIAN_POINT('Ctrl Pts',(-7.42270957644242,2.67426279043094,30.9749909236393));
#68370=CARTESIAN_POINT('Ctrl Pts',(-7.42024646331645,-4.06248999587925,
31.2398268731457));
#68371=CARTESIAN_POINT('Ctrl Pts',(-0.593856094554934,-8.43799479280045,
31.5576300125534));
#68372=CARTESIAN_POINT('Ctrl Pts',(6.76433588793489,-5.0689489929646,31.875433151961));
#68373=CARTESIAN_POINT('Ctrl Pts',(7.93180400173229,2.93920167094248,32.1932362913687));
#68374=CARTESIAN_POINT('Ctrl Pts',(1.81559240863278,8.2624153096231,32.5110394307764));
#68375=CARTESIAN_POINT('Ctrl Pts',(-4.6508433705407,6.37322170265487,32.7758753802828));
#68376=CARTESIAN_POINT('Ctrl Pts',(-7.1241264552189,2.12793611346102,32.9877441398879));
#68377=CARTESIAN_POINT('Ctrl Pts',(-7.38437218715985,-2.77837116490822,
33.199612899493));
#68378=CARTESIAN_POINT('Ctrl Pts',(-3.01341312605451,-7.90463306388738,
33.4644488489995));
#68379=CARTESIAN_POINT('Ctrl Pts',(5.02038597150706,-6.80794725901008,33.7822519884071));
#68380=CARTESIAN_POINT('Ctrl Pts',(8.43629411486896,0.528607137209164,34.1000551278148));
#68381=CARTESIAN_POINT('Ctrl Pts',(4.1313013145946,7.38137999512265,34.4178582672224));
#68382=CARTESIAN_POINT('Ctrl Pts',(-3.97655762654219,7.46665065379174,34.7356614066301));
#68383=CARTESIAN_POINT('Ctrl Pts',(-7.67343176575536,1.83486889580421,35.0004973561365));
#68384=CARTESIAN_POINT('Ctrl Pts',(-6.80278048844522,-3.0005778575052,35.2123661157416));
#68385=CARTESIAN_POINT('Ctrl Pts',(-3.81891471135974,-6.90392564819853,
35.4242348753467));
#68386=CARTESIAN_POINT('Ctrl Pts',(2.83276667106822,-7.9711552193057,35.6890708248531));
#68387=CARTESIAN_POINT('Ctrl Pts',(8.23665787120028,-1.92610703159567,36.0068739642608));
#68388=CARTESIAN_POINT('Ctrl Pts',(6.07868534894961,5.87367587857433,36.3246771036684));
#68389=CARTESIAN_POINT('Ctrl Pts',(-1.64250329731608,8.29786744306471,36.6424802430762));
#68390=CARTESIAN_POINT('Ctrl Pts',(-7.86931852960366,3.10446588362884,36.9602833824838));
#68391=CARTESIAN_POINT('Ctrl Pts',(-7.03083175665605,-3.57990275539581,
37.2251193319902));
#68392=CARTESIAN_POINT('Ctrl Pts',(-3.23210971831374,-6.69587609067724,
37.4369880915954));
#68393=CARTESIAN_POINT('Ctrl Pts',(1.57063429798398,-7.73184368895865,37.6488568512004));
#68394=CARTESIAN_POINT('Ctrl Pts',(7.32588516890857,-4.23028238241191,37.9136928007069));
#68395=CARTESIAN_POINT('Ctrl Pts',(7.51871834614993,3.87573162327282,38.2314959401145));
#68396=CARTESIAN_POINT('Ctrl Pts',(0.817613343300754,8.4132034516549,38.5492990795222));
#68397=CARTESIAN_POINT('Ctrl Pts',(-6.63177183421585,5.25090692388172,38.8671022189298));
#68398=CARTESIAN_POINT('Ctrl Pts',(-8.00332638643711,-2.74055638422911,
39.1849053583376));
#68399=CARTESIAN_POINT('Ctrl Pts',(-3.02997903692706,-7.28474611529298,
39.4497413078438));
#68400=CARTESIAN_POINT('Ctrl Pts',(1.88236719001822,-7.19291203997827,39.6616100674491));
#68401=CARTESIAN_POINT('Ctrl Pts',(6.20997521372375,-4.86667307032534,39.8734788270541));
#68402=CARTESIAN_POINT('Ctrl Pts',(8.31981970420338,1.53117034732538,40.1383147765605));
#68403=CARTESIAN_POINT('Ctrl Pts',(3.20948875182505,7.82634034119881,40.4561179159682));
#68404=CARTESIAN_POINT('Ctrl Pts',(-4.83398887575954,6.93419320808945,40.7739210553758));
#68405=CARTESIAN_POINT('Ctrl Pts',(-8.4533972658104,-0.304131305124825,
41.0917241947836));
#68406=CARTESIAN_POINT('Ctrl Pts',(-4.31457280315205,-7.27656128052804,
41.4095273341912));
#68407=CARTESIAN_POINT('Ctrl Pts',(2.41813279325872,-7.51005544071813,41.6743632836976));
#68408=CARTESIAN_POINT('Ctrl Pts',(6.09773785643282,-4.25427818638455,41.8862320433027));
#68409=CARTESIAN_POINT('Ctrl Pts',(7.88314273544256,0.323047273835714,42.0981008029079));
#68410=CARTESIAN_POINT('Ctrl Pts',(5.33982085001841,6.56126480434131,42.3629367524142));
#68411=CARTESIAN_POINT('Ctrl Pts',(-2.63274215352489,8.03872439740416,42.6807398918219));
#68412=CARTESIAN_POINT('Ctrl Pts',(-8.17665286289524,2.14308932566695,42.9985430312296));
#68413=CARTESIAN_POINT('Ctrl Pts',(-6.23728644307629,-5.71390225777308,
43.3163461706372));
#68414=CARTESIAN_POINT('Ctrl Pts',(1.43502170377997,-8.33694160065068,43.634149310045));
#68415=CARTESIAN_POINT('Ctrl Pts',(6.71123177593405,-4.14821250398127,43.8989852595513));
#68416=CARTESIAN_POINT('Ctrl Pts',(7.40054491816626,0.716397073643458,44.1108540191565));
#68417=CARTESIAN_POINT('Ctrl Pts',(5.79095412635695,5.35846519396396,44.3227227787615));
#68418=CARTESIAN_POINT('Ctrl Pts',(-0.190725146312963,8.4573935974119,44.587558728268));
#68419=CARTESIAN_POINT('Ctrl Pts',(-7.21745278538906,4.41143927477727,44.9053618676755));
#68420=CARTESIAN_POINT('Ctrl Pts',(-7.61376661200979,-3.67165383389088,
45.2231650070833));
#68421=CARTESIAN_POINT('Ctrl Pts',(-1.04195711115155,-8.39444736494835,
45.540968146491));
#68422=CARTESIAN_POINT('Ctrl Pts',(6.49918300830777,-5.41521031609143,45.8587712858986));
#68423=CARTESIAN_POINT('Ctrl Pts',(7.79873388426272,1.19500992922489,46.123607235405));
#68424=CARTESIAN_POINT('Ctrl Pts',(5.16850704380232,5.34488772483455,46.3354759950102));
#68425=CARTESIAN_POINT('Ctrl Pts',(0.932736110642546,7.83443056491003,46.5473447546152));
#68426=CARTESIAN_POINT('Ctrl Pts',(-5.6301719296693,6.31387730205009,46.8121807041218));
#68427=CARTESIAN_POINT('Ctrl Pts',(-8.35477181135561,-1.32295470993732,
47.1299838435293));
#68428=CARTESIAN_POINT('Ctrl Pts',(-3.41419081316633,-7.732644113715,47.447786982937));
#68429=CARTESIAN_POINT('Ctrl Pts',(4.65105946660589,-7.06541343606045,47.7655901223447));
#68430=CARTESIAN_POINT('Ctrl Pts',(8.4590318061587,0.0930776309034,48.0833932617524));
#68431=CARTESIAN_POINT('Ctrl Pts',(5.16119746048464,5.96743996219319,48.3482292112587));
#68432=CARTESIAN_POINT('Ctrl Pts',(0.467749480146434,7.4204110584754,48.5600979708639));
#68433=CARTESIAN_POINT('Ctrl Pts',(-4.37100011405199,6.56830700648585,48.7719667304689));
#68434=CARTESIAN_POINT('Ctrl Pts',(-8.38038637202662,1.15455913600378,49.0368026799754));
#68435=CARTESIAN_POINT('Ctrl Pts',(-5.50146269355898,-6.42544390806941,
49.354605819383));
#68436=CARTESIAN_POINT('Ctrl Pts',(2.41616153527492,-8.10016341400214,49.6724089587907));
#68437=CARTESIAN_POINT('Ctrl Pts',(8.12251341825707,-2.36160897580472,49.9902120981984));
#68438=CARTESIAN_POINT('Ctrl Pts',(6.37845303077979,5.55690736625286,50.3080152376061));
#68439=CARTESIAN_POINT('Ctrl Pts',(0.0584327448535862,7.88954273344295,
50.5728511871124));
#68440=CARTESIAN_POINT('Ctrl Pts',(-4.45642702083661,5.95160046213443,50.7847199467176));
#68441=CARTESIAN_POINT('Ctrl Pts',(-7.58694310329044,2.16485410037873,50.9965887063226));
#68442=CARTESIAN_POINT('Ctrl Pts',(-7.12773796343645,-4.55623024742675,
51.2614246558292));
#68443=CARTESIAN_POINT('Ctrl Pts',(-0.0203987606110949,-8.45884182822524,
51.5792277952367));
#68444=CARTESIAN_POINT('Ctrl Pts',(7.09244260083074,-4.59866739958459,51.8970309346444));
#68445=CARTESIAN_POINT('Ctrl Pts',(7.71427665221152,3.47020992412735,52.2148340740521));
#68446=CARTESIAN_POINT('Ctrl Pts',(1.25122800903597,8.3664993284159,52.5326372134597));
#68447=CARTESIAN_POINT('Ctrl Pts',(-5.07224217124685,6.0432324367609,52.7974731629662));
#68448=CARTESIAN_POINT('Ctrl Pts',(-7.25200641689262,1.64002828703338,53.0093419225713));
#68449=CARTESIAN_POINT('Ctrl Pts',(-7.17900870165025,-3.27263395296864,
53.2212106821764));
#68450=CARTESIAN_POINT('Ctrl Pts',(-2.470549926415,-8.09075185653782,53.4860466316827));
#68451=CARTESIAN_POINT('Ctrl Pts',(5.47040857048482,-6.45190291746039,53.8038497710905));
#68452=CARTESIAN_POINT('Ctrl Pts',(8.38104274703086,1.09936634954972,54.1216529104981));
#68453=CARTESIAN_POINT('Ctrl Pts',(3.62134206171429,7.64449493795545,54.4394560499058));
#68454=CARTESIAN_POINT('Ctrl Pts',(-4.47364178624171,7.17986153845404,54.7572591893135));
#68455=CARTESIAN_POINT('Ctrl Pts',(-7.7801779847604,1.31039286244344,55.0220951388199));
#68456=CARTESIAN_POINT('Ctrl Pts',(-6.58368978329653,-3.45489778289289,
55.233963898425));
#68457=CARTESIAN_POINT('Ctrl Pts',(-3.34204537905406,-7.14695960621277,
55.4458326580302));
#68458=CARTESIAN_POINT('Ctrl Pts',(3.36668782226014,-7.76075354913583,55.7106686075364));
#68459=CARTESIAN_POINT('Ctrl Pts',(8.34829398196702,-1.36323467349575,56.0284717469442));
#68460=CARTESIAN_POINT('Ctrl Pts',(5.66646652701038,6.272291526735,56.3462748863518));
#68461=CARTESIAN_POINT('Ctrl Pts',(-2.20131416283494,8.16741312417033,56.6640780257595));
#68462=CARTESIAN_POINT('Ctrl Pts',(-8.06169190285053,2.5637874729575,56.9818811651672));
#68463=CARTESIAN_POINT('Ctrl Pts',(-6.77193842801764,-4.04835137502064,
57.2467171146735));
#68464=CARTESIAN_POINT('Ctrl Pts',(-2.77069627135412,-6.89960375853757,
57.4585858742787));
#68465=CARTESIAN_POINT('Ctrl Pts',(2.09123447360709,-7.60756447918061,57.6704546338838));
#68466=CARTESIAN_POINT('Ctrl Pts',(7.5958386622641,-3.72385788663226,57.9352905833903));
#68467=CARTESIAN_POINT('Ctrl Pts',(7.23864536270936,4.37657794370142,58.2530937227978));
#68468=CARTESIAN_POINT('Ctrl Pts',(0.245321975866281,8.44927813639946,58.5708968622056));
#68469=CARTESIAN_POINT('Ctrl Pts',(-6.97252021617379,4.78919440192351,58.8887000016132));
#68470=CARTESIAN_POINT('Ctrl Pts',(-7.79910249030586,-3.27687089899559,
59.2065031410209));
#68471=CARTESIAN_POINT('Ctrl Pts',(-2.52910567245795,-7.473414442277,59.4713390905273));
#68472=CARTESIAN_POINT('Ctrl Pts',(2.36571082601458,-7.04873762744781,59.6832078501324));
#68473=CARTESIAN_POINT('Ctrl Pts',(6.52564334163617,-4.43444223169647,59.8950766097376));
#68474=CARTESIAN_POINT('Ctrl Pts',(8.19686317810968,2.09172574261759,60.1599125592438));
#68475=CARTESIAN_POINT('Ctrl Pts',(2.67148257557379,8.0259330942124,60.4777156986516));
#68476=CARTESIAN_POINT('Ctrl Pts',(-5.29299977691561,6.59049597979186,60.7955188380592));
#68477=CARTESIAN_POINT('Ctrl Pts',(-8.41332586649955,-0.876566625224416,
61.113321977467));
#68478=CARTESIAN_POINT('Ctrl Pts',(-3.81129848224015,-7.55234310808594,
61.4311251168746));
#68479=CARTESIAN_POINT('Ctrl Pts',(2.92174574632196,-7.32882669479521,61.6959610663809));
#68480=CARTESIAN_POINT('Ctrl Pts',(6.37214424900164,-3.83106610786561,61.9078298259862));
#68481=CARTESIAN_POINT('Ctrl Pts',(7.84310101539102,0.856776161471738,62.1196985855912));
#68482=CARTESIAN_POINT('Ctrl Pts',(4.8826840680845,6.90820373427514,62.3845345350977));
#68483=CARTESIAN_POINT('Ctrl Pts',(-3.17170471496819,7.84172878805536,62.7023376745052));
#68484=CARTESIAN_POINT('Ctrl Pts',(-8.3031383127742,1.58378598839051,63.020140813913));
#68485=CARTESIAN_POINT('Ctrl Pts',(-5.83553522914796,-6.12363860574255,
63.3379439533206));
#68486=CARTESIAN_POINT('Ctrl Pts',(1.99695919361291,-8.2204644955151,63.6557470927283));
#68487=CARTESIAN_POINT('Ctrl Pts',(6.97703531524421,-3.68364997500153,63.9205830422348));
#68488=CARTESIAN_POINT('Ctrl Pts',(7.3349447936348,1.21650101818743,64.1324518018397));
#68489=CARTESIAN_POINT('Ctrl Pts',(5.41432834879617,5.73875835524684,64.344320561445));
#68490=CARTESIAN_POINT('Ctrl Pts',(-0.763692365716531,8.42500187023871,
64.6091565109513));
#68491=CARTESIAN_POINT('Ctrl Pts',(-7.49993811029349,3.91194958123631,64.926959650359));
#68492=CARTESIAN_POINT('Ctrl Pts',(-7.34731126864177,-4.17941395649796,
65.2447627897667));
#68493=CARTESIAN_POINT('Ctrl Pts',(-0.470421174093057,-8.44577557737201,
65.5625659291743));
#68494=CARTESIAN_POINT('Ctrl Pts',(6.85137614946615,-4.96210916864047,65.8803690685821));
#68495=CARTESIAN_POINT('Ctrl Pts',(7.69976785954471,1.72100954024463,66.1452050180884));
#68496=CARTESIAN_POINT('Ctrl Pts',(4.79423407699781,5.68301059895882,66.3570737776935));
#68497=CARTESIAN_POINT('Ctrl Pts',(0.399420288423597,7.87964227371272,66.5689425372987));
#68498=CARTESIAN_POINT('Ctrl Pts',(-6.04529375638949,5.91762671532605,66.833778486805));
#68499=CARTESIAN_POINT('Ctrl Pts',(-8.24585175168749,-1.8863589461156,67.1515816262127));
#68500=CARTESIAN_POINT('Ctrl Pts',(-2.88206615879987,-7.94633113797258,
67.4693847656204));
#68501=CARTESIAN_POINT('Ctrl Pts',(5.11938794374809,-6.73381676806031,67.787187905028));
#68502=CARTESIAN_POINT('Ctrl Pts',(8.43325675090628,0.666380609302265,68.1049910444358));
#68503=CARTESIAN_POINT('Ctrl Pts',(4.74473265450711,6.30363474237736,68.3698269939421));
#68504=CARTESIAN_POINT('Ctrl Pts',(-0.0364261280579175,7.4350496293269,
68.5816957535472));
#68505=CARTESIAN_POINT('Ctrl Pts',(-4.80626950490606,6.25684204486051,68.7935645131524));
#68506=CARTESIAN_POINT('Ctrl Pts',(-8.43938128704969,0.583717425620363,
69.0584004626587));
#68507=CARTESIAN_POINT('Ctrl Pts',(-5.05316254300341,-6.7836545831746,69.3762036020665));
#68508=CARTESIAN_POINT('Ctrl Pts',(2.95978798216355,-7.91771046410669,69.694006741474));
#68509=CARTESIAN_POINT('Ctrl Pts',(8.26393894154964,-1.80547344113602,70.0118098808819));
#68510=CARTESIAN_POINT('Ctrl Pts',(5.98702114732562,5.97657597305592,70.3296130202893));
#68511=CARTESIAN_POINT('Ctrl Pts',(-0.476607856380058,7.87535039433149,
70.5944489697959));
#68512=CARTESIAN_POINT('Ctrl Pts',(-4.84968751467229,5.63576267054211,70.8063177294009));
#68513=CARTESIAN_POINT('Ctrl Pts',(-7.71626113646769,1.64548263069972,71.0181864890061));
#68514=CARTESIAN_POINT('Ctrl Pts',(-6.80242723150402,-5.02900247240576,
71.2830224385124));
#68515=CARTESIAN_POINT('Ctrl Pts',(0.553152422106158,-8.44076087529441,
71.6008255779202));
#68516=CARTESIAN_POINT('Ctrl Pts',(7.38790957909878,-4.10722243773945,71.9186287173277));
#68517=CARTESIAN_POINT('Ctrl Pts',(7.46124771108228,3.98524796982142,72.2364318567355));
#68518=CARTESIAN_POINT('Ctrl Pts',(0.681105581927244,8.43208053298718,72.5542349961431));
#68519=CARTESIAN_POINT('Ctrl Pts',(-5.4702985817129,5.68543147735568,72.8190709456496));
#68520=CARTESIAN_POINT('Ctrl Pts',(-7.34651183457599,1.14457353746562,73.0309397052545));
#68521=CARTESIAN_POINT('Ctrl Pts',(-6.94060811730116,-3.75183730228112,
73.2428084648599));
#68522=CARTESIAN_POINT('Ctrl Pts',(-1.91631486239838,-8.23963364106499,
73.507644414366));
#68523=CARTESIAN_POINT('Ctrl Pts',(5.89525226469161,-6.06617154303566,73.8254475537739));
#68524=CARTESIAN_POINT('Ctrl Pts',(8.28722834591438,1.66507528224125,74.1432506931814));
#68525=CARTESIAN_POINT('Ctrl Pts',(3.09470404059807,7.8724123713359,74.4610538325893));
#68526=CARTESIAN_POINT('Ctrl Pts',(-4.95011189218524,6.86006436447352,74.7788569719968));
#68527=CARTESIAN_POINT('Ctrl Pts',(-7.85116507114007,0.779826871913311,
75.0436929215033));
#68528=CARTESIAN_POINT('Ctrl Pts',(-6.33423966281534,-3.89323870918931,
75.2555616811083));
#68529=CARTESIAN_POINT('Ctrl Pts',(-2.84994413976273,-7.35729615265609,
75.4674304407135));
#68530=CARTESIAN_POINT('Ctrl Pts',(3.88543032268657,-7.5142261247853,75.7322663902198));
#68531=CARTESIAN_POINT('Ctrl Pts',(8.42098238217486,-0.794776998686755,
76.0500695296276));
#68532=CARTESIAN_POINT('Ctrl Pts',(5.22913513009899,6.64329840099667,76.3678726690352));
#68533=CARTESIAN_POINT('Ctrl Pts',(-2.7518091883857,7.99700948568447,76.6856758084429));
#68534=CARTESIAN_POINT('Ctrl Pts',(-8.21345806569579,2.01586733850936,77.0034789478505));
#68535=CARTESIAN_POINT('Ctrl Pts',(-6.14214966524969,-5.80958392169303,
77.3212820872583));
#68536=CARTESIAN_POINT('Ctrl Pts',(1.55454614605433,-8.31432505007639,77.6390852266658));
#68537=CARTESIAN_POINT('Ctrl Pts',(7.83537994160767,-3.18857087384152,77.9568883660737));
#68538=CARTESIAN_POINT('Ctrl Pts',(7.06879253230392,3.50487666158179,78.2217243155799));
#68539=CARTESIAN_POINT('Ctrl Pts',(3.30326759019129,6.66095511021538,78.4335930751852));
#68540=CARTESIAN_POINT('Ctrl Pts',(-1.48802546613442,7.74820644643544,78.6454618347901));
#68541=CARTESIAN_POINT('Ctrl Pts',(-7.28038169229118,4.30814730997263,78.9102977842966));
#68542=CARTESIAN_POINT('Ctrl Pts',(-7.55961163766212,-3.79530519602571,
79.2281009237043));
#68543=CARTESIAN_POINT('Ctrl Pts',(-0.90730672759395,-8.4040123664188,79.5459040631119));
#68544=CARTESIAN_POINT('Ctrl Pts',(6.57539537422739,-5.32133555853004,79.8637072025197));
#68545=CARTESIAN_POINT('Ctrl Pts',(8.03209799109985,2.65503805098697,80.1815103419273));
#68546=CARTESIAN_POINT('Ctrl Pts',(3.10750385441467,7.25201654545354,80.4463462914337));
#68547=CARTESIAN_POINT('Ctrl Pts',(-1.80554424357141,7.21257892176842,80.6582150510388));
#68548=CARTESIAN_POINT('Ctrl Pts',(-6.15771582622757,4.93262946715277,80.8700838106439));
#68549=CARTESIAN_POINT('Ctrl Pts',(-8.33567749448872,-1.44234795953961,
81.1349197601503));
#68550=CARTESIAN_POINT('Ctrl Pts',(-3.29277836034727,-7.79166410060939,
81.4527228995579));
#68551=CARTESIAN_POINT('Ctrl Pts',(4.75975683582896,-6.98535603715296,81.7705260389657));
#68552=CARTESIAN_POINT('Ctrl Pts',(8.45616021047951,0.213953851766904,82.0883291783733));
#68553=CARTESIAN_POINT('Ctrl Pts',(4.39193595102736,7.23013006172392,82.406132317781));
#68554=CARTESIAN_POINT('Ctrl Pts',(-2.337896323999,7.53541901902798,82.6709682672874));
#68555=CARTESIAN_POINT('Ctrl Pts',(-6.05201678514127,4.31907197219638,82.8828370268925));
#68556=CARTESIAN_POINT('Ctrl Pts',(-7.88613982887975,-0.238950793295768,
83.0947057864976));
#68557=CARTESIAN_POINT('Ctrl Pts',(-5.40949666956307,-6.50393944945827,
83.359541736004));
#68558=CARTESIAN_POINT('Ctrl Pts',(2.54685493909067,-8.06634682464978,83.6773448754118));
#68559=CARTESIAN_POINT('Ctrl Pts',(8.15333054530708,-2.230175982237,83.9951480148192));
#68560=CARTESIAN_POINT('Ctrl Pts',(6.29787362155546,5.6470531285578,84.3129511542271));
#68561=CARTESIAN_POINT('Ctrl Pts',(-1.34602196100505,8.35177271132716,84.6307542936346));
#68562=CARTESIAN_POINT('Ctrl Pts',(-6.66660705557152,4.21955558023922,84.8955902431412));
#68563=CARTESIAN_POINT('Ctrl Pts',(-7.40776475847419,-0.637425396785901,
85.1074590027462));
#68564=CARTESIAN_POINT('Ctrl Pts',(-5.84777575731517,-5.29639666379029,
85.3193277623513));
#68565=CARTESIAN_POINT('Ctrl Pts',(0.100511489746323,-8.45894674197618,
85.5841637118577));
#68566=CARTESIAN_POINT('Ctrl Pts',(7.16999181195573,-4.4881665077057,85.9019668512654));
#68567=CARTESIAN_POINT('Ctrl Pts',(7.65249378215863,3.59023993794783,86.219769990673));
#68568=CARTESIAN_POINT('Ctrl Pts',(1.13142929779594,8.38285684766757,86.5375731300808));
#68569=CARTESIAN_POINT('Ctrl Pts',(-6.44105711244674,5.48421970905446,86.8553762694884));
#68570=CARTESIAN_POINT('Ctrl Pts',(-7.81103574848863,-1.11176412260787,
87.1202122189948));
#68571=CARTESIAN_POINT('Ctrl Pts',(-5.22521926747735,-5.28945871140975,
87.3320809786));
#68572=CARTESIAN_POINT('Ctrl Pts',(-1.01624161886705,-7.82403680337547,
87.543949738205));
#68573=CARTESIAN_POINT('Ctrl Pts',(5.56251067857787,-6.37356709336982,87.8087856877114));
#68574=CARTESIAN_POINT('Ctrl Pts',(8.36840665116155,1.23377117212372,88.1265888271191));
#68575=CARTESIAN_POINT('Ctrl Pts',(3.49646957042679,7.69579004658781,88.4443919665267));
#68576=CARTESIAN_POINT('Ctrl Pts',(-4.57543835510379,7.11461770181735,88.7621951059345));
#68577=CARTESIAN_POINT('Ctrl Pts',(-8.45954339245076,-0.002852056000995,
89.0799982453421));
#68578=CARTESIAN_POINT('Ctrl Pts',(-5.22454996591466,-5.91205349960188,
89.3448341948485));
#68579=CARTESIAN_POINT('Ctrl Pts',(-0.54686568779491,-7.41500018694766,
89.5567029544537));
#68580=CARTESIAN_POINT('Ctrl Pts',(4.30069684861065,-6.61455255817383,89.7685717140586));
#68581=CARTESIAN_POINT('Ctrl Pts',(8.36759569126859,-1.24387494968049,90.0334076635652));
#68582=CARTESIAN_POINT('Ctrl Pts',(5.56968071207069,6.36640227679301,90.3512108029727));
#68583=CARTESIAN_POINT('Ctrl Pts',(-2.32963135753805,8.12547239463998,90.6690139423806));
#68584=CARTESIAN_POINT('Ctrl Pts',(-8.09686354683089,2.44810577556786,90.9868170817879));
#68585=CARTESIAN_POINT('Ctrl Pts',(-6.43735774178527,-5.48856154627573,
91.3046202211961));
#68586=CARTESIAN_POINT('Ctrl Pts',(-0.142575784227132,-7.88847076905561,
91.5694561707021));
#68587=CARTESIAN_POINT('Ctrl Pts',(4.39269641485442,-5.99879221675887,91.7813249303074));
#68588=CARTESIAN_POINT('Ctrl Pts',(7.5634221946081,-2.24564993589899,91.9931936899123));
#68589=CARTESIAN_POINT('Ctrl Pts',(7.17592727787235,4.47994980392269,92.258029639419));
#68590=CARTESIAN_POINT('Ctrl Pts',(0.11061585490748,8.45814313646977,92.5758327788264));
#68591=CARTESIAN_POINT('Ctrl Pts',(-7.04299184568019,4.67405068005932,92.8936359182344));
#68592=CARTESIAN_POINT('Ctrl Pts',(-7.75084959410668,-3.38773549054587,
93.2114390576417));
#68593=CARTESIAN_POINT('Ctrl Pts',(-1.34039021126954,-8.35267841021741,
93.5292421970496));
#68594=CARTESIAN_POINT('Ctrl Pts',(5.00749923252853,-6.0969869906963,93.7940781465558));
#68595=CARTESIAN_POINT('Ctrl Pts',(7.234102118271,-1.71728168782766,94.0059469061612));
#68596=CARTESIAN_POINT('Ctrl Pts',(7.21350483120897,3.19587968775712,94.217815665766));
#68597=CARTESIAN_POINT('Ctrl Pts',(2.55670177503496,8.06394187581435,94.4826516152727));
#68598=CARTESIAN_POINT('Ctrl Pts',(-5.40128428653493,6.50988089295023,94.8004547546802));
#68599=CARTESIAN_POINT('Ctrl Pts',(-8.39229139831418,-1.00991533499733,
95.1182578940879));
#68600=CARTESIAN_POINT('Ctrl Pts',(-3.70266887648321,-7.60543650131208,
95.4360610334955));
#68601=CARTESIAN_POINT('Ctrl Pts',(4.39681011332992,-7.22716703628046,95.7538641729033));
#68602=CARTESIAN_POINT('Ctrl Pts',(7.76575938965619,-1.39329825610326,96.0187001224095));
#68603=CARTESIAN_POINT('Ctrl Pts',(6.62016371895673,3.38448255825473,96.2305688820149));
#68604=CARTESIAN_POINT('Ctrl Pts',(3.41808158870619,7.11090832323413,96.4424376416197));
#68605=CARTESIAN_POINT('Ctrl Pts',(-3.28372357491219,7.79621972667172,96.7072735911263));
#68606=CARTESIAN_POINT('Ctrl Pts',(-8.33327948586795,1.45219633479086,97.0250767305339));
#68607=CARTESIAN_POINT('Ctrl Pts',(-5.73304170496459,-6.21149874887032,
97.3428798699416));
#68608=CARTESIAN_POINT('Ctrl Pts',(2.11407894975325,-8.19042681296763,97.6606830093493));
#68609=CARTESIAN_POINT('Ctrl Pts',(8.03388914470774,-2.64962407777525,97.978486148757));
#68610=CARTESIAN_POINT('Ctrl Pts',(6.81473116910066,3.97589461899854,98.2433220982633));
#68611=CARTESIAN_POINT('Ctrl Pts',(2.84412679083728,6.86966030095835,98.4551908578685));
#68612=CARTESIAN_POINT('Ctrl Pts',(-2.00997661900668,7.62943595028749,98.6670596174735));
#68613=CARTESIAN_POINT('Ctrl Pts',(-7.55568960481281,3.80465992418547,98.93189556698));
#68614=CARTESIAN_POINT('Ctrl Pts',(-7.28491227710381,-4.29912482945887,
99.2496987063876));
#68615=CARTESIAN_POINT('Ctrl Pts',(-0.335424274736072,-8.44618105737727,
99.5675018457952));
#68616=CARTESIAN_POINT('Ctrl Pts',(6.92104420556015,-4.86328780652038,99.8853049852031));
#68617=CARTESIAN_POINT('Ctrl Pts',(7.83360853914484,3.19350274751976,100.20310812461));
#68618=CARTESIAN_POINT('Ctrl Pts',(2.60866994349881,7.44601504526949,100.467944074117));
#68619=CARTESIAN_POINT('Ctrl Pts',(-2.29039755886778,7.0735683268951,100.679812833722));
#68620=CARTESIAN_POINT('Ctrl Pts',(-6.47797637805987,4.50378962361612,100.891681593327));
#68621=CARTESIAN_POINT('Ctrl Pts',(-8.21870637035112,-2.00418266156781,
101.156517542833));
#68622=CARTESIAN_POINT('Ctrl Pts',(-2.75693166724786,-7.9969837417925,101.474320682241));
#68623=CARTESIAN_POINT('Ctrl Pts',(5.22240741161874,-6.64657390880071,101.792123821649));
#68624=CARTESIAN_POINT('Ctrl Pts',(8.42219639853767,0.786783965791493,102.109926961056));
#68625=CARTESIAN_POINT('Ctrl Pts',(3.89163164200336,7.51126392199993,102.427730100465));
#68626=CARTESIAN_POINT('Ctrl Pts',(-2.8434135469081,7.35957188495038,102.69256604997));
#68627=CARTESIAN_POINT('Ctrl Pts',(-6.33092135832433,3.89881066578444,102.904434809576));
#68628=CARTESIAN_POINT('Ctrl Pts',(-7.85179290474972,-0.773076393000939,
103.116303569181));
#68629=CARTESIAN_POINT('Ctrl Pts',(-4.95608618404943,-6.85573426259024,
103.381139518688));
#68630=CARTESIAN_POINT('Ctrl Pts',(3.08788791202162,-7.87511075650104,103.698942658095));
#68631=CARTESIAN_POINT('Ctrl Pts',(8.28577408258241,-1.6722534946851,104.016745797503));
#68632=CARTESIAN_POINT('Ctrl Pts',(5.90051532458819,6.06105107128024,104.33454893691));
#68633=CARTESIAN_POINT('Ctrl Pts',(-1.90916978157587,8.24129560737247,104.652352076318));
#68634=CARTESIAN_POINT('Ctrl Pts',(-6.93735029424958,3.75785441753258,104.917188025824));
#68635=CARTESIAN_POINT('Ctrl Pts',(-7.3475022519864,-1.13820055788763,105.12905678543));
#68636=CARTESIAN_POINT('Ctrl Pts',(-5.47522743990438,-5.68068511799518,
105.340925545035));
#68637=CARTESIAN_POINT('Ctrl Pts',(0.673791595344492,-8.43266787138114,
105.605761494541));
#68638=CARTESIAN_POINT('Ctrl Pts',(7.45778840496133,-3.99171808763995,105.923564633949));
#68639=CARTESIAN_POINT('Ctrl Pts',(7.39146913864016,4.10081307433183,106.241367773356));
#68640=CARTESIAN_POINT('Ctrl Pts',(0.560473312880324,8.44027788937762,106.559170912764));
#68641=CARTESIAN_POINT('Ctrl Pts',(-6.79806279716929,5.03490066920113,106.876974052172));
#68642=CARTESIAN_POINT('Ctrl Pts',(-7.71768543134127,-1.63878934319104,
107.141810001678));
#68643=CARTESIAN_POINT('Ctrl Pts',(-4.8545738574009,-5.63155418299077,107.353678761283));
#68644=CARTESIAN_POINT('Ctrl Pts',(-0.483438338969841,-7.87493405057514,
107.565547520888));
#68645=CARTESIAN_POINT('Ctrl Pts',(5.98183512670323,-5.98176655010195,107.830383470395));
#68646=CARTESIAN_POINT('Ctrl Pts',(8.26550180637324,1.79830505565891,108.148186609802));
#68647=CARTESIAN_POINT('Ctrl Pts',(2.96665427361026,7.91514032212636,108.46598974921));
#68648=CARTESIAN_POINT('Ctrl Pts',(-5.04727685731576,6.78803487837035,108.783792888618));
#68649=CARTESIAN_POINT('Ctrl Pts',(-8.43988439848631,-0.576397330985157,
109.101596028025));
#68650=CARTESIAN_POINT('Ctrl Pts',(-4.81169455230378,-6.25267098637243,
109.366431977532));
#68651=CARTESIAN_POINT('Ctrl Pts',(-0.0428748849056034,-7.4350152385295,
109.578300737137));
#68652=CARTESIAN_POINT('Ctrl Pts',(4.73926342898019,-6.30774770256575,109.790169496742));
#68653=CARTESIAN_POINT('Ctrl Pts',(8.43267559531305,-0.673694921452692,
110.055005446249));
#68654=CARTESIAN_POINT('Ctrl Pts',(5.12522657618584,6.72937394763629,110.372808585656));
#68655=CARTESIAN_POINT('Ctrl Pts',(-2.87517284554175,7.94882790141666,110.690611725064));
#68656=CARTESIAN_POINT('Ctrl Pts',(-8.24421252162756,1.89351025415944,111.008414864471));
#68657=CARTESIAN_POINT('Ctrl Pts',(-6.05042412027553,-5.91238111996912,
111.326218003879));
#68658=CARTESIAN_POINT('Ctrl Pts',(0.392585751409091,-7.87998574594424,
111.591053953385));
#68659=CARTESIAN_POINT('Ctrl Pts',(4.78930312953449,-5.68716672749729,111.802922712991));
#68660=CARTESIAN_POINT('Ctrl Pts',(7.69827225026102,-1.72768726607415,112.014791472596));
#68661=CARTESIAN_POINT('Ctrl Pts',(6.85567744454336,4.9561647792783,112.279627422102));
#68662=CARTESIAN_POINT('Ctrl Pts',(-0.463095576155875,8.44618041908367,
112.59743056151));
#68663=CARTESIAN_POINT('Ctrl Pts',(-7.34368350139931,4.18578505532193,112.915233700918));
#68664=CARTESIAN_POINT('Ctrl Pts',(-7.50332830829109,-3.90544305839496,
113.233036840325));
#68665=CARTESIAN_POINT('Ctrl Pts',(-0.770999481427355,-8.42433631466713,
113.550839979733));
#68666=CARTESIAN_POINT('Ctrl Pts',(5.40934881541923,-5.74345229993392,113.815675929239));
#68667=CARTESIAN_POINT('Ctrl Pts',(7.3338869057028,-1.22286250546905,114.027544688844));
#68668=CARTESIAN_POINT('Ctrl Pts',(6.98022769487296,3.67759707638322,114.239413448449));
#68669=CARTESIAN_POINT('Ctrl Pts',(2.00408844048741,8.21872934617535,114.504249397956));
#68670=CARTESIAN_POINT('Ctrl Pts',(-5.83022171247392,6.12869773832626,114.822052537364));
#68671=CARTESIAN_POINT('Ctrl Pts',(-8.3045088821496,-1.57658368771828,115.139855676771));
#68672=CARTESIAN_POINT('Ctrl Pts',(-3.17850502455827,-7.83897486877112,
115.457658816179));
#68673=CARTESIAN_POINT('Ctrl Pts',(4.87669041934326,-6.91243611882708,115.775461955587));
#68674=CARTESIAN_POINT('Ctrl Pts',(7.8423549427161,-0.863578532010263,116.040297905093));
#68675=CARTESIAN_POINT('Ctrl Pts',(6.37546471714856,3.82553780445514,116.252166664698));
#68676=CARTESIAN_POINT('Ctrl Pts',(2.92810128566636,7.32628976968374,116.464035424303));
#68677=CARTESIAN_POINT('Ctrl Pts',(-3.80474654392298,7.55564598690843,116.728871373809));
#68678=CARTESIAN_POINT('Ctrl Pts',(-8.41256241413094,0.883863571327154,
117.046674513217));
#68679=CARTESIAN_POINT('Ctrl Pts',(-5.29871403514028,-6.58590263152199,
117.364477652625));
#68680=CARTESIAN_POINT('Ctrl Pts',(2.66452029897814,-8.02824717860013,117.682280792032));
#68681=CARTESIAN_POINT('Ctrl Pts',(8.19504584213313,-2.09883448330634,118.00008393144));
#68682=CARTESIAN_POINT('Ctrl Pts',(6.52948708872176,4.42878056429865,118.264919880946));
#68683=CARTESIAN_POINT('Ctrl Pts',(2.37182364000149,7.04668308310025,118.476788640552));
#68684=CARTESIAN_POINT('Ctrl Pts',(-2.52262267500035,7.47560524426402,118.688657400157));
#68685=CARTESIAN_POINT('Ctrl Pts',(-7.79625737144515,3.28363419722211,118.953493349663));
#68686=CARTESIAN_POINT('Ctrl Pts',(-6.97667148852008,-4.78314500361829,
119.271296489071));
#68687=CARTESIAN_POINT('Ctrl Pts',(0.237993424663934,-8.44948773760265,
119.589099628479));
#68688=CARTESIAN_POINT('Ctrl Pts',(7.23484662668109,-4.38285471727832,119.906902767886));
#68689=CARTESIAN_POINT('Ctrl Pts',(7.59906568335794,3.71726825545198,120.224705907294));
#68690=CARTESIAN_POINT('Ctrl Pts',(2.09783208782094,7.6057477909672,120.4895418568));
#68691=CARTESIAN_POINT('Ctrl Pts',(-2.76471087619419,6.90200431932459,120.701410616405));
#68692=CARTESIAN_POINT('Ctrl Pts',(-6.76842455398081,4.0542234750396,120.913279376011));
#68693=CARTESIAN_POINT('Ctrl Pts',(-8.06391256472688,-2.55679422156329,
121.178115325517));
#68694=CARTESIAN_POINT('Ctrl Pts',(-2.20839731887642,-8.16550074804653,
121.495918464925));
#68695=CARTESIAN_POINT('Ctrl Pts',(5.66102414021502,-6.2772039621143,121.813721604332));
#68696=CARTESIAN_POINT('Ctrl Pts',(8.34947323976075,1.35599329013339,122.13152474374));
#68697=CARTESIAN_POINT('Ctrl Pts',(3.37341782485002,7.75783054223044,122.449327883148));
#68698=CARTESIAN_POINT('Ctrl Pts',(-3.33584522554693,7.14985563208721,122.714163832654));
#68699=CARTESIAN_POINT('Ctrl Pts',(-6.58069071046394,3.46060682917539,122.926032592259));
#68700=CARTESIAN_POINT('Ctrl Pts',(-7.78131162404423,-1.30364425285691,
123.137901351864));
#68701=CARTESIAN_POINT('Ctrl Pts',(-4.47986753731459,-7.17597863647143,
123.402737301371));
#68702=CARTESIAN_POINT('Ctrl Pts',(3.61471026720376,-7.64763302391918,123.720540440778));
#68703=CARTESIAN_POINT('Ctrl Pts',(8.38008606205693,-1.1066352111694,124.038343580186));
#68704=CARTESIAN_POINT('Ctrl Pts',(5.47600255365382,6.44715574627637,124.356146719594));
#68705=CARTESIAN_POINT('Ctrl Pts',(-2.46353150501837,8.09289163814524,124.673949859001));
#68706=CARTESIAN_POINT('Ctrl Pts',(-7.17616749093923,3.27885941608981,124.938785808508));
#68707=CARTESIAN_POINT('Ctrl Pts',(-7.25342616325499,-1.63373766166086,
125.150654568113));
#68708=CARTESIAN_POINT('Ctrl Pts',(-5.07748184492967,-6.0388307678642,125.362523327718));
#68709=CARTESIAN_POINT('Ctrl Pts',(1.24397087744539,-8.36758143067917,125.627359277224));
#68710=CARTESIAN_POINT('Ctrl Pts',(7.71126387316832,-3.47689957616502,125.945162416632));
#68711=CARTESIAN_POINT('Ctrl Pts',(7.0964285749799,4.59251405858379,126.26296555604));
#68712=CARTESIAN_POINT('Ctrl Pts',(-0.01306199897006,8.45885633927841,126.580768695447));
#68713=CARTESIAN_POINT('Ctrl Pts',(-7.12378344817752,4.56241075819036,126.898571834855));
#68714=CARTESIAN_POINT('Ctrl Pts',(-7.58881792994159,-2.15827277115052,
127.163407784361));
#68715=CARTESIAN_POINT('Ctrl Pts',(-4.46158744940634,-5.94773295333789,
127.375276543967));
#68716=CARTESIAN_POINT('Ctrl Pts',(0.0515897489622841,-7.88959044731065,
127.587145303571));
#68717=CARTESIAN_POINT('Ctrl Pts',(6.373630862723,-5.56243761032195,127.851981253078));
#68718=CARTESIAN_POINT('Ctrl Pts',(8.12455869827376,2.35456304707941,128.169784392486));
#68719=CARTESIAN_POINT('Ctrl Pts',(2.42318628164524,8.09806471587669,128.487587531893));
#68720=CARTESIAN_POINT('Ctrl Pts',(-5.49588753251821,6.43021317020505,128.805390671301));
#68721=CARTESIAN_POINT('Ctrl Pts',(-8.38138462357639,-1.14728999588441,
129.123193810709));
#68722=CARTESIAN_POINT('Ctrl Pts',(-4.37669547353614,-6.56451336051821,
129.388029760215));
#68723=CARTESIAN_POINT('Ctrl Pts',(0.461313230403254,-7.420813968587,129.59989851982));
#68724=CARTESIAN_POINT('Ctrl Pts',(5.15601967593785,-5.97191426845995,129.811767279426));
#68725=CARTESIAN_POINT('Ctrl Pts',(8.45894789369403,-0.100414514637539,
130.076603228932));
#68726=CARTESIAN_POINT('Ctrl Pts',(4.65718588468659,7.06137669437366,130.39440636834));
#68727=CARTESIAN_POINT('Ctrl Pts',(-3.40748264062172,7.73560249443716,130.712209507747));
#68728=CARTESIAN_POINT('Ctrl Pts',(-8.35362120749351,1.33020070142903,131.030012647155));
#68729=CARTESIAN_POINT('Ctrl Pts',(-5.63564613659342,-6.30899161245907,
131.347815786563));
#68730=CARTESIAN_POINT('Ctrl Pts',(0.925940587278862,-7.83523662420755,
131.612651736069));
#68731=CARTESIAN_POINT('Ctrl Pts',(5.16386922553399,-5.34936860521914,131.824520495674));
#68732=CARTESIAN_POINT('Ctrl Pts',(7.7976944621173,-1.20177369082486,132.036389255279));
#68733=CARTESIAN_POINT('Ctrl Pts',(6.50387743193635,5.40957123008177,132.301225204786));
#68734=CARTESIAN_POINT('Ctrl Pts',(-1.03467581762238,8.39534794614227,132.619028344193));
#68735=CARTESIAN_POINT('Ctrl Pts',(-7.61057914893361,3.67825623303999,132.936831483601));
#68736=CARTESIAN_POINT('Ctrl Pts',(-7.22127632069979,-4.4051775769506,133.254634623009));
#68737=CARTESIAN_POINT('Ctrl Pts',(-0.198060572421381,-8.45722499125046,
133.572437762416));
#68738=CARTESIAN_POINT('Ctrl Pts',(5.78630429757597,-5.36348594706348,133.837273711923));
#68739=CARTESIAN_POINT('Ctrl Pts',(7.3999207693856,-0.722815647130796,134.049142471528));
#68740=CARTESIAN_POINT('Ctrl Pts',(6.71482719261795,4.14238997461265,134.261011231133));
#68741=CARTESIAN_POINT('Ctrl Pts',(1.4422521881325,8.33569380248617,134.525847180639));
#68742=CARTESIAN_POINT('Ctrl Pts',(-6.23232815901695,5.71931000232475,134.843650320047));
#68743=CARTESIAN_POINT('Ctrl Pts',(-8.17850859011008,-2.13599652143357,
135.161453459455));
#68744=CARTESIAN_POINT('Ctrl Pts',(-2.63971352946167,-8.03643787176537,
135.479256598862));
#68745=CARTESIAN_POINT('Ctrl Pts',(5.33412794588531,-6.56589381576526,135.79705973827));
#68746=CARTESIAN_POINT('Ctrl Pts',(7.88285957603773,-0.329884575213671,
136.061895687776));
#68747=CARTESIAN_POINT('Ctrl Pts',(6.10142549966758,4.24898772943948,136.273764447381));
#68748=CARTESIAN_POINT('Ctrl Pts',(2.42464571030607,7.50795525479395,136.485633206987));
#68749=CARTESIAN_POINT('Ctrl Pts',(-4.30825987416497,7.2803007767289,136.750469156493));
#68750=CARTESIAN_POINT('Ctrl Pts',(-8.45313029862189,0.311463222368526,
137.068272295901));
#68751=CARTESIAN_POINT('Ctrl Pts',(-4.84000141151651,-6.92999785242384,
137.386075435308));
#68752=CARTESIAN_POINT('Ctrl Pts',(3.20269938910426,-7.82912113888902,137.703878574716));
#68753=CARTESIAN_POINT('Ctrl Pts',(8.31848851820898,-1.53838594488056,138.021681714124));
#68754=CARTESIAN_POINT('Ctrl Pts',(6.21419397381502,4.86128503425738,138.28651766363));
#68755=CARTESIAN_POINT('Ctrl Pts',(1.88860523510587,7.19127666821767,138.498386423235));
#68756=CARTESIAN_POINT('Ctrl Pts',(-3.02365949204008,7.28737141942756,138.71025518284));
#68757=CARTESIAN_POINT('Ctrl Pts',(-8.00094636172687,2.74749701724112,138.975091132347));
#68758=CARTESIAN_POINT('Ctrl Pts',(-6.63632369986131,-5.24515289910853,
139.292894271754));
#68759=CARTESIAN_POINT('Ctrl Pts',(0.810315866115488,-8.41390944182324,
139.610697411162));
#68760=CARTESIAN_POINT('Ctrl Pts',(7.51535391249767,-3.88225150579835,139.928500550569));
#68761=CARTESIAN_POINT('Ctrl Pts',(7.32955153748415,4.22392670418686,140.246303689978));
#68762=CARTESIAN_POINT('Ctrl Pts',(1.57733990126167,7.73047849517612,140.511139639483));
#68763=CARTESIAN_POINT('Ctrl Pts',(-3.22630085224598,6.69867693382198,140.723008399089));
#68764=CARTESIAN_POINT('Ctrl Pts',(-7.0277240929022,3.58599958206011,140.934877158694));
#68765=CARTESIAN_POINT('Ctrl Pts',(-7.87200821982235,-3.09763928339454,
141.1997131082));
#68766=CARTESIAN_POINT('Ctrl Pts',(-1.64969981275852,-8.29643970098937,
141.517516247608));
#68767=CARTESIAN_POINT('Ctrl Pts',(6.07358854532228,-5.87894600079035,141.835319387016));
#68768=CARTESIAN_POINT('Ctrl Pts',(8.23832537682881,1.91896226379478,142.153122526423));
#68769=CARTESIAN_POINT('Ctrl Pts',(2.83967936581918,7.96869522834969,142.470925665831));
#68770=CARTESIAN_POINT('Ctrl Pts',(-3.81292517333676,6.9072353768361,142.735761615337));
#68771=CARTESIAN_POINT('Ctrl Pts',(-6.80017538638254,3.00647710241965,142.947630374943));
#68772=CARTESIAN_POINT('Ctrl Pts',(-7.67502034808243,-1.82821267498914,
143.159499134547));
#68773=CARTESIAN_POINT('Ctrl Pts',(-3.98303231037213,-7.46319878855479,
143.424335084054));
#68774=CARTESIAN_POINT('Ctrl Pts',(4.12489754031804,-7.38496049186462,143.742138223462));
#68775=CARTESIAN_POINT('Ctrl Pts',(8.43583245558475,-0.535924135632676,
144.059941362869));
#68776=CARTESIAN_POINT('Ctrl Pts',(5.02628893808761,6.80359027978314,144.377744502277));
#68777=CARTESIAN_POINT('Ctrl Pts',(-3.00655593015018,7.90724376650081,144.695547641685));
#68778=CARTESIAN_POINT('Ctrl Pts',(-7.38195959663264,2.78477493533829,144.960383591191));
#68779=CARTESIAN_POINT('Ctrl Pts',(-7.12596943535156,-2.12175622080281,
145.172252350796));
#68780=CARTESIAN_POINT('Ctrl Pts',(-4.65636941776872,-6.36918540902089,
145.384121110401));
#68781=CARTESIAN_POINT('Ctrl Pts',(1.80842534117273,-8.26398695045161,145.648957059908));
#68782=CARTESIAN_POINT('Ctrl Pts',(7.92925171044218,-2.94608019540264,145.966760199315));
#68783=CARTESIAN_POINT('Ctrl Pts',(6.76872988120031,5.06308005923279,146.284563338723));
#68784=CARTESIAN_POINT('Ctrl Pts',(-0.586537195444585,8.43850669521212,
146.602366478131));
#68785=CARTESIAN_POINT('Ctrl Pts',(-7.41672008904618,4.06892440513404,146.920169617539));
#68786=CARTESIAN_POINT('Ctrl Pts',(-7.42502628740076,-2.66782372811747,
147.185005567045));
#68787=CARTESIAN_POINT('Ctrl Pts',(-4.04806860277639,-6.23653993682789,
147.39687432665));
#68788=CARTESIAN_POINT('Ctrl Pts',(0.586380456386066,-7.86793857988935,
147.608743086255));
#68789=CARTESIAN_POINT('Ctrl Pts',(6.73609474152045,-5.11750997130243,147.873579035761));
#68790=CARTESIAN_POINT('Ctrl Pts',(7.9462260902675,2.89998509101313,148.191382175169));
#68791=CARTESIAN_POINT('Ctrl Pts',(1.86856641345216,8.2437216336388,148.509185314577));
#68792=CARTESIAN_POINT('Ctrl Pts',(-5.91920538067212,6.04279884965457,148.826988453984));
#68793=CARTESIAN_POINT('Ctrl Pts',(-8.28431422065509,-1.71290189729374,
149.144791593392));
#68794=CARTESIAN_POINT('Ctrl Pts',(-3.92155298584147,-6.84614703813004,
149.409627542898));
#68795=CARTESIAN_POINT('Ctrl Pts',(0.963376180029544,-7.3724596885991,149.621496302504));
#68796=CARTESIAN_POINT('Ctrl Pts',(5.54905295979434,-5.60860275371463,149.833365062109));
#68797=CARTESIAN_POINT('Ctrl Pts',(8.44628041647932,0.473338570214859,150.098201011615));
#68798=CARTESIAN_POINT('Ctrl Pts',(4.16773148534924,7.36086489439583,150.416004151023));
#68799=CARTESIAN_POINT('Ctrl Pts',(-3.92414558494879,7.48680986493268,150.733807290431));
#68800=CARTESIAN_POINT('Ctrl Pts',(-8.42452068060102,0.760708132485531,
151.051610429838));
#68801=CARTESIAN_POINT('Ctrl Pts',(-5.1950624265719,-6.67644604184268,151.369413569246));
#68802=CARTESIAN_POINT('Ctrl Pts',(1.45526099684437,-7.75464208274247,151.634249518752));
#68803=CARTESIAN_POINT('Ctrl Pts',(5.51436814750265,-4.98666840110588,151.846118278357));
#68804=CARTESIAN_POINT('Ctrl Pts',(7.86196849621255,-0.671020980375969,
152.057987037962));
#68805=CARTESIAN_POINT('Ctrl Pts',(6.12058015872781,5.83955124144195,152.322822987469));
#68806=CARTESIAN_POINT('Ctrl Pts',(-1.59886355244496,8.30341385629451,152.640626126877));
#68807=CARTESIAN_POINT('Ctrl Pts',(-7.84728433526637,3.1583187843365,152.958429266284));
#68808=CARTESIAN_POINT('Ctrl Pts',(-6.89665240705195,-4.89327593653704,
153.276232405692));
#68809=CARTESIAN_POINT('Ctrl Pts',(-0.853023022284405,-7.84339939259971,
153.541068355198));
#68810=CARTESIAN_POINT('Ctrl Pts',(3.85308616354897,-6.36807934659861,153.752940555492));
#68811=CARTESIAN_POINT('Ctrl Pts',(5.575743272665,-4.63562593309149,153.858878375984));
#68812=CARTESIAN_POINT('Ctrl Pts',(6.17613128330911,-3.60784117027914,153.911849006574));
#68813=CARTESIAN_POINT('Ctrl Pts',(3.92189707255582,-5.50607442349664,0.00384848156121544));
#68814=CARTESIAN_POINT('Ctrl Pts',(4.83912110844101,-4.85277318818901,0.0568724131943062));
#68815=CARTESIAN_POINT('Ctrl Pts',(6.32345378264837,-3.08238468302881,0.162863534728675));
#68816=CARTESIAN_POINT('Ctrl Pts',(7.30927705068616,1.47456590514539,0.374789036065603));
#68817=CARTESIAN_POINT('Ctrl Pts',(4.01501554670995,6.91028183275668,0.639624985571995));
#68818=CARTESIAN_POINT('Ctrl Pts',(-3.64467828148407,7.11551430628303,0.95742812497967));
#68819=CARTESIAN_POINT('Ctrl Pts',(-7.95222266353516,0.793792895267176,
1.27523126438734));
#68820=CARTESIAN_POINT('Ctrl Pts',(-4.97212509168922,-6.26086721103317,
1.59303440379501));
#68821=CARTESIAN_POINT('Ctrl Pts',(1.30485300361989,-7.34234073945092,1.85787035330141));
#68822=CARTESIAN_POINT('Ctrl Pts',(5.16576429400649,-4.76316292789717,2.06973911290652));
#68823=CARTESIAN_POINT('Ctrl Pts',(7.42341252941831,-0.705627305158844,
2.28160787251164));
#68824=CARTESIAN_POINT('Ctrl Pts',(5.83908213869992,5.46142515952503,2.54644382201803));
#68825=CARTESIAN_POINT('Ctrl Pts',(-1.43744337681211,7.86414290590199,2.8642469614257));
#68826=CARTESIAN_POINT('Ctrl Pts',(-7.38275336158889,3.05231572299541,3.18205010083337));
#68827=CARTESIAN_POINT('Ctrl Pts',(-6.57124549684319,-4.5530973272568,3.49985324024105));
#68828=CARTESIAN_POINT('Ctrl Pts',(0.277803164040553,-7.99030393413117,
3.81765637964872));
#68829=CARTESIAN_POINT('Ctrl Pts',(5.75410874632856,-4.74254802380421,4.08249232915512));
#68830=CARTESIAN_POINT('Ctrl Pts',(7.02157291719532,-0.275386851147049,
4.29436108876022));
#68831=CARTESIAN_POINT('Ctrl Pts',(6.10786722962805,4.27731130384919,4.50622984836535));
#68832=CARTESIAN_POINT('Ctrl Pts',(0.90276317339467,7.94401173023616,4.77106579787173));
#68833=CARTESIAN_POINT('Ctrl Pts',(-6.19447961726102,5.05375776909775,5.08886893727942));
#68834=CARTESIAN_POINT('Ctrl Pts',(-7.59909807827523,-2.46469341659131,
5.40667207668708));
#68835=CARTESIAN_POINT('Ctrl Pts',(-2.04901701299504,-7.72745660686897,
5.72447521609476));
#68836=CARTESIAN_POINT('Ctrl Pts',(5.39353975456735,-5.9018657915656,6.04227835550243));
#68837=CARTESIAN_POINT('Ctrl Pts',(7.45564034162571,0.121878774205148,6.30711430500882));
#68838=CARTESIAN_POINT('Ctrl Pts',(5.5232612325937,4.34418463217063,6.51898306461393));
#68839=CARTESIAN_POINT('Ctrl Pts',(1.87513732783761,7.2170136964436,6.73085182421905));
#68840=CARTESIAN_POINT('Ctrl Pts',(-4.46488187821364,6.63227883343294,6.99568777372545));
#68841=CARTESIAN_POINT('Ctrl Pts',(-7.99268121358921,-0.170593163642286,
7.31349091313311));
#68842=CARTESIAN_POINT('Ctrl Pts',(-4.18579272791893,-6.80442075922423,
7.6312940525408));
#68843=CARTESIAN_POINT('Ctrl Pts',(3.45193553577881,-7.21083879562565,7.94909719194845));
#68844=CARTESIAN_POINT('Ctrl Pts',(7.93305976229589,-0.994412074459289,
8.26690033135614));
#68845=CARTESIAN_POINT('Ctrl Pts',(5.59601594140876,4.92808607679508,8.53173628086252));
#68846=CARTESIAN_POINT('Ctrl Pts',(1.38678064839306,6.88877305814278,8.74360504046765));
#68847=CARTESIAN_POINT('Ctrl Pts',(-3.25324393373007,6.70953282295394,8.95547380007275));
#68848=CARTESIAN_POINT('Ctrl Pts',(-7.69989228592105,2.15266146016066,9.22030974957918));
#68849=CARTESIAN_POINT('Ctrl Pts',(-5.9732055492464,-5.31346125678687,9.53811288898681));
#68850=CARTESIAN_POINT('Ctrl Pts',(1.22684194597112,-7.89403961704749,9.85591602839451));
#68851=CARTESIAN_POINT('Ctrl Pts',(7.30408302773333,-3.24998864384153,10.1737191678022));
#68852=CARTESIAN_POINT('Ctrl Pts',(6.68338086465625,4.38801923353478,10.4915223072099));
#68853=CARTESIAN_POINT('Ctrl Pts',(1.06347372757189,7.3804099091378,10.7563582567163));
#68854=CARTESIAN_POINT('Ctrl Pts',(-3.41209097832941,6.14296263768009,10.9682270163214));
#68855=CARTESIAN_POINT('Ctrl Pts',(-6.82772436023289,2.99726656419267,11.1800957759264));
#68856=CARTESIAN_POINT('Ctrl Pts',(-7.25707551891202,-3.35516728178466,
11.4449317254329));
#68857=CARTESIAN_POINT('Ctrl Pts',(-1.10064870702956,-7.91837278010439,
11.7627348648406));
#68858=CARTESIAN_POINT('Ctrl Pts',(6.05347976412343,-5.21309748436201,12.0805380042483));
#68859=CARTESIAN_POINT('Ctrl Pts',(7.66746027614776,2.26320745285952,12.3983411436559));
#68860=CARTESIAN_POINT('Ctrl Pts',(2.24140798450443,7.67452818243227,12.7161442830636));
#68861=CARTESIAN_POINT('Ctrl Pts',(-3.97703306998174,6.30750622325713,12.9809802325699));
#68862=CARTESIAN_POINT('Ctrl Pts',(-6.58118903448087,2.46298715074713,13.1928489921751));
#68863=CARTESIAN_POINT('Ctrl Pts',(-7.14096562836087,-2.14663380452386,
13.4047177517802));
#68864=CARTESIAN_POINT('Ctrl Pts',(-3.34794148307743,-7.26041186172221,
13.6695537012866));
#68865=CARTESIAN_POINT('Ctrl Pts',(4.29762922081813,-6.74110066245508,13.9873568406943));
#68866=CARTESIAN_POINT('Ctrl Pts',(7.98869370380649,-0.0421371911454969,
14.3051599801019));
#68867=CARTESIAN_POINT('Ctrl Pts',(4.36850138181588,6.695390260325,14.6229631195097));
#68868=CARTESIAN_POINT('Ctrl Pts',(-3.27116574347611,7.29532502734838,14.9407662589173));
#68869=CARTESIAN_POINT('Ctrl Pts',(-7.11792364148947,2.22184379065709,15.2056022084237));
#68870=CARTESIAN_POINT('Ctrl Pts',(-6.6068046863944,-2.39342571394088,15.4174709680288));
#68871=CARTESIAN_POINT('Ctrl Pts',(-4.04334911920576,-6.26520188791823,
15.6293397276339));
#68872=CARTESIAN_POINT('Ctrl Pts',(2.16032533671653,-7.69774558007002,15.8941756771403));
#68873=CARTESIAN_POINT('Ctrl Pts',(7.64315926909541,-2.34396489910217,16.211978816548));
#68874=CARTESIAN_POINT('Ctrl Pts',(6.10813545411811,5.14894978711782,16.5297819559557));
#68875=CARTESIAN_POINT('Ctrl Pts',(-1.01705723707682,7.92954283912332,16.8475850953633));
#68876=CARTESIAN_POINT('Ctrl Pts',(-7.22127835658967,3.43153485667809,17.165388234771));
#68877=CARTESIAN_POINT('Ctrl Pts',(-6.85896236183368,-2.92507471957642,
17.4302241842774));
#68878=CARTESIAN_POINT('Ctrl Pts',(-3.4767027056567,-6.10662698294204,17.6420929438824));
#68879=CARTESIAN_POINT('Ctrl Pts',(0.985559249797878,-7.39121774549323,
17.8539617034876));
#68880=CARTESIAN_POINT('Ctrl Pts',(6.63672015772432,-4.45827748396203,18.118797652994));
#68881=CARTESIAN_POINT('Ctrl Pts',(7.33796046741645,3.17275767111442,18.4366007924016));
#68882=CARTESIAN_POINT('Ctrl Pts',(1.3100472228219,7.88065853276818,18.7544039318094));
#68883=CARTESIAN_POINT('Ctrl Pts',(-5.91682194971578,5.37617643649685,19.072207071217));
#68884=CARTESIAN_POINT('Ctrl Pts',(-7.72217209282292,-2.07131618657662,
19.3900102106246));
#68885=CARTESIAN_POINT('Ctrl Pts',(-3.32384119939761,-6.6748413072779,19.6548461601311));
#68886=CARTESIAN_POINT('Ctrl Pts',(1.31403441604731,-6.90301878642667,19.8667149197362));
#68887=CARTESIAN_POINT('Ctrl Pts',(5.54371861830293,-4.98684375905617,20.0785836793414));
#68888=CARTESIAN_POINT('Ctrl Pts',(7.94310832364928,0.910671584447784,20.3434196288477));
#68889=CARTESIAN_POINT('Ctrl Pts',(3.52780997821278,7.1740234052172,20.6612227682555));
#68890=CARTESIAN_POINT('Ctrl Pts',(-4.11378057803941,6.84819771851404,20.9790259076631));
#68891=CARTESIAN_POINT('Ctrl Pts',(-7.99043692094834,0.254897770346762,
21.2968290470708));
#68892=CARTESIAN_POINT('Ctrl Pts',(-4.53459677443546,-6.5848101467868,21.6146321864784));
#68893=CARTESIAN_POINT('Ctrl Pts',(1.79890132903279,-7.23639280336275,21.8794681359848));
#68894=CARTESIAN_POINT('Ctrl Pts',(5.4771274989967,-4.40220730680084,22.0913368955899));
#68895=CARTESIAN_POINT('Ctrl Pts',(7.45393977391325,-0.200520929158071,
22.3032056551951));
#68896=CARTESIAN_POINT('Ctrl Pts',(5.45549800092228,5.84464148925155,22.5680416047014));
#68897=CARTESIAN_POINT('Ctrl Pts',(-1.96738686567052,7.74864142813236,22.8858447441091));
#68898=CARTESIAN_POINT('Ctrl Pts',(-7.57267517394138,2.54471871649641,23.2036478835168));
#68899=CARTESIAN_POINT('Ctrl Pts',(-6.24744706111155,-4.98813194288109,
23.5214510229244));
#68900=CARTESIAN_POINT('Ctrl Pts',(0.818913163983748,-7.95309209086637,
23.8392541623321));
#68901=CARTESIAN_POINT('Ctrl Pts',(6.06240479820683,-4.34150605882739,24.1040901118385));
#68902=CARTESIAN_POINT('Ctrl Pts',(7.02408938913868,0.20130341702492,24.3159588714437));
#68903=CARTESIAN_POINT('Ctrl Pts',(5.80381212343591,4.68158003584414,24.5278276310488));
#68904=CARTESIAN_POINT('Ctrl Pts',(0.362087741070216,7.98693840239888,24.7926635805551));
#68905=CARTESIAN_POINT('Ctrl Pts',(-6.52286811072147,4.62214740906376,25.1104667199629));
#68906=CARTESIAN_POINT('Ctrl Pts',(-7.41450740655606,-2.97423646575735,
25.4282698593705));
#68907=CARTESIAN_POINT('Ctrl Pts',(-1.5203855076761,-7.84859751605537,25.7460729987782));
#68908=CARTESIAN_POINT('Ctrl Pts',(5.78127203409363,-5.52260683407338,26.0638761381858));
#68909=CARTESIAN_POINT('Ctrl Pts',(7.43022137695885,0.627086186692075,26.3287120876923));
#68910=CARTESIAN_POINT('Ctrl Pts',(5.21601903740572,4.70866225309671,26.5405808472972));
#68911=CARTESIAN_POINT('Ctrl Pts',(1.38151348805886,7.32754032936478,26.7524496069024));
#68912=CARTESIAN_POINT('Ctrl Pts',(-4.90427248829062,6.31430153988095,27.0172855564088));
#68913=CARTESIAN_POINT('Ctrl Pts',(-7.96272374104042,-0.712099490839074,
27.3350886958166));
#68914=CARTESIAN_POINT('Ctrl Pts',(-3.7148255683103,-7.07255778577618,27.6528918352242));
#68915=CARTESIAN_POINT('Ctrl Pts',(3.93288297675611,-6.96020736416123,27.9706949746319));
#68916=CARTESIAN_POINT('Ctrl Pts',(7.98222611578696,-0.454267335822995,
28.2884981140396));
#68917=CARTESIAN_POINT('Ctrl Pts',(5.24901816070196,5.29615286267089,28.553334063546));
#68918=CARTESIAN_POINT('Ctrl Pts',(0.916535055346602,6.96694468936257,28.7652028231511));
#68919=CARTESIAN_POINT('Ctrl Pts',(-3.70066033372871,6.47352607861612,28.9770715827562));
#68920=CARTESIAN_POINT('Ctrl Pts',(-7.82812375889614,1.62566017093144,29.2419075322626));
#68921=CARTESIAN_POINT('Ctrl Pts',(-5.59921164576593,-5.70621450761371,
29.5597106716702));
#68922=CARTESIAN_POINT('Ctrl Pts',(1.75922998076748,-7.79269610025208,29.877513811078));
#68923=CARTESIAN_POINT('Ctrl Pts',(7.50762337597611,-2.74729800085093,30.1953169504856));
#68924=CARTESIAN_POINT('Ctrl Pts',(6.37049722937737,4.83105139968957,30.5131200898933));
#68925=CARTESIAN_POINT('Ctrl Pts',(0.560639395885922,7.43553026111364,30.7779560393996));
#68926=CARTESIAN_POINT('Ctrl Pts',(-3.82072875711326,5.89748985390262,30.9898247990048));
#68927=CARTESIAN_POINT('Ctrl Pts',(-7.01522642047157,2.52745426579268,31.2016935586098));
#68928=CARTESIAN_POINT('Ctrl Pts',(-7.01289852442548,-3.83947221139287,
31.4665295081164));
#68929=CARTESIAN_POINT('Ctrl Pts',(-0.561255283071585,-7.97477570645133,
31.7843326475239));
#68930=CARTESIAN_POINT('Ctrl Pts',(6.39299535422847,-4.79067980947678,32.1021357869317));
#68931=CARTESIAN_POINT('Ctrl Pts',(7.49637318042916,2.77784884411021,32.4199389263393));
#68932=CARTESIAN_POINT('Ctrl Pts',(1.71592215789716,7.80883497866261,32.7377420657469));
#68933=CARTESIAN_POINT('Ctrl Pts',(-4.39552685639725,6.02335209421187,33.0025780152534));
#68934=CARTESIAN_POINT('Ctrl Pts',(-6.73303456328756,2.01111918639638,33.2144467748584));
#68935=CARTESIAN_POINT('Ctrl Pts',(-6.97899363197104,-2.62584742151247,
33.4263155344636));
#68936=CARTESIAN_POINT('Ctrl Pts',(-2.84798632628573,-7.47069384068419,
33.6911514839699));
#68937=CARTESIAN_POINT('Ctrl Pts',(4.74478274349493,-6.43421259969041,34.0089546233777));
#68938=CARTESIAN_POINT('Ctrl Pts',(7.97316839033122,0.499588286030254,34.3267577627853));
#68939=CARTESIAN_POINT('Ctrl Pts',(3.90450600749062,6.97616570176283,34.6445609021931));
#68940=CARTESIAN_POINT('Ctrl Pts',(-3.75825725591887,7.05675527238122,34.9623640416006));
#68941=CARTESIAN_POINT('Ctrl Pts',(-7.25218475873788,1.73414042721053,35.2271999911071));
#68942=CARTESIAN_POINT('Ctrl Pts',(-6.42932946840217,-2.83585567317026,
35.4390687507122));
#68943=CARTESIAN_POINT('Ctrl Pts',(-3.60926843557079,-6.52492208046566,
35.6509375103173));
#68944=CARTESIAN_POINT('Ctrl Pts',(2.67725678732941,-7.5335641412711,35.9157734598237));
#68945=CARTESIAN_POINT('Ctrl Pts',(7.78449154171594,-1.82036987942978,36.2335765992314));
#68946=CARTESIAN_POINT('Ctrl Pts',(5.74498484987571,5.55122974761572,36.551379738639));
#68947=CARTESIAN_POINT('Ctrl Pts',(-1.55233508847075,7.8423409026951,36.8691828780467));
#68948=CARTESIAN_POINT('Ctrl Pts',(-7.43731796205355,2.93404057696251,37.1869860174544));
#68949=CARTESIAN_POINT('Ctrl Pts',(-6.64486144705489,-3.38337747607327,
37.4518219669608));
#68950=CARTESIAN_POINT('Ctrl Pts',(-3.05467717095417,-6.3282937821792,37.6636907265659));
#68951=CARTESIAN_POINT('Ctrl Pts',(1.48441146870158,-7.3073900530725,37.875559486171));
#68952=CARTESIAN_POINT('Ctrl Pts',(6.92371736506755,-3.99805332938537,38.1403954356774));
#68953=CARTESIAN_POINT('Ctrl Pts',(7.10596461397305,3.66296627966264,38.4581985750851));
#68954=CARTESIAN_POINT('Ctrl Pts',(0.772728970275458,7.95134533111302,38.7760017144927));
#68955=CARTESIAN_POINT('Ctrl Pts',(-6.2677086455842,4.96264882850391,39.0938048539005));
#68956=CARTESIAN_POINT('Ctrl Pts',(-7.56396921361207,-2.59010855206421,
39.4116079933081));
#68957=CARTESIAN_POINT('Ctrl Pts',(-2.86364282132101,-6.88483671469794,
39.6764439428145));
#68958=CARTESIAN_POINT('Ctrl Pts',(1.77903121608731,-6.79804403814093,39.8883127024196));
#68959=CARTESIAN_POINT('Ctrl Pts',(5.86906731849622,-4.59950819187393,40.1001814620248));
#68960=CARTESIAN_POINT('Ctrl Pts',(7.86308805449229,1.44711396346235,40.3650174115311));
#68961=CARTESIAN_POINT('Ctrl Pts',(3.03329802360466,7.3966991395472,40.6828205509388));
#68962=CARTESIAN_POINT('Ctrl Pts',(-4.56861825567268,6.55352804755189,41.0006236903464));
#68963=CARTESIAN_POINT('Ctrl Pts',(-7.98933263266374,-0.287435463428486,
41.3184268297541));
#68964=CARTESIAN_POINT('Ctrl Pts',(-4.07771647401996,-6.87710120133864,
41.6362299691616));
#68965=CARTESIAN_POINT('Ctrl Pts',(2.28538499112399,-7.0977772745065,41.9010659186683));
#68966=CARTESIAN_POINT('Ctrl Pts',(5.76299143527295,-4.02073184001211,42.1129346782732));
#68967=CARTESIAN_POINT('Ctrl Pts',(7.45038326294484,0.305313005598657,42.3248034378785));
#68968=CARTESIAN_POINT('Ctrl Pts',(5.04668166278878,6.2010722274796,42.5896393873848));
#68969=CARTESIAN_POINT('Ctrl Pts',(-2.48821297984089,7.59742398632151,42.9074425267925));
#68970=CARTESIAN_POINT('Ctrl Pts',(-7.7277806175868,2.02544053543043,43.2252456662));
#68971=CARTESIAN_POINT('Ctrl Pts',(-5.89487924819143,-5.40022719061191,
43.5430488056078));
#68972=CARTESIAN_POINT('Ctrl Pts',(1.35624357475243,-7.87927001326201,43.8608519450155));
#68973=CARTESIAN_POINT('Ctrl Pts',(6.34280648913723,-3.9204888263474,44.1256878945219));
#68974=CARTESIAN_POINT('Ctrl Pts',(6.99427853146466,0.677069152014045,44.337556654127));
#68975=CARTESIAN_POINT('Ctrl Pts',(5.47304915659019,5.0643024915287,44.5494254137322));
#68976=CARTESIAN_POINT('Ctrl Pts',(-0.180254942171659,7.99310957836625,
44.8142613632384));
#68977=CARTESIAN_POINT('Ctrl Pts',(-6.82123757465311,4.16926528433038,45.1320645026462));
#68978=CARTESIAN_POINT('Ctrl Pts',(-7.19579503223384,-3.47009171207247,
45.4498676420539));
#68979=CARTESIAN_POINT('Ctrl Pts',(-0.98475697855021,-7.9336188939335,45.7676707814614));
#68980=CARTESIAN_POINT('Ctrl Pts',(6.14239852466531,-5.11793248686778,46.0854739208693));
#68981=CARTESIAN_POINT('Ctrl Pts',(7.37060818932517,1.12940768352659,46.3503098703756));
#68982=CARTESIAN_POINT('Ctrl Pts',(4.88477243985844,5.05147038228633,46.5621786299808));
#68983=CARTESIAN_POINT('Ctrl Pts',(0.881531863711674,7.40434523569889,46.7740473895858));
#68984=CARTESIAN_POINT('Ctrl Pts',(-5.32109339130866,5.96726551252067,47.0388833390923));
#68985=CARTESIAN_POINT('Ctrl Pts',(-7.89612140208864,-1.25032870256573,
47.3566864784998));
#68986=CARTESIAN_POINT('Ctrl Pts',(-3.2267625926084,-7.30814653705427,47.6744896179076));
#68987=CARTESIAN_POINT('Ctrl Pts',(4.39573108947547,-6.67754470220911,47.9922927573153));
#68988=CARTESIAN_POINT('Ctrl Pts',(7.99465785466138,0.0879679648973956,
48.310095896723));
#68989=CARTESIAN_POINT('Ctrl Pts',(4.87786412942484,5.63984648115765,48.5749318462293));
#68990=CARTESIAN_POINT('Ctrl Pts',(0.442071520850445,7.01305408383319,48.7868006058345));
#68991=CARTESIAN_POINT('Ctrl Pts',(-4.13104610495561,6.20772783511707,48.9986693654394));
#68992=CARTESIAN_POINT('Ctrl Pts',(-7.92032980481764,1.09117751024513,49.2635053149461));
#68993=CARTESIAN_POINT('Ctrl Pts',(-5.19944988304332,-6.07270746658381,
49.5813084543535));
#68994=CARTESIAN_POINT('Ctrl Pts',(2.28352194893603,-7.65549019624757,49.8991115937613));
#68995=CARTESIAN_POINT('Ctrl Pts',(7.67661325632821,-2.23196415153741,50.216914733169));
#68996=CARTESIAN_POINT('Ctrl Pts',(6.02829623905529,5.2518508194863,50.5347178725766));
#68997=CARTESIAN_POINT('Ctrl Pts',(0.055224972942848,7.45643192140313,50.799553822083));
#68998=CARTESIAN_POINT('Ctrl Pts',(-4.21178334616425,5.62487651929266,51.0114225816882));
#68999=CARTESIAN_POINT('Ctrl Pts',(-7.17044404886006,2.04601049320944,51.2232913412932));
#69000=CARTESIAN_POINT('Ctrl Pts',(-6.73644781118686,-4.30610769292906,
51.4881272907997));
#69001=CARTESIAN_POINT('Ctrl Pts',(-0.019278933510005,-7.99447830591245,
51.8059304302074));
#69002=CARTESIAN_POINT('Ctrl Pts',(6.70309005176943,-4.3462151803592,52.123733569615));
#69003=CARTESIAN_POINT('Ctrl Pts',(7.29078739079027,3.27970643248381,52.4415367090227));
#69004=CARTESIAN_POINT('Ctrl Pts',(1.18253956949703,7.90720511574864,52.7593398484304));
#69005=CARTESIAN_POINT('Ctrl Pts',(-4.79379220274076,5.71147818984704,53.0241757979367));
#69006=CARTESIAN_POINT('Ctrl Pts',(-6.85389432164721,1.54999594838462,53.2360445575419));
#69007=CARTESIAN_POINT('Ctrl Pts',(-6.78490394888292,-3.09297675396837,
53.4479133171469));
#69008=CARTESIAN_POINT('Ctrl Pts',(-2.33492459032621,-7.64659530336457,
53.7127492666534));
#69009=CARTESIAN_POINT('Ctrl Pts',(5.17010053259149,-6.09771396048381,54.030552406061));
#69010=CARTESIAN_POINT('Ctrl Pts',(7.92095014692118,1.03901463228617,54.3483555454688));
#69011=CARTESIAN_POINT('Ctrl Pts',(3.42254189622809,7.22483647078226,54.6661586848763));
#69012=CARTESIAN_POINT('Ctrl Pts',(-4.22805307568117,6.78570996765777,54.9839618242842));
#69013=CARTESIAN_POINT('Ctrl Pts',(-7.35307094970871,1.23845646056125,55.2487977737904));
#69014=CARTESIAN_POINT('Ctrl Pts',(-6.2222661463888,-3.26523487911977,55.4606665333956));
#69015=CARTESIAN_POINT('Ctrl Pts',(-3.15857771344953,-6.75461424688753,
55.6725352930006));
#69016=CARTESIAN_POINT('Ctrl Pts',(3.18186736487078,-7.33471285384217,55.9373712425071));
#69017=CARTESIAN_POINT('Ctrl Pts',(7.88999918493768,-1.28839742419215,56.2551743819147));
#69018=CARTESIAN_POINT('Ctrl Pts',(5.35539553065171,5.92796266405168,56.5729775213225));
#69019=CARTESIAN_POINT('Ctrl Pts',(-2.08046901415689,7.71904811114137,56.89078066073));
#69020=CARTESIAN_POINT('Ctrl Pts',(-7.61913064874144,2.42304369200314,57.2085838001378));
#69021=CARTESIAN_POINT('Ctrl Pts',(-6.40018053903285,-3.82610975586708,
57.4734197496441));
#69022=CARTESIAN_POINT('Ctrl Pts',(-2.61859385521392,-6.52083744880613,
57.6852885092493));
#69023=CARTESIAN_POINT('Ctrl Pts',(1.97643234988012,-7.18993337677778,57.8971572688543));
#69024=CARTESIAN_POINT('Ctrl Pts',(7.1788512699285,-3.51942992829707,58.1619932183609));
#69025=CARTESIAN_POINT('Ctrl Pts',(6.84126674685888,4.13631772949141,58.4797963577683));
#69026=CARTESIAN_POINT('Ctrl Pts',(0.231854579368945,7.98543963036104,58.7975994971761));
#69027=CARTESIAN_POINT('Ctrl Pts',(-6.5897510247487,4.52628285603161,59.1154026365838));
#69028=CARTESIAN_POINT('Ctrl Pts',(-7.37095656006863,-3.09698110512935,
59.4332057759915));
#69029=CARTESIAN_POINT('Ctrl Pts',(-2.39026581208361,-7.06314775038297,
59.6980417254979));
#69030=CARTESIAN_POINT('Ctrl Pts',(2.2358408232111,-6.66178434247006,59.9099104851029));
#69031=CARTESIAN_POINT('Ctrl Pts',(6.16740626982208,-4.19100545205031,60.1217792447082));
#69032=CARTESIAN_POINT('Ctrl Pts',(7.74688145075298,1.97689664978385,60.3866151942145));
#69033=CARTESIAN_POINT('Ctrl Pts',(2.52482667589181,7.58533488500591,60.704418333622));
#69034=CARTESIAN_POINT('Ctrl Pts',(-5.0024309177354,6.22869870433632,61.0222214730299));
#69035=CARTESIAN_POINT('Ctrl Pts',(-7.95146102577201,-0.828445904456495,
61.3400246124374));
#69036=CARTESIAN_POINT('Ctrl Pts',(-3.60207031321488,-7.13774348338487,
61.6578277518453));
#69037=CARTESIAN_POINT('Ctrl Pts',(2.76135119425199,-6.92649741053579,61.9226637013515));
#69038=CARTESIAN_POINT('Ctrl Pts',(6.02233378933796,-3.62075275904264,62.1345324609568));
#69039=CARTESIAN_POINT('Ctrl Pts',(7.4125397060154,0.809741874242037,62.3464012205618));
#69040=CARTESIAN_POINT('Ctrl Pts',(4.61464023676158,6.52896531321834,62.6112371700682));
#69041=CARTESIAN_POINT('Ctrl Pts',(-2.99758821023952,7.4112428095978,62.9290403094758));
#69042=CARTESIAN_POINT('Ctrl Pts',(-7.84732241841548,1.49684117312045,63.2468434488836));
#69043=CARTESIAN_POINT('Ctrl Pts',(-5.51518289857927,-5.78747031579437,
63.5646465882912));
#69044=CARTESIAN_POINT('Ctrl Pts',(1.8873324830186,-7.7691871308709,63.8824497276989));
#69045=CARTESIAN_POINT('Ctrl Pts',(6.59401825923553,-3.48142930317772,64.1472856772053));
#69046=CARTESIAN_POINT('Ctrl Pts',(6.93227964520087,1.14971898003392,64.3591544368104));
#69047=CARTESIAN_POINT('Ctrl Pts',(5.11709893677285,5.42371876736192,64.5710231964155));
#69048=CARTESIAN_POINT('Ctrl Pts',(-0.721768082922962,7.96249605402861,
64.8358591459219));
#69049=CARTESIAN_POINT('Ctrl Pts',(-7.08821535335468,3.69719598688643,65.1536622853295));
#69050=CARTESIAN_POINT('Ctrl Pts',(-6.94396724004815,-3.94997741832189,
65.4714654247371));
#69051=CARTESIAN_POINT('Ctrl Pts',(-0.444596547293857,-7.98212935068814,
65.7892685641449));
#69052=CARTESIAN_POINT('Ctrl Pts',(6.47525738213762,-4.68970515182132,66.1070717035525));
#69053=CARTESIAN_POINT('Ctrl Pts',(7.27707508471146,1.62653158826546,66.371907653059));
#69054=CARTESIAN_POINT('Ctrl Pts',(4.53104586896739,5.37103138564965,66.5837764126641));
#69055=CARTESIAN_POINT('Ctrl Pts',(0.377493384507276,7.44707496543455,66.7956451722693));
#69056=CARTESIAN_POINT('Ctrl Pts',(-5.71342634958102,5.59276782316797,67.0604811217756));
#69057=CARTESIAN_POINT('Ctrl Pts',(-7.79318070739572,-1.78280383746625,
67.3782842611832));
#69058=CARTESIAN_POINT('Ctrl Pts',(-2.72384988992859,-7.51010282307705,
67.696087400591));
#69059=CARTESIAN_POINT('Ctrl Pts',(4.83834982222698,-6.36415163700317,68.0138905399985));
#69060=CARTESIAN_POINT('Ctrl Pts',(7.97029776799309,0.62979843254267,68.3316936794063));
#69061=CARTESIAN_POINT('Ctrl Pts',(4.48426191718657,5.95758523680802,68.5965296289128));
#69062=CARTESIAN_POINT('Ctrl Pts',(-0.0344264494403155,7.02688904368688,
68.8083983885178));
#69063=CARTESIAN_POINT('Ctrl Pts',(-4.54242059014808,5.91336130961274,69.0202671481229));
#69064=CARTESIAN_POINT('Ctrl Pts',(-7.97608608657452,0.551673194826624,
69.2851030976293));
#69065=CARTESIAN_POINT('Ctrl Pts',(-4.77575998542697,-6.41125351452142,
69.6029062370369));
#69066=CARTESIAN_POINT('Ctrl Pts',(2.79730503229739,-7.48305333321018,69.9207093764445));
#69067=CARTESIAN_POINT('Ctrl Pts',(7.81027496804063,-1.70635868954371,70.2385125158524));
#69068=CARTESIAN_POINT('Ctrl Pts',(5.65835272148355,5.64848095407101,70.5563156552599));
#69069=CARTESIAN_POINT('Ctrl Pts',(-0.450443600392101,7.44301869658579,
70.8211516047665));
#69070=CARTESIAN_POINT('Ctrl Pts',(-4.58345508922149,5.32637721828354,71.0330203643715));
#69071=CARTESIAN_POINT('Ctrl Pts',(-7.29266293316989,1.55515086592525,71.2448891239765));
#69072=CARTESIAN_POINT('Ctrl Pts',(-6.42899560414404,-4.75292622588962,
71.5097250734831));
#69073=CARTESIAN_POINT('Ctrl Pts',(0.522786112825735,-7.97738993981093,
71.8275282128906));
#69074=CARTESIAN_POINT('Ctrl Pts',(6.98233683233883,-3.8817489844184,72.1453313522984));
#69075=CARTESIAN_POINT('Ctrl Pts',(7.0516489340484,3.76647052698219,72.4631344917059));
#69076=CARTESIAN_POINT('Ctrl Pts',(0.643715050988336,7.96918612069798,72.7809376311138));
#69077=CARTESIAN_POINT('Ctrl Pts',(-5.16999658185351,5.37331936552019,73.04577358062));
#69078=CARTESIAN_POINT('Ctrl Pts',(-6.94321169237049,1.08174008931842,73.2576423402253));
#69079=CARTESIAN_POINT('Ctrl Pts',(-6.5595907986434,-3.54587336298357,73.4695110998303));
#69080=CARTESIAN_POINT('Ctrl Pts',(-1.81111526918817,-7.78730395127627,
73.7343470493367));
#69081=CARTESIAN_POINT('Ctrl Pts',(5.57162165873517,-5.73315801212,74.0521501887443));
#69082=CARTESIAN_POINT('Ctrl Pts',(7.83228585815234,1.57366794318893,74.3699533281521));
#69083=CARTESIAN_POINT('Ctrl Pts',(2.92481462807732,7.44024196171124,74.6877564675598));
#69084=CARTESIAN_POINT('Ctrl Pts',(-4.67836648769833,6.48346864176512,75.0055596069673));
#69085=CARTESIAN_POINT('Ctrl Pts',(-7.42016107074263,0.737016856028769,
75.2703955564739));
#69086=CARTESIAN_POINT('Ctrl Pts',(-5.98651004441989,-3.67951228222445,
75.4822643160789));
#69087=CARTESIAN_POINT('Ctrl Pts',(-2.69349126760775,-6.95340398567554,
75.6941330756841));
#69088=CARTESIAN_POINT('Ctrl Pts',(3.67213255131463,-7.10171900127879,75.9589690251904));
#69089=CARTESIAN_POINT('Ctrl Pts',(7.95869722307977,-0.751146268374845,
76.2767721645981));
#69090=CARTESIAN_POINT('Ctrl Pts',(4.94207223697856,6.27860244049634,76.5945753040058));
#69091=CARTESIAN_POINT('Ctrl Pts',(-2.60074361304978,7.55799909062679,76.9123784434135));
#69092=CARTESIAN_POINT('Ctrl Pts',(-7.76256533177215,1.90520263087797,77.230181582821));
#69093=CARTESIAN_POINT('Ctrl Pts',(-5.80496517698946,-5.49065623539311,
77.5479847222288));
#69094=CARTESIAN_POINT('Ctrl Pts',(1.46920650516214,-7.85789503940717,77.8657878616364));
#69095=CARTESIAN_POINT('Ctrl Pts',(7.40524249463413,-3.01352847061608,78.1835910010441));
#69096=CARTESIAN_POINT('Ctrl Pts',(6.68073829681224,3.31247007627155,78.4484269505505));
#69097=CARTESIAN_POINT('Ctrl Pts',(3.12192870190511,6.29528985251686,78.6602957101557));
#69098=CARTESIAN_POINT('Ctrl Pts',(-1.40633759907391,7.3228545471876,78.8721644697607));
#69099=CARTESIAN_POINT('Ctrl Pts',(-6.88071188464259,4.07164371998688,79.1370004192671));
#69100=CARTESIAN_POINT('Ctrl Pts',(-7.14461299379745,-3.58695500756345,
79.454803558675));
#69101=CARTESIAN_POINT('Ctrl Pts',(-0.857498472942246,-7.94265880723423,
79.7726066980824));
#69102=CARTESIAN_POINT('Ctrl Pts',(6.21442707400568,-5.02921115503095,80.0904098374902));
#69103=CARTESIAN_POINT('Ctrl Pts',(7.59116134865531,2.50928490341992,80.4082129768979));
#69104=CARTESIAN_POINT('Ctrl Pts',(2.9369117728111,6.85390389418223,80.6730489264042));
#69105=CARTESIAN_POINT('Ctrl Pts',(-1.70642560514941,6.81663127064972,80.8849176860094));
#69106=CARTESIAN_POINT('Ctrl Pts',(-5.81967680521998,4.66184379221742,81.0967864456144));
#69107=CARTESIAN_POINT('Ctrl Pts',(-7.87807530250925,-1.36316764236396,
81.361622395121));
#69108=CARTESIAN_POINT('Ctrl Pts',(-3.11201529743014,-7.36392651431642,
81.6794255345284));
#69109=CARTESIAN_POINT('Ctrl Pts',(4.49846131872081,-6.601882199967,81.9972286739362));
#69110=CARTESIAN_POINT('Ctrl Pts',(7.99194390045502,0.202208465549562,82.3150318133438));
#69111=CARTESIAN_POINT('Ctrl Pts',(4.15083263104545,6.83321890882335,82.6328349527516));
#69112=CARTESIAN_POINT('Ctrl Pts',(-2.20955324892266,7.12174847300815,82.8976709022579));
#69113=CARTESIAN_POINT('Ctrl Pts',(-5.71978030542964,4.08196865298834,83.1095396618632));
#69114=CARTESIAN_POINT('Ctrl Pts',(-7.45321582548128,-0.225833154463851,
83.321408421468));
#69115=CARTESIAN_POINT('Ctrl Pts',(-5.11253250136785,-6.14689385231929,
83.5862443709747));
#69116=CARTESIAN_POINT('Ctrl Pts',(2.40704070040914,-7.62353003013413,83.9040475103822));
#69117=CARTESIAN_POINT('Ctrl Pts',(7.70573862108322,-2.10774641143824,84.22185064979));
#69118=CARTESIAN_POINT('Ctrl Pts',(5.95214038320305,5.3370478660503,84.5396537891976));
#69119=CARTESIAN_POINT('Ctrl Pts',(-1.27212963488989,7.89328694311642,84.8574569286053));
#69120=CARTESIAN_POINT('Ctrl Pts',(-6.30063152404268,3.98791539454707,85.1222928781117));
#69121=CARTESIAN_POINT('Ctrl Pts',(-7.00110202549445,-0.602432769133268,
85.3341616377169));
#69122=CARTESIAN_POINT('Ctrl Pts',(-5.52675146066759,-5.00564132632078,
85.5460303973217));
#69123=CARTESIAN_POINT('Ctrl Pts',(0.0949937285250582,-7.99457746023201,
85.8108663468282));
#69124=CARTESIAN_POINT('Ctrl Pts',(6.77638205776378,-4.24178043611775,86.128669486236));
#69125=CARTESIAN_POINT('Ctrl Pts',(7.23239620387072,3.3931471801692,86.4464726256435));
#69126=CARTESIAN_POINT('Ctrl Pts',(1.06931742661586,7.92266465920051,86.7642757650515));
#69127=CARTESIAN_POINT('Ctrl Pts',(-6.08746355568148,5.18315348356572,87.0820789044588));
#69128=CARTESIAN_POINT('Ctrl Pts',(-7.38223472031762,-1.05073180702098,
87.3469148539655));
#69129=CARTESIAN_POINT('Ctrl Pts',(-4.93837134276466,-4.99908424546743,
87.5587836135705));
#69130=CARTESIAN_POINT('Ctrl Pts',(-0.960453185032206,-7.39452205862662,
87.7706523731756));
#69131=CARTESIAN_POINT('Ctrl Pts',(5.25714652777984,-6.02367852407476,88.0354883226819));
#69132=CARTESIAN_POINT('Ctrl Pts',(7.90900773253987,1.16604105742781,88.3532914620898));
#69133=CARTESIAN_POINT('Ctrl Pts',(3.30452450769246,7.27331564103845,88.6710946014972));
#69134=CARTESIAN_POINT('Ctrl Pts',(-4.32426133656494,6.72404781021609,88.9888977409051));
#69135=CARTESIAN_POINT('Ctrl Pts',(-7.99514135649253,-0.00269548719377464,
89.3067008803125));
#69136=CARTESIAN_POINT('Ctrl Pts',(-4.93773878372982,-5.58750055926678,
89.5715368298191));
#69137=CARTESIAN_POINT('Ctrl Pts',(-0.516844500241237,-7.00794025194897,
89.7834055894242));
#69138=CARTESIAN_POINT('Ctrl Pts',(4.06460226526468,-6.25143465305058,89.9952743490292));
#69139=CARTESIAN_POINT('Ctrl Pts',(7.90824129176649,-1.17559016972185,90.2601102985357));
#69140=CARTESIAN_POINT('Ctrl Pts',(5.26392294923123,6.0169070331474,90.5779134379432));
#69141=CARTESIAN_POINT('Ctrl Pts',(-2.20174200284272,7.6794097943158,90.8957165773511));
#69142=CARTESIAN_POINT('Ctrl Pts',(-7.65237148129207,2.31371255200161,91.2135197167587));
#69143=CARTESIAN_POINT('Ctrl Pts',(-6.0839672687083,-5.18725696772707,91.5313228561664));
#69144=CARTESIAN_POINT('Ctrl Pts',(-0.134748826979324,-7.45541880445244,
91.7961588056728));
#69145=CARTESIAN_POINT('Ctrl Pts',(4.15155134782528,-5.66947759662977,92.0080275652779));
#69146=CARTESIAN_POINT('Ctrl Pts',(7.14821436328194,-2.12237089424207,92.219896324883));
#69147=CARTESIAN_POINT('Ctrl Pts',(6.78199168547343,4.23401480324719,92.4847322743895));
#69148=CARTESIAN_POINT('Ctrl Pts',(0.1045433961659,7.99381797011292,92.8025354137969));
#69149=CARTESIAN_POINT('Ctrl Pts',(-6.65635398585283,4.41746015840961,93.1203385532049));
#69150=CARTESIAN_POINT('Ctrl Pts',(-7.32535259445545,-3.2017595830866,93.4381416926121));
#69151=CARTESIAN_POINT('Ctrl Pts',(-1.26680705031046,-7.89414292201699,
93.7559448320203));
#69152=CARTESIAN_POINT('Ctrl Pts',(4.73260344551426,-5.76228178967871,94.0207807815264));
#69153=CARTESIAN_POINT('Ctrl Pts',(6.83697291209494,-1.62300838309489,94.2326495411316));
#69154=CARTESIAN_POINT('Ctrl Pts',(6.81750635060592,3.02043605388431,94.4445183007367));
#69155=CARTESIAN_POINT('Ctrl Pts',(2.41634697636828,7.62125710534312,94.7093542502432));
#69156=CARTESIAN_POINT('Ctrl Pts',(-5.10477095205658,6.15250912945454,95.0271573896507));
#69157=CARTESIAN_POINT('Ctrl Pts',(-7.931581283013,-0.954474194032004,95.3449605290586));
#69158=CARTESIAN_POINT('Ctrl Pts',(-3.49940412743684,-7.18792221812814,
95.662763668466));
#69159=CARTESIAN_POINT('Ctrl Pts',(4.15543921733351,-6.83041854405671,95.9805668078738));
#69160=CARTESIAN_POINT('Ctrl Pts',(7.33944388963318,-1.31681061169869,96.2454027573801));
#69161=CARTESIAN_POINT('Ctrl Pts',(6.25673777894657,3.19868522643596,96.4572715169854));
#69162=CARTESIAN_POINT('Ctrl Pts',(3.23043977694139,6.72054206472292,96.6691402765903));
#69163=CARTESIAN_POINT('Ctrl Pts',(-3.10345759092554,7.36823205099255,96.933976226097));
#69164=CARTESIAN_POINT('Ctrl Pts',(-7.87580893693733,1.37247537312704,97.2517793655042));
#69165=CARTESIAN_POINT('Ctrl Pts',(-5.41831594300546,-5.87050721640711,
97.5695825049123));
#69166=CARTESIAN_POINT('Ctrl Pts',(1.9980227369176,-7.74079842159345,97.8873856443198));
#69167=CARTESIAN_POINT('Ctrl Pts',(7.59285417362454,-2.50416814012545,98.2051887837274));
#69168=CARTESIAN_POINT('Ctrl Pts',(6.44062409468572,3.75763064538146,98.4700247332341));
#69169=CARTESIAN_POINT('Ctrl Pts',(2.68799327264257,6.49253779184573,98.6818934928389));
#69170=CARTESIAN_POINT('Ctrl Pts',(-1.89963529314591,7.21060417365909,98.8937622524443));
#69171=CARTESIAN_POINT('Ctrl Pts',(-7.14090626808129,3.59579619089075,99.1585982019505));
#69172=CARTESIAN_POINT('Ctrl Pts',(-6.88499375475416,-4.06311654496619,
99.4764013413583));
#69173=CARTESIAN_POINT('Ctrl Pts',(-0.317010548502199,-7.98251257113032,
99.7942044807658));
#69174=CARTESIAN_POINT('Ctrl Pts',(6.54110088345483,-4.59630876828881,100.112007620174));
#69175=CARTESIAN_POINT('Ctrl Pts',(7.40356833653495,3.01818960010868,100.429810759582));
#69176=CARTESIAN_POINT('Ctrl Pts',(2.46546225761111,7.03725249315749,100.694646709088));
#69177=CARTESIAN_POINT('Ctrl Pts',(-2.16466201497952,6.68525191546445,100.906515468693));
#69178=CARTESIAN_POINT('Ctrl Pts',(-6.12235607099368,4.25654589263679,101.118384228298));
#69179=CARTESIAN_POINT('Ctrl Pts',(-7.76752552118866,-1.89415940554908,
101.383220177805));
#69180=CARTESIAN_POINT('Ctrl Pts',(-2.60558488410996,-7.55797475999223,
101.701023317212));
#69181=CARTESIAN_POINT('Ctrl Pts',(4.93571384885182,-6.28169813333685,102.01882645662));
#69182=CARTESIAN_POINT('Ctrl Pts',(7.95984459380424,0.743592027571294,102.336629596027));
#69183=CARTESIAN_POINT('Ctrl Pts',(3.67799343791845,7.09891941400772,102.654432735435));
#69184=CARTESIAN_POINT('Ctrl Pts',(-2.68731918353641,6.95555478750277,102.919268684942));
#69185=CARTESIAN_POINT('Ctrl Pts',(-5.98337390429468,3.68477835611888,103.131137444547));
#69186=CARTESIAN_POINT('Ctrl Pts',(-7.42075443828335,-0.730636956945093,
103.343006204152));
#69187=CARTESIAN_POINT('Ctrl Pts',(-4.68401280993483,-6.4793762487074,103.607842153658));
#69188=CARTESIAN_POINT('Ctrl Pts',(2.9183726832874,-7.44279221411051,103.925645293066));
#69189=CARTESIAN_POINT('Ctrl Pts',(7.83091142925338,-1.5804520945932,104.243448432474));
#69190=CARTESIAN_POINT('Ctrl Pts',(5.57659579337766,5.72831863798309,104.561251571881));
#69191=CARTESIAN_POINT('Ctrl Pts',(-1.80436243058459,7.78887468091779,104.879054711289));
#69192=CARTESIAN_POINT('Ctrl Pts',(-6.55651181971887,3.55156015773956,105.143890660795));
#69193=CARTESIAN_POINT('Ctrl Pts',(-6.94414773901417,-1.07571696605596,
105.3557594204));
#69194=CARTESIAN_POINT('Ctrl Pts',(-5.1746548614019,-5.36883356619723,105.567628180006));
#69195=CARTESIAN_POINT('Ctrl Pts',(0.636802579013681,-7.96974121608161,
105.832464129512));
#69196=CARTESIAN_POINT('Ctrl Pts',(7.0483795328344,-3.77258545590462,106.15026726892));
#69197=CARTESIAN_POINT('Ctrl Pts',(6.98570098337924,3.87569147468288,106.468070408327));
#69198=CARTESIAN_POINT('Ctrl Pts',(0.529705109973643,7.97693346828529,106.785873547735));
#69199=CARTESIAN_POINT('Ctrl Pts',(-6.4248707633773,4.75850063043461,107.103676687143));
#69200=CARTESIAN_POINT('Ctrl Pts',(-7.29400903878353,-1.54882501861905,
107.368512636649));
#69201=CARTESIAN_POINT('Ctrl Pts',(-4.58807318727075,-5.32239976331763,
107.580381396254));
#69202=CARTESIAN_POINT('Ctrl Pts',(-0.456899111205659,-7.44262520877786,
107.792250155859));
#69203=CARTESIAN_POINT('Ctrl Pts',(5.65345139690404,-5.65338658494099,108.057086105366));
#69204=CARTESIAN_POINT('Ctrl Pts',(7.81175203655464,1.69958382563695,108.374889244773));
#69205=CARTESIAN_POINT('Ctrl Pts',(2.80379438617548,7.48062428385264,108.692692384181));
#69206=CARTESIAN_POINT('Ctrl Pts',(-4.77019740516966,6.41539334543834,109.010495523589));
#69207=CARTESIAN_POINT('Ctrl Pts',(-7.97656157879294,-0.544754950112174,
109.328298662996));
#69208=CARTESIAN_POINT('Ctrl Pts',(-4.54754781969298,-5.9094192289735,109.593134612503));
#69209=CARTESIAN_POINT('Ctrl Pts',(-0.0405211900412987,-7.02685654083492,
109.805003372108));
#69210=CARTESIAN_POINT('Ctrl Pts',(4.47909293475132,-5.9614724085595,110.016872131713));
#69211=CARTESIAN_POINT('Ctrl Pts',(7.96974851599409,-0.636711212212364,
110.281708081219));
#69212=CARTESIAN_POINT('Ctrl Pts',(4.84386793230822,6.3599527132942,110.599511220627));
#69213=CARTESIAN_POINT('Ctrl Pts',(-2.71733499765062,7.51246252214666,110.917314360035));
#69214=CARTESIAN_POINT('Ctrl Pts',(-7.79163146585404,1.78956256143654,111.235117499442));
#69215=CARTESIAN_POINT('Ctrl Pts',(-5.71827507280204,-5.58781019431744,
111.55292063885));
#69216=CARTESIAN_POINT('Ctrl Pts',(0.37103404184402,-7.44739958213263,111.817756588356));
#69217=CARTESIAN_POINT('Ctrl Pts',(4.52638561484153,-5.37495935594604,112.029625347962));
#69218=CARTESIAN_POINT('Ctrl Pts',(7.27566157962207,-1.63284272817919,112.241494107567));
#69219=CARTESIAN_POINT('Ctrl Pts',(6.47932254979134,4.68408709053455,112.506330057073));
#69220=CARTESIAN_POINT('Ctrl Pts',(-0.437673101391219,7.98251196787706,
112.824133196481));
#69221=CARTESIAN_POINT('Ctrl Pts',(-6.94053862569258,3.95599876407772,113.141936335888));
#69222=CARTESIAN_POINT('Ctrl Pts',(-7.09141944026156,-3.69104665146115,
113.459739475296));
#69223=CARTESIAN_POINT('Ctrl Pts',(-0.728674061214709,-7.96186703534172,
113.777542614704));
#69224=CARTESIAN_POINT('Ctrl Pts',(5.11239276394556,-5.42815502941039,114.04237856421));
#69225=CARTESIAN_POINT('Ctrl Pts',(6.93127983195271,-1.15573124189053,114.254247323815));
#69226=CARTESIAN_POINT('Ctrl Pts',(6.59703538737303,3.47570868944796,114.46611608342));
#69227=CARTESIAN_POINT('Ctrl Pts',(1.89407035690759,7.7675472357129,114.730952032927));
#69228=CARTESIAN_POINT('Ctrl Pts',(-5.51016107707595,5.79225171808505,115.048755172334));
#69229=CARTESIAN_POINT('Ctrl Pts',(-7.84861774789,-1.49003425585493,115.366558311742));
#69230=CARTESIAN_POINT('Ctrl Pts',(-3.00401520445511,-7.40864007172603,
115.68436145115));
#69231=CARTESIAN_POINT('Ctrl Pts',(4.60897562027904,-6.53296535331549,116.002164590558));
#69232=CARTESIAN_POINT('Ctrl Pts',(7.41183459035819,-0.816170816266582,
116.267000540064));
#69233=CARTESIAN_POINT('Ctrl Pts',(6.02547197434124,3.61552794191181,116.478869299669));
#69234=CARTESIAN_POINT('Ctrl Pts',(2.76735783469423,6.92409975454661,116.690738059274));
#69235=CARTESIAN_POINT('Ctrl Pts',(-3.595878055479,7.14086504466174,116.95557400878));
#69236=CARTESIAN_POINT('Ctrl Pts',(-7.95073948451101,0.835342271419291,
117.273377148188));
#69237=CARTESIAN_POINT('Ctrl Pts',(-5.00783148135237,-6.2243575162816,117.591180287596));
#69238=CARTESIAN_POINT('Ctrl Pts',(2.51824660614424,-7.58752193351855,117.908983427003));
#69239=CARTESIAN_POINT('Ctrl Pts',(7.74516388074322,-1.98361514321149,118.226786566411));
#69240=CARTESIAN_POINT('Ctrl Pts',(6.17103900741412,4.185654592191,118.491622515917));
#69241=CARTESIAN_POINT('Ctrl Pts',(2.24161806314621,6.65984258607461,118.703491275523));
#69242=CARTESIAN_POINT('Ctrl Pts',(-2.38413871057332,7.06521828430672,118.915360035128));
#69243=CARTESIAN_POINT('Ctrl Pts',(-7.36826762918714,3.10337311978758,119.180195984634));
#69244=CARTESIAN_POINT('Ctrl Pts',(-6.59367440544241,-4.52056555045889,
119.497999124042));
#69245=CARTESIAN_POINT('Ctrl Pts',(0.224928342326,-7.98563772512462,119.81580226345));
#69246=CARTESIAN_POINT('Ctrl Pts',(6.83767654936024,-4.14224992815635,120.133605402857));
#69247=CARTESIAN_POINT('Ctrl Pts',(7.1819011378248,3.51320204691645,120.451408542265));
#69248=CARTESIAN_POINT('Ctrl Pts',(1.98266777605119,7.188216418971,120.716244491771));
#69249=CARTESIAN_POINT('Ctrl Pts',(-2.61293703921732,6.52310622643868,120.928113251376));
#69250=CARTESIAN_POINT('Ctrl Pts',(-6.39685956550806,3.83165949626573,121.139982010982));
#69251=CARTESIAN_POINT('Ctrl Pts',(-7.62122940334152,-2.41643434787499,
121.404817960488));
#69252=CARTESIAN_POINT('Ctrl Pts',(-2.08716332745305,-7.71724071838623,
121.722621099896));
#69253=CARTESIAN_POINT('Ctrl Pts',(5.35025191358701,-5.93260542234808,122.040424239303));
#69254=CARTESIAN_POINT('Ctrl Pts',(7.89111370522805,1.28155356975195,122.358227378711));
#69255=CARTESIAN_POINT('Ctrl Pts',(3.18822791171694,7.33195031072198,122.676030518119));
#69256=CARTESIAN_POINT('Ctrl Pts',(-3.15271792865614,6.75735129014959,122.940866467625));
#69257=CARTESIAN_POINT('Ctrl Pts',(-6.21943171311898,3.27063051691363,123.15273522723));
#69258=CARTESIAN_POINT('Ctrl Pts',(-7.35414235580032,-1.23207832818336,
123.364603986835));
#69259=CARTESIAN_POINT('Ctrl Pts',(-4.23393705281535,-6.78204022464807,
123.629439936342));
#69260=CARTESIAN_POINT('Ctrl Pts',(3.41627416614999,-7.22780228580432,123.947243075749));
#69261=CARTESIAN_POINT('Ctrl Pts',(7.92004598091047,-1.04588445651475,124.265046215157));
#69262=CARTESIAN_POINT('Ctrl Pts',(5.17538742387095,6.09322739390386,124.582849354565));
#69263=CARTESIAN_POINT('Ctrl Pts',(-2.32829145794874,7.64861761776532,124.900652493972));
#69264=CARTESIAN_POINT('Ctrl Pts',(-6.78221871160612,3.09886045895844,125.165488443479));
#69265=CARTESIAN_POINT('Ctrl Pts',(-6.85523612844846,-1.5440506583436,125.377357203084));
#69266=CARTESIAN_POINT('Ctrl Pts',(-4.79874423499827,-5.70731815857739,
125.589225962689));
#69267=CARTESIAN_POINT('Ctrl Pts',(1.17568083135626,-7.90822781403826,125.854061912195));
#69268=CARTESIAN_POINT('Ctrl Pts',(7.28794000373724,-3.28602884389481,126.171865051603));
#69269=CARTESIAN_POINT('Ctrl Pts',(6.70685720861144,4.34039963821441,126.489668191011));
#69270=CARTESIAN_POINT('Ctrl Pts',(-0.0123449367553314,7.99449202035492,
126.807471330418));
#69271=CARTESIAN_POINT('Ctrl Pts',(-6.73271038624204,4.3119489133031,127.125274469826));
#69272=CARTESIAN_POINT('Ctrl Pts',(-7.17221595348917,-2.03979045803012,
127.390110419332));
#69273=CARTESIAN_POINT('Ctrl Pts',(-4.21666048361343,-5.62122132443205,
127.601979178938));
#69274=CARTESIAN_POINT('Ctrl Pts',(0.0487576357682374,-7.45647701593123,
127.813847938542));
#69275=CARTESIAN_POINT('Ctrl Pts',(6.02373879269242,-5.25707747073975,128.078683888049));
#69276=CARTESIAN_POINT('Ctrl Pts',(7.67854625697508,2.2253050218961,128.396487027457));
#69277=CARTESIAN_POINT('Ctrl Pts',(2.29016105906626,7.65350670997627,128.714290166864));
#69278=CARTESIAN_POINT('Ctrl Pts',(-5.19418078061711,6.07721491139238,129.032093306272));
#69279=CARTESIAN_POINT('Ctrl Pts',(-7.92127325553131,-1.08430742280561,
129.34989644568));
#69280=CARTESIAN_POINT('Ctrl Pts',(-4.13642880731286,-6.2041424482509,129.614732395186));
#69281=CARTESIAN_POINT('Ctrl Pts',(0.4359886007537,-7.01343487546074,129.826601154791));
#69282=CARTESIAN_POINT('Ctrl Pts',(4.87297058878657,-5.64407516223672,130.038469914396));
#69283=CARTESIAN_POINT('Ctrl Pts',(7.99457854872422,-0.0949020770426225,
130.303305863903));
#69284=CARTESIAN_POINT('Ctrl Pts',(4.40152118668289,6.67372956480586,130.62110900331));
#69285=CARTESIAN_POINT('Ctrl Pts',(-3.2204226774074,7.31094251208114,130.938912142718));
#69286=CARTESIAN_POINT('Ctrl Pts',(-7.89503396272016,1.25717691216364,131.256715282126));
#69287=CARTESIAN_POINT('Ctrl Pts',(-5.32626708167825,-5.96264803175383,
131.574518421534));
#69288=CARTESIAN_POINT('Ctrl Pts',(0.875109392973854,-7.40510704490388,
131.83935437104));
#69289=CARTESIAN_POINT('Ctrl Pts',(4.8803892230668,-5.05570527658503,132.051223130645));
#69290=CARTESIAN_POINT('Ctrl Pts',(7.36962582815063,-1.13580013612054,132.26309189025));
#69291=CARTESIAN_POINT('Ctrl Pts',(6.1468352393629,5.11260296875023,132.527927839757));
#69292=CARTESIAN_POINT('Ctrl Pts',(-0.977875404884448,7.93447003608332,
132.845730979164));
#69293=CARTESIAN_POINT('Ctrl Pts',(-7.19278255074581,3.47633166050105,133.163534118572));
#69294=CARTESIAN_POINT('Ctrl Pts',(-6.82485121003244,-4.16334733380493,
133.481337257979));
#69295=CARTESIAN_POINT('Ctrl Pts',(-0.187187676710187,-7.99295022814698,
133.799140397387));
#69296=CARTESIAN_POINT('Ctrl Pts',(5.46865458862486,-5.06904762124686,134.063976346893));
#69297=CARTESIAN_POINT('Ctrl Pts',(6.99368864646755,-0.68313536622519,134.275845106499));
#69298=CARTESIAN_POINT('Ctrl Pts',(6.34620452887703,3.91498593532799,134.487713866104));
#69299=CARTESIAN_POINT('Ctrl Pts',(1.36307712850379,7.87809071524929,134.75254981561));
#69300=CARTESIAN_POINT('Ctrl Pts',(-5.89019315816176,5.40533806718196,135.070352955018));
#69301=CARTESIAN_POINT('Ctrl Pts',(-7.72953447127796,-2.01873710359743,
135.388156094426));
#69302=CARTESIAN_POINT('Ctrl Pts',(-2.4948016494047,-7.59526298367014,135.705959233833));
#69303=CARTESIAN_POINT('Ctrl Pts',(5.04130128099164,-6.20544712089461,136.023762373241));
#69304=CARTESIAN_POINT('Ctrl Pts',(7.450115648091,-0.311774960870602,136.288598322747));
#69305=CARTESIAN_POINT('Ctrl Pts',(5.76647663861923,4.01573181233197,136.500467082352));
#69306=CARTESIAN_POINT('Ctrl Pts',(2.29154036973368,7.09579238211189,136.712335841958));
#69307=CARTESIAN_POINT('Ctrl Pts',(-4.0717501047619,6.88063541108804,136.977171791464));
#69308=CARTESIAN_POINT('Ctrl Pts',(-7.98908032112504,0.294364881727811,
137.294974930872));
#69309=CARTESIAN_POINT('Ctrl Pts',(-4.57430072233384,-6.54956300357293,
137.612778070279));
#69310=CARTESIAN_POINT('Ctrl Pts',(3.02688137531002,-7.39932728028593,137.930581209687));
#69311=CARTESIAN_POINT('Ctrl Pts',(7.8618299463764,-1.45393344765422,138.248384349095));
#69312=CARTESIAN_POINT('Ctrl Pts',(5.87305448207229,4.59441594185449,138.513220298601));
#69313=CARTESIAN_POINT('Ctrl Pts',(1.78492681233391,6.79649844309022,138.725089058206));
#69314=CARTESIAN_POINT('Ctrl Pts',(-2.85767019935493,6.88731789798286,138.936957817811));
#69315=CARTESIAN_POINT('Ctrl Pts',(-7.56171984469098,2.59666816639205,139.201793767318));
#69316=CARTESIAN_POINT('Ctrl Pts',(-6.27201062827867,-4.95721068139547,
139.519596906725));
#69317=CARTESIAN_POINT('Ctrl Pts',(0.765832101384861,-7.95201256466585,
139.837400046133));
#69318=CARTESIAN_POINT('Ctrl Pts',(7.10278487703089,-3.66912824136791,140.155203185541));
#69319=CARTESIAN_POINT('Ctrl Pts',(6.92718246166577,3.99204655768657,140.473006324948));
#69320=CARTESIAN_POINT('Ctrl Pts',(1.49074895568024,7.30609980408792,140.737842274455));
#69321=CARTESIAN_POINT('Ctrl Pts',(-3.04918719316388,6.33094086794075,140.94971103406));
#69322=CARTESIAN_POINT('Ctrl Pts',(-6.64192438416009,3.38913960633895,141.161579793665));
#69323=CARTESIAN_POINT('Ctrl Pts',(-7.43985999683126,-2.92758873537547,
141.426415743171));
#69324=CARTESIAN_POINT('Ctrl Pts',(-1.55913653809718,-7.8409915391201,141.744218882579));
#69325=CARTESIAN_POINT('Ctrl Pts',(5.74016784456189,-5.55621055687876,142.062022021987));
#69326=CARTESIAN_POINT('Ctrl Pts',(7.78606750658739,1.8136173366639,142.379825161394));
#69327=CARTESIAN_POINT('Ctrl Pts',(2.68378999711791,7.53123919599689,142.697628300802));
#69328=CARTESIAN_POINT('Ctrl Pts',(-3.60360770414117,6.52805011552451,142.962464250308));
#69329=CARTESIAN_POINT('Ctrl Pts',(-6.42686737815966,2.84143106829594,143.174333009914));
#69330=CARTESIAN_POINT('Ctrl Pts',(-7.25368613294617,-1.72784961175433,
143.386201769518));
#69331=CARTESIAN_POINT('Ctrl Pts',(-3.76437650019324,-7.05349290357036,
143.651037719025));
#69332=CARTESIAN_POINT('Ctrl Pts',(3.89845378006065,-6.97954964061808,143.968840858433));
#69333=CARTESIAN_POINT('Ctrl Pts',(7.97273207467384,-0.506503604505183,
144.28664399784));
#69334=CARTESIAN_POINT('Ctrl Pts',(4.75036165597909,6.43009480476973,144.604447137248));
#69335=CARTESIAN_POINT('Ctrl Pts',(-2.84150556863367,7.47316122402503,144.922250276656));
#69336=CARTESIAN_POINT('Ctrl Pts',(-6.97671348499278,2.63189964530712,145.187086226162));
#69337=CARTESIAN_POINT('Ctrl Pts',(-6.73477636967082,-2.00527855019573,
145.398954985767));
#69338=CARTESIAN_POINT('Ctrl Pts',(-4.40074954120288,-6.01953738026474,
145.610823745372));
#69339=CARTESIAN_POINT('Ctrl Pts',(1.70914853965251,-7.81032034140677,145.875659694879));
#69340=CARTESIAN_POINT('Ctrl Pts',(7.49396100181569,-2.78434975944821,146.193462834286));
#69341=CARTESIAN_POINT('Ctrl Pts',(6.3971481312346,4.78513306154618,146.511265973694));
#69342=CARTESIAN_POINT('Ctrl Pts',(-0.554338168251488,7.97525950704822,
146.829069113102));
#69343=CARTESIAN_POINT('Ctrl Pts',(-7.00956573689031,3.8455533920382,147.146872252509));
#69344=CARTESIAN_POINT('Ctrl Pts',(-7.01741595136444,-2.52136868752679,
147.411708202016));
#69345=CARTESIAN_POINT('Ctrl Pts',(-3.82584250692092,-5.89417372276192,
147.623576961621));
#69346=CARTESIAN_POINT('Ctrl Pts',(0.55419003366898,-7.43601376719139,147.835445721226));
#69347=CARTESIAN_POINT('Ctrl Pts',(6.36630455696223,-4.83657494449871,148.100281670732));
#69348=CARTESIAN_POINT('Ctrl Pts',(7.51000354215738,2.74078512973372,148.41808481014));
#69349=CARTESIAN_POINT('Ctrl Pts',(1.7659880582776,7.79116752605513,148.735887949548));
#69350=CARTESIAN_POINT('Ctrl Pts',(-5.59425982480493,5.71106840529436,149.053691088956));
#69351=CARTESIAN_POINT('Ctrl Pts',(-7.8295317091046,-1.61886902913507,149.371494228363));
#69352=CARTESIAN_POINT('Ctrl Pts',(-3.7062721951118,-6.47031533238849,149.63633017787));
#69353=CARTESIAN_POINT('Ctrl Pts',(0.910489890705346,-6.96773509170653,
149.848198937475));
#69354=CARTESIAN_POINT('Ctrl Pts',(5.24442759497008,-5.30070829453768,150.06006769708));
#69355=CARTESIAN_POINT('Ctrl Pts',(7.98260647573363,0.447353787642963,150.324903646586));
#69356=CARTESIAN_POINT('Ctrl Pts',(3.93893627769698,6.95677681484015,150.642706785994));
#69357=CARTESIAN_POINT('Ctrl Pts',(-3.70872246877002,7.07580780692477,150.960509925402));
#69358=CARTESIAN_POINT('Ctrl Pts',(-7.96204128017202,0.718947674609458,
151.278313064809));
#69359=CARTESIAN_POINT('Ctrl Pts',(-4.9098700165443,-6.30993038124958,151.596116204217));
#69360=CARTESIAN_POINT('Ctrl Pts',(1.37537179497646,-7.32893688752285,151.860952153723));
#69361=CARTESIAN_POINT('Ctrl Pts',(5.21164686859631,-4.71291616050793,152.072820913328));
#69362=CARTESIAN_POINT('Ctrl Pts',(7.43037142212706,-0.634184061999188,
152.284689672933));
#69363=CARTESIAN_POINT('Ctrl Pts',(5.78457976779752,5.51897844456597,152.54952562244));
#69364=CARTESIAN_POINT('Ctrl Pts',(-1.51109102684477,7.84758283547285,152.867328761848));
#69365=CARTESIAN_POINT('Ctrl Pts',(-7.41649337492981,2.98493712464134,153.185131901255));
#69366=CARTESIAN_POINT('Ctrl Pts',(-6.51804811713408,-4.62465064531089,
153.502935040663));
#69367=CARTESIAN_POINT('Ctrl Pts',(-0.806194770464466,-7.41282170326391,
153.767770990169));
#69368=CARTESIAN_POINT('Ctrl Pts',(3.64156398367868,-6.01849203715341,153.979643190462));
#69369=CARTESIAN_POINT('Ctrl Pts',(5.26965269452346,-4.3811448078825,154.085581010954));
#69370=CARTESIAN_POINT('Ctrl Pts',(5.83708131225798,-3.40978216080788,154.138551641544));
#69371=CARTESIAN_POINT('Ctrl Pts',(3.43101696651027,7.14016450787011,1.65822217068623E-14));
#69372=CARTESIAN_POINT('Ctrl Pts',(3.61003597782292,7.03974453288905,1.31692278925585E-14));
#69373=CARTESIAN_POINT('Ctrl Pts',(3.78453304467846,6.93211991481877,1.59736015986178E-14));
#69374=CARTESIAN_POINT('Ctrl Pts',(3.95400783053005,6.81726961947616,1.53627111032506E-14));
#69375=CARTESIAN_POINT('Ctrl Pts',(4.12383106727608,6.70218318465156,1.45970944988586E-14));
#69376=CARTESIAN_POINT('Ctrl Pts',(4.28861172272689,6.57984074250072,1.20659957845407E-14));
#69377=CARTESIAN_POINT('Ctrl Pts',(4.44814243011172,6.45071609426073,1.22124532708767E-14));
#69378=CARTESIAN_POINT('Ctrl Pts',(4.60928369061434,6.32028785934319,1.23603893287374E-14));
#69379=CARTESIAN_POINT('Ctrl Pts',(4.76506884842713,6.18293913020302,1.03995638427172E-14));
#69380=CARTESIAN_POINT('Ctrl Pts',(4.91524218627338,6.03912581706056,1.29757316003065E-14));
#69381=CARTESIAN_POINT('Ctrl Pts',(4.96008620607599,5.99618099639577,1.37450140814249E-14));
#69382=CARTESIAN_POINT('Ctrl Pts',(5.00442975271524,5.95265929902808,1.55276531095038E-14));
#69383=CARTESIAN_POINT('Ctrl Pts',(5.04826448447757,5.90857319066696,1.45022882591661E-14));
#69384=CARTESIAN_POINT('Ctrl Pts',(5.07244303315987,5.88425598660599,1.39367131329073E-14));
#69385=CARTESIAN_POINT('Ctrl Pts',(5.09646351320685,5.85977024716788,1.48017877861931E-14));
#69386=CARTESIAN_POINT('Ctrl Pts',(5.1203146633298,5.83512874369868,1.43218770176645E-14));
#69387=CARTESIAN_POINT('Ctrl Pts',(5.26273479984385,5.6879892443495,1.14562308406016E-14));
#69388=CARTESIAN_POINT('Ctrl Pts',(5.39923071701932,5.53518844907465,1.30927522722923E-14));
#69389=CARTESIAN_POINT('Ctrl Pts',(5.52960032490143,5.37719968636751,1.25732757538799E-14));
#69390=CARTESIAN_POINT('Ctrl Pts',(5.66063860884131,5.21840058676716,1.20511347992075E-14));
#69391=CARTESIAN_POINT('Ctrl Pts',(5.78548791527577,5.05435946905415,8.76473059902014E-15));
#69392=CARTESIAN_POINT('Ctrl Pts',(5.90389832912926,4.88552923085758,7.13318293321663E-15));
#69393=CARTESIAN_POINT('Ctrl Pts',(6.02173466768101,4.71751751247513,5.50954530832999E-15));
#69394=CARTESIAN_POINT('Ctrl Pts',(6.13319465726933,4.54476228664395,7.19754582327447E-15));
#69395=CARTESIAN_POINT('Ctrl Pts',(6.23798347774738,4.36769307789513,6.16173778666962E-15));
#69396=CARTESIAN_POINT('Ctrl Pts',(6.25387388903657,4.34084190674124,6.00466553751931E-15));
#69397=CARTESIAN_POINT('Ctrl Pts',(6.26961079874451,4.31389151400701,5.35714192551716E-15));
#69398=CARTESIAN_POINT('Ctrl Pts',(6.28519307487105,4.28684337930822,5.57887069874141E-15));
#69399=CARTESIAN_POINT('Ctrl Pts',(6.29843934789536,4.26385014172799,5.0289415732972E-15));
#69400=CARTESIAN_POINT('Ctrl Pts',(6.31156974583608,4.24079340614484,7.2115050195674E-15));
#69401=CARTESIAN_POINT('Ctrl Pts',(6.3245813935981,4.21767852568033,7.16093850883226E-15));
#69402=CARTESIAN_POINT('Ctrl Pts',(6.42415862933386,4.04078195246255,6.90070714083338E-15));
#69403=CARTESIAN_POINT('Ctrl Pts',(6.51683135396108,3.860401258507,4.02818541900997E-15));
#69404=CARTESIAN_POINT('Ctrl Pts',(6.60240201838025,3.67698384153671,4.10782519111308E-15));
#69405=CARTESIAN_POINT('Ctrl Pts',(6.68774671377467,3.4940507804507,3.96951696376866E-15));
#69406=CARTESIAN_POINT('Ctrl Pts',(6.76602705909268,3.30809630596838,2.71533609189988E-15));
#69407=CARTESIAN_POINT('Ctrl Pts',(6.83699907130241,3.11954532599916,1.58206781009085E-15));
#69408=CARTESIAN_POINT('Ctrl Pts',(6.90718750333259,2.93307607946455,8.69852090214781E-16));
#69409=CARTESIAN_POINT('Ctrl Pts',(6.97022825956894,2.7440666764262,-1.05615630689871E-15));
#69410=CARTESIAN_POINT('Ctrl Pts',(7.025835331104,2.55291979031694,-2.1094237467878E-15));
#69411=CARTESIAN_POINT('Ctrl Pts',(7.07793698356765,2.37382262956653,-3.46212101854286E-15));
#69412=CARTESIAN_POINT('Ctrl Pts',(7.12351236716729,2.19284848651913,-2.88434274368081E-15));
#69413=CARTESIAN_POINT('Ctrl Pts',(7.16228352934668,2.01032949625264,-4.38538094726937E-15));
#69414=CARTESIAN_POINT('Ctrl Pts',(7.19136190098122,1.87344025355278,-5.55485411509882E-15));
#69415=CARTESIAN_POINT('Ctrl Pts',(7.21661206831502,1.73568201351242,-6.23233312377065E-15));
#69416=CARTESIAN_POINT('Ctrl Pts',(7.23790051720632,1.597197609874,-5.99520433297585E-15));
#69417=CARTESIAN_POINT('Ctrl Pts',(7.24390133298475,1.55816144530123,-6.56938230126875E-15));
#69418=CARTESIAN_POINT('Ctrl Pts',(7.24958816967185,1.51906011540194,-6.87988353579413E-15));
#69419=CARTESIAN_POINT('Ctrl Pts',(7.25495188924773,1.47994306170205,-6.32827124036339E-15));
#69420=CARTESIAN_POINT('Ctrl Pts',(7.28130928311069,1.28772130652989,-3.61764061834054E-15));
#69421=CARTESIAN_POINT('Ctrl Pts',(7.29990057069104,1.09492930404099,-4.9161174975687E-15));
#69422=CARTESIAN_POINT('Ctrl Pts',(7.31049892499678,0.901945400796462,-5.38458166943201E-15));
#69423=CARTESIAN_POINT('Ctrl Pts',(7.32069773744585,0.716236697529725,-5.83538545369078E-15));
#69424=CARTESIAN_POINT('Ctrl Pts',(7.32349479503547,0.530349761762813,-8.49735146053655E-15));
#69425=CARTESIAN_POINT('Ctrl Pts',(7.3186423718122,0.34462194553665,-8.49320613838245E-15));
#69426=CARTESIAN_POINT('Ctrl Pts',(7.31355073209503,0.14973805306282,-8.40735269849132E-15));
#69427=CARTESIAN_POINT('Ctrl Pts',(7.30003679274451,-0.04497140859214,-8.72424650198269E-15));
#69428=CARTESIAN_POINT('Ctrl Pts',(7.27832783927718,-0.239012460972904,
-7.88258347483861E-15));
#69429=CARTESIAN_POINT('Ctrl Pts',(7.25659221464526,-0.433291908118023,
-7.33792831234507E-15));
#69430=CARTESIAN_POINT('Ctrl Pts',(7.22664105273108,-0.626902029575905,
-8.15483405442268E-15));
#69431=CARTESIAN_POINT('Ctrl Pts',(7.18865483465271,-0.81932603837647,-7.66053886991358E-15));
#69432=CARTESIAN_POINT('Ctrl Pts',(7.16907168253685,-0.918526980868588,
-7.92704640417113E-15));
#69433=CARTESIAN_POINT('Ctrl Pts',(7.14735227907707,-1.01741227644876,-6.68596638540915E-15));
#69434=CARTESIAN_POINT('Ctrl Pts',(7.12351690973822,-1.11590797526994,-8.38218383591993E-15));
#69435=CARTESIAN_POINT('Ctrl Pts',(7.11427622357686,-1.15409357365995,-8.33885810172723E-15));
#69436=CARTESIAN_POINT('Ctrl Pts',(7.10471747311699,-1.19222058884854,-8.36988889943339E-15));
#69437=CARTESIAN_POINT('Ctrl Pts',(7.09484172726625,-1.23028460780204,-8.10462807976364E-15));
#69438=CARTESIAN_POINT('Ctrl Pts',(7.08652641365314,-1.26233426357057,-7.88128019919228E-15));
#69439=CARTESIAN_POINT('Ctrl Pts',(7.0779855309813,-1.29434187629915,-5.88751111059832E-15));
#69440=CARTESIAN_POINT('Ctrl Pts',(7.06922855023602,-1.32627370263882,-5.55111512312578E-15));
#69441=CARTESIAN_POINT('Ctrl Pts',(7.01841803332525,-1.51155132850308,-3.59924900541043E-15));
#69442=CARTESIAN_POINT('Ctrl Pts',(6.96027727489818,-1.6945131914679,-6.19570876562944E-15));
#69443=CARTESIAN_POINT('Ctrl Pts',(6.89506241820436,-1.87470313308216,-4.6074255521944E-15));
#69444=CARTESIAN_POINT('Ctrl Pts',(6.82965550073751,-2.05542374241897,-3.01446477114324E-15));
#69445=CARTESIAN_POINT('Ctrl Pts',(6.75713237389037,-2.23335678785184,-2.31960625851253E-15));
#69446=CARTESIAN_POINT('Ctrl Pts',(6.6777034145667,-2.40802117644964,-2.22044604925031E-15));
#69447=CARTESIAN_POINT('Ctrl Pts',(6.5989855489093,-2.58112186911696,-2.12217357913706E-15));
#69448=CARTESIAN_POINT('Ctrl Pts',(6.51348450654554,-2.75101279163696,-4.30431460656709E-15));
#69449=CARTESIAN_POINT('Ctrl Pts',(6.42136423171764,-2.91719531413377,-2.33146835171283E-15));
#69450=CARTESIAN_POINT('Ctrl Pts',(6.39153541170114,-2.97100571106004,-1.69265484441239E-15));
#69451=CARTESIAN_POINT('Ctrl Pts',(6.36101228159959,-3.02442701025753,-1.86620021322499E-15));
#69452=CARTESIAN_POINT('Ctrl Pts',(6.32979959358533,-3.07744142707614,-1.4432899320127E-15));
#69453=CARTESIAN_POINT('Ctrl Pts',(6.25665722612945,-3.2016729560503,-9.6487752581363E-16));
#69454=CARTESIAN_POINT('Ctrl Pts',(6.17972892780882,-3.32367110683975,-8.91121715210751E-16));
#69455=CARTESIAN_POINT('Ctrl Pts',(6.09910488142111,-3.44327304576849,-3.33066907387547E-16));
#69456=CARTESIAN_POINT('Ctrl Pts',(6.06259861362104,-3.49742835807996,-9.66891900049288E-16));
#69457=CARTESIAN_POINT('Ctrl Pts',(6.02533449549714,-3.55109219988174,1.72414040061109E-15));
#69458=CARTESIAN_POINT('Ctrl Pts',(5.98732028987866,-3.60424847320198,0.));
#69459=CARTESIAN_POINT('Ctrl Pts',(5.96420424303597,-3.63657225543186,-1.89149828765009E-16));
#69460=CARTESIAN_POINT('Ctrl Pts',(5.94081130726099,-3.66870769301961,-2.08278402782922E-15));
#69461=CARTESIAN_POINT('Ctrl Pts',(5.91714166721159,-3.70065306896213,-7.7715611723761E-16));
#69462=CARTESIAN_POINT('Ctrl Pts',(5.89678246694326,-3.72813055932968,3.45866457342017E-16));
#69463=CARTESIAN_POINT('Ctrl Pts',(5.87621810525247,-3.75546774264844,2.65112159864947E-15));
#69464=CARTESIAN_POINT('Ctrl Pts',(5.85547020257177,-3.7826359155115,2.22044604925031E-15));
#69465=CARTESIAN_POINT('Ctrl Pts',(5.74169178169016,-3.93162214579068,-1.41314783979673E-16));
#69466=CARTESIAN_POINT('Ctrl Pts',(5.62227441123033,-4.07569710199864,-3.93788939876355E-16));
#69467=CARTESIAN_POINT('Ctrl Pts',(5.49748908512713,-4.21457279958388,3.33066907387547E-16));
#69468=CARTESIAN_POINT('Ctrl Pts',(5.37305505713184,-4.35305753156988,1.05787649575351E-15));
#69469=CARTESIAN_POINT('Ctrl Pts',(5.24328275729723,-4.48637266644393,6.27024174355871E-16));
#69470=CARTESIAN_POINT('Ctrl Pts',(5.10840575685314,-4.61419509848205,2.22044604925031E-16));
#69471=CARTESIAN_POINT('Ctrl Pts',(4.97464552680793,-4.74095917136371,-1.79581767194132E-16));
#69472=CARTESIAN_POINT('Ctrl Pts',(4.83586429127236,-4.8623214916972,1.92427926616426E-15));
#69473=CARTESIAN_POINT('Ctrl Pts',(4.69226263119319,-4.97792406018082,-3.33066907387547E-16));
#69474=CARTESIAN_POINT('Ctrl Pts',(4.55148028125308,-5.09125702054677,-2.54609493760483E-15));
#69475=CARTESIAN_POINT('Ctrl Pts',(4.40606445652634,-5.19905441201978,1.48420063567409E-15));
#69476=CARTESIAN_POINT('Ctrl Pts',(4.25618497479233,-5.30093319600521,-3.33066907387547E-16));
#69477=CARTESIAN_POINT('Ctrl Pts',(4.14933403573732,-5.37356384306032,-1.62861944896186E-15));
#69478=CARTESIAN_POINT('Ctrl Pts',(4.04021406211686,-5.4431854630145,2.9443224414169E-15));
#69479=CARTESIAN_POINT('Ctrl Pts',(3.92888236737297,-5.50964357679762,-1.11022302462516E-16));
#69480=CARTESIAN_POINT('Ctrl Pts',(-2.92283340683968,6.09544329646178,-0.664547330701837));
#69481=CARTESIAN_POINT('Ctrl Pts',(-3.93854213988516,5.60840058998238,-0.611506103854861));
#69482=CARTESIAN_POINT('Ctrl Pts',(-5.7050272011839,4.11645562634411,-0.505426300633415));
#69483=CARTESIAN_POINT('Ctrl Pts',(-7.45550178091418,-0.210827257858674,
-0.293269344663029));
#69484=CARTESIAN_POINT('Ctrl Pts',(-5.12620949291362,-6.13604307561665,
-0.0280764627906812));
#69485=CARTESIAN_POINT('Ctrl Pts',(2.40255415416736,-7.62885674758421,0.290154995456135));
#69486=CARTESIAN_POINT('Ctrl Pts',(7.71325449472373,-2.10499323613276,0.608386453702953));
#69487=CARTESIAN_POINT('Ctrl Pts',(5.93871117578135,5.35810720449711,0.926617911949768));
#69488=CARTESIAN_POINT('Ctrl Pts',(-0.0856345739722672,7.4588348660275,
1.19181079382212));
#69489=CARTESIAN_POINT('Ctrl Pts',(-4.32158964384802,5.5412541473786,1.40396509932));
#69490=CARTESIAN_POINT('Ctrl Pts',(-7.21288526193602,1.89948635041438,1.61611940481787));
#69491=CARTESIAN_POINT('Ctrl Pts',(-6.64449808808741,-4.45309590180648,
1.88131228669022));
#69492=CARTESIAN_POINT('Ctrl Pts',(0.164673416110273,-7.99633117084599,
2.19954374493704));
#69493=CARTESIAN_POINT('Ctrl Pts',(6.80998385256597,-4.18360353937514,2.51777520318386));
#69494=CARTESIAN_POINT('Ctrl Pts',(7.20734006215933,3.46751732933175,2.83600666143067));
#69495=CARTESIAN_POINT('Ctrl Pts',(0.968699846707641,7.93984220175686,3.15423811967749));
#69496=CARTESIAN_POINT('Ctrl Pts',(-4.95436512982973,5.57535620991625,3.41943100154983));
#69497=CARTESIAN_POINT('Ctrl Pts',(-6.89665372451194,1.35030356582765,3.63158530704772));
#69498=CARTESIAN_POINT('Ctrl Pts',(-6.69115139650215,-3.29525832728733,
3.84373961254559));
#69499=CARTESIAN_POINT('Ctrl Pts',(-2.09715951672875,-7.71891001831387,
4.10893249441794));
#69500=CARTESIAN_POINT('Ctrl Pts',(5.36749476028327,-5.92954507333267,4.42716395266475));
#69501=CARTESIAN_POINT('Ctrl Pts',(7.88485451519108,1.30645067348062,4.74539541091158));
#69502=CARTESIAN_POINT('Ctrl Pts',(3.1682124011442,7.34383728681522,5.06362686915839));
#69503=CARTESIAN_POINT('Ctrl Pts',(-4.47465103507491,6.63001770779555,5.38185832740521));
#69504=CARTESIAN_POINT('Ctrl Pts',(-7.39638799231719,0.961079031362873,
5.64705120927755));
#69505=CARTESIAN_POINT('Ctrl Pts',(-6.09258682522784,-3.50250887814472,
5.85920551477544));
#69506=CARTESIAN_POINT('Ctrl Pts',(-2.89139378365477,-6.87532323477221,
6.0713598202733));
#69507=CARTESIAN_POINT('Ctrl Pts',(3.4777477733007,-7.20311800115464,6.33655270214567));
#69508=CARTESIAN_POINT('Ctrl Pts',(7.94055883120079,-0.957622040899968,
6.65478416039247));
#69509=CARTESIAN_POINT('Ctrl Pts',(5.09671433411442,6.15639866781965,6.97301561863929));
#69510=CARTESIAN_POINT('Ctrl Pts',(-2.42313748367644,7.62219911374143,7.2912470768861));
#69511=CARTESIAN_POINT('Ctrl Pts',(-7.72572038657178,2.07192733349136,7.60947853513293));
#69512=CARTESIAN_POINT('Ctrl Pts',(-6.21469165940851,-4.12405568382962,
7.87467141700526));
#69513=CARTESIAN_POINT('Ctrl Pts',(-2.30356798303852,-6.63933409733441,
8.08682572250317));
#69514=CARTESIAN_POINT('Ctrl Pts',(2.32494740867123,-7.08694907910043,8.29898002800102));
#69515=CARTESIAN_POINT('Ctrl Pts',(7.34879763468661,-3.15829252949285,8.56417290987339));
#69516=CARTESIAN_POINT('Ctrl Pts',(6.62329263599618,4.4834706682624,8.88240436812019));
#69517=CARTESIAN_POINT('Ctrl Pts',(-0.188466539193348,7.99013278561538,
9.20063582636702));
#69518=CARTESIAN_POINT('Ctrl Pts',(-6.82731609888302,4.16620564318667,9.51886728461381));
#69519=CARTESIAN_POINT('Ctrl Pts',(-7.19171590592274,-3.50126558618686,
9.83709874286067));
#69520=CARTESIAN_POINT('Ctrl Pts',(-1.98822215884615,-7.18868557884129,
10.102291624733));
#69521=CARTESIAN_POINT('Ctrl Pts',(2.61404138588895,-6.52334042805334,10.3144459302309));
#69522=CARTESIAN_POINT('Ctrl Pts',(6.40222362337669,-3.82645532845434,10.5266002357288));
#69523=CARTESIAN_POINT('Ctrl Pts',(7.61944006308874,2.43387992751043,10.7917931176011));
#69524=CARTESIAN_POINT('Ctrl Pts',(2.06106675097439,7.72796987722388,11.1100245758479));
#69525=CARTESIAN_POINT('Ctrl Pts',(-5.3813117170739,5.9092491716001,11.4282560340947));
#69526=CARTESIAN_POINT('Ctrl Pts',(-7.88657750684671,-1.33094320079776,
11.7464874923416));
#69527=CARTESIAN_POINT('Ctrl Pts',(-3.13426327320923,-7.35907821066942,
12.0647189505884));
#69528=CARTESIAN_POINT('Ctrl Pts',(3.21234000341252,-6.73135197466789,12.3299118324607));
#69529=CARTESIAN_POINT('Ctrl Pts',(6.25094954120617,-3.21135680681792,12.5420661379586));
#69530=CARTESIAN_POINT('Ctrl Pts',(7.34284882357209,1.30873941583336,12.7542204434565));
#69531=CARTESIAN_POINT('Ctrl Pts',(4.15707880260768,6.83361794406501,13.0194133253288));
#69532=CARTESIAN_POINT('Ctrl Pts',(-3.51094065617307,7.18629322280136,13.3376447835757));
#69533=CARTESIAN_POINT('Ctrl Pts',(-7.93768278073829,0.933238255080724,
13.6558762418225));
#69534=CARTESIAN_POINT('Ctrl Pts',(-5.08195617773027,-6.17602104780083,
13.9741077000693));
#69535=CARTESIAN_POINT('Ctrl Pts',(2.45876366208963,-7.61144661877917,14.2923391583161));
#69536=CARTESIAN_POINT('Ctrl Pts',(6.83907561365005,-2.97611700965661,14.5575320401884));
#69537=CARTESIAN_POINT('Ctrl Pts',(6.8253206198653,1.67397166745522,14.7696863456863));
#69538=CARTESIAN_POINT('Ctrl Pts',(4.68598109533263,5.80274149679056,14.9818406511842));
#69539=CARTESIAN_POINT('Ctrl Pts',(-1.34196630560764,7.88535128013655,15.2470335330566));
#69540=CARTESIAN_POINT('Ctrl Pts',(-7.36282764599865,3.12382516005102,15.5652649913034));
#69541=CARTESIAN_POINT('Ctrl Pts',(-6.60513302389061,-4.49999547834049,
15.8834964495502));
#69542=CARTESIAN_POINT('Ctrl Pts',(0.212475557574551,-7.9952716472102,16.201727907797));
#69543=CARTESIAN_POINT('Ctrl Pts',(6.84716483161442,-4.13472757811682,16.5199593660438));
#69544=CARTESIAN_POINT('Ctrl Pts',(7.11513265916595,2.23721142202968,16.7851522479161));
#69545=CARTESIAN_POINT('Ctrl Pts',(4.05575213852165,5.73916869400773,16.9973065534141));
#69546=CARTESIAN_POINT('Ctrl Pts',(-0.266696373551286,7.453797739993,17.2094608589119));
#69547=CARTESIAN_POINT('Ctrl Pts',(-6.1835398505895,5.07380264621208,17.4746537407843));
#69548=CARTESIAN_POINT('Ctrl Pts',(-7.60743345297728,-2.46910324485873,
17.7928851990311));
#69549=CARTESIAN_POINT('Ctrl Pts',(-2.03652054591839,-7.7285396831761,18.1111166572779));
#69550=CARTESIAN_POINT('Ctrl Pts',(5.40280882453206,-5.89738682645189,18.4293481155248));
#69551=CARTESIAN_POINT('Ctrl Pts',(7.8809242737375,1.36772474136872,18.7475795737715));
#69552=CARTESIAN_POINT('Ctrl Pts',(3.90526209794003,6.35445950894199,19.0127724556439));
#69553=CARTESIAN_POINT('Ctrl Pts',(-0.70085706616846,6.99256620134576,19.2249267611418));
#69554=CARTESIAN_POINT('Ctrl Pts',(-5.08871088845878,5.45300368586626,19.4370810666396));
#69555=CARTESIAN_POINT('Ctrl Pts',(-7.99560244965949,-0.223561721984852,
19.702273948512));
#69556=CARTESIAN_POINT('Ctrl Pts',(-4.12491798751938,-6.85234019671303,
20.0205054067588));
#69557=CARTESIAN_POINT('Ctrl Pts',(3.52984749513087,-7.17062885871895,20.3387368650056));
#69558=CARTESIAN_POINT('Ctrl Pts',(7.94613586721033,-0.910186439738384,
20.6569683232524));
#69559=CARTESIAN_POINT('Ctrl Pts',(5.05357067574419,6.20008562858578,20.9751997814993));
#69560=CARTESIAN_POINT('Ctrl Pts',(-1.21791937551955,7.35845772557836,21.2403926633716));
#69561=CARTESIAN_POINT('Ctrl Pts',(-5.11409431809678,4.82008527030502,21.4525469688695));
#69562=CARTESIAN_POINT('Ctrl Pts',(-7.41760565162783,0.780611363822664,
21.6647012743673));
#69563=CARTESIAN_POINT('Ctrl Pts',(-5.89036755802206,-5.41139616069077,
21.9298941562398));
#69564=CARTESIAN_POINT('Ctrl Pts',(1.37852472933923,-7.87839984678675,22.2481256144865));
#69565=CARTESIAN_POINT('Ctrl Pts',(7.36683206291293,-3.09960109130408,22.5663570727334));
#69566=CARTESIAN_POINT('Ctrl Pts',(6.59640065605321,4.52294295343979,22.8845885309801));
#69567=CARTESIAN_POINT('Ctrl Pts',(-0.24968637690976,7.99482927208096,23.202819989227));
#69568=CARTESIAN_POINT('Ctrl Pts',(-5.74440378410562,4.75731572102831,23.4680128710993));
#69569=CARTESIAN_POINT('Ctrl Pts',(-7.02177567656341,0.286092739201462,
23.6801671765972));
#69570=CARTESIAN_POINT('Ctrl Pts',(-6.11238176155939,-4.27422705355557,
23.8923214820951));
#69571=CARTESIAN_POINT('Ctrl Pts',(-0.899256061130584,-7.94801716864386,
24.1575143639675));
#69572=CARTESIAN_POINT('Ctrl Pts',(6.20658475963767,-5.04458325302331,24.4757458222142));
#69573=CARTESIAN_POINT('Ctrl Pts',(7.59457355786801,2.4900188839659,24.7939772804611));
#69574=CARTESIAN_POINT('Ctrl Pts',(2.0148809858328,7.74014012716691,25.1122087387078));
#69575=CARTESIAN_POINT('Ctrl Pts',(-5.4306142087339,5.87265422891856,25.4304401969547));
#69576=CARTESIAN_POINT('Ctrl Pts',(-7.45652383794003,-0.174585104238434,
25.695633078827));
#69577=CARTESIAN_POINT('Ctrl Pts',(-5.48926795468329,-4.38806563636966,
25.9077873843249));
#69578=CARTESIAN_POINT('Ctrl Pts',(-1.81250951477807,-7.23498700504909,
26.1199416898228));
#69579=CARTESIAN_POINT('Ctrl Pts',(4.53242930545347,-6.59065421393082,26.3851345716951));
#69580=CARTESIAN_POINT('Ctrl Pts',(7.99384341719809,0.260733573918202,26.703366029942));
#69581=CARTESIAN_POINT('Ctrl Pts',(4.1014942480699,6.85970017576753,27.0215974881888));
#69582=CARTESIAN_POINT('Ctrl Pts',(-3.55379234536194,7.16519884869196,27.3398289464356));
#69583=CARTESIAN_POINT('Ctrl Pts',(-7.95091308272635,0.873280898375759,
27.6580604046824));
#69584=CARTESIAN_POINT('Ctrl Pts',(-5.51545799319263,-5.02095118774497,
27.9232532865547));
#69585=CARTESIAN_POINT('Ctrl Pts',(-1.26739495731764,-6.91237243857469,
28.1354075920526));
#69586=CARTESIAN_POINT('Ctrl Pts',(3.37536823488139,-6.65109893050344,28.3475618975505));
#69587=CARTESIAN_POINT('Ctrl Pts',(7.7435347899277,-2.00432216315541,28.6127547794229));
#69588=CARTESIAN_POINT('Ctrl Pts',(5.8646663894612,5.4383088102437,28.9309862376697));
#69589=CARTESIAN_POINT('Ctrl Pts',(-1.40103628535671,7.86859828022052,29.2492176959165));
#69590=CARTESIAN_POINT('Ctrl Pts',(-7.38135086693103,3.07980096020935,29.5674491541633));
#69591=CARTESIAN_POINT('Ctrl Pts',(-6.57580919452638,-4.5539402514438,29.8856806124101));
#69592=CARTESIAN_POINT('Ctrl Pts',(-0.872195548143221,-7.40739513123128,
30.1508734942825));
#69593=CARTESIAN_POINT('Ctrl Pts',(3.57541475085797,-6.0500902527771,30.3630277997804));
#69594=CARTESIAN_POINT('Ctrl Pts',(6.90954676675677,-2.80862798931996,30.5751821052782));
#69595=CARTESIAN_POINT('Ctrl Pts',(7.1608386699862,3.56399044877616,30.8403749871506));
#69596=CARTESIAN_POINT('Ctrl Pts',(0.862204568500049,7.95148526108846,31.1586064453974));
#69597=CARTESIAN_POINT('Ctrl Pts',(-6.2171550118467,5.02242223703313,31.4768379036442));
#69598=CARTESIAN_POINT('Ctrl Pts',(-7.59255309626208,-2.51448842822771,
31.795069361891));
#69599=CARTESIAN_POINT('Ctrl Pts',(-1.97900925286816,-7.75004262914722,
32.1133008201379));
#69600=CARTESIAN_POINT('Ctrl Pts',(4.19838296891676,-6.16472287703994,32.3784937020102));
#69601=CARTESIAN_POINT('Ctrl Pts',(6.666516151879,-2.223678282517,32.5906480075081));
#69602=CARTESIAN_POINT('Ctrl Pts',(7.05852069625791,2.40987827179894,32.802802313006));
#69603=CARTESIAN_POINT('Ctrl Pts',(3.06982212892467,7.38619187899295,33.0679951948783));
#69604=CARTESIAN_POINT('Ctrl Pts',(-4.56267842884224,6.56897862153834,33.3862266531251));
#69605=CARTESIAN_POINT('Ctrl Pts',(-7.98729366609293,-0.284396659556839,
33.7044581113719));
#69606=CARTESIAN_POINT('Ctrl Pts',(-4.08392440862244,-6.87685073270514,
34.0226895696187));
#69607=CARTESIAN_POINT('Ctrl Pts',(3.58736965787411,-7.14915500701318,34.3409210278655));
#69608=CARTESIAN_POINT('Ctrl Pts',(7.21204142614238,-1.90175870498772,34.606113909738));
#69609=CARTESIAN_POINT('Ctrl Pts',(6.49148130388875,2.69218372119435,34.8182682152357));
#69610=CARTESIAN_POINT('Ctrl Pts',(3.74930300284587,6.44770925967051,35.0304225207337));
#69611=CARTESIAN_POINT('Ctrl Pts',(-2.52519696832531,7.58966525267737,35.295615402606));
#69612=CARTESIAN_POINT('Ctrl Pts',(-7.7521615457203,1.9681224413906,35.6138468608529));
#69613=CARTESIAN_POINT('Ctrl Pts',(-5.84420556441641,-5.45188067452137,
35.9320783190996));
#69614=CARTESIAN_POINT('Ctrl Pts',(1.42554748487432,-7.87002725177103,36.2503097773465));
#69615=CARTESIAN_POINT('Ctrl Pts',(7.39618317595128,-3.04567115826906,36.5685412355932));
#69616=CARTESIAN_POINT('Ctrl Pts',(6.69229361918976,3.29293695945461,36.8337341174657));
#69617=CARTESIAN_POINT('Ctrl Pts',(3.13606529227772,6.28906011976134,37.0458884229635));
#69618=CARTESIAN_POINT('Ctrl Pts',(-1.39681632961355,7.32660438714381,37.2580427284614));
#69619=CARTESIAN_POINT('Ctrl Pts',(-6.88304253051742,4.07472255492631,37.5232356103338));
#69620=CARTESIAN_POINT('Ctrl Pts',(-7.14361653878869,-3.59697891597865,
37.8414670685805));
#69621=CARTESIAN_POINT('Ctrl Pts',(-0.837857072193403,-7.94831662020021,
38.1596985268274));
#69622=CARTESIAN_POINT('Ctrl Pts',(6.23659876272117,-5.00742952502321,38.4779299850742));
#69623=CARTESIAN_POINT('Ctrl Pts',(7.58137358640385,2.54998292541648,38.796161443321));
#69624=CARTESIAN_POINT('Ctrl Pts',(2.89378037003512,6.87431908441773,39.0613543251934));
#69625=CARTESIAN_POINT('Ctrl Pts',(-1.75580788781819,6.8047278688039,39.2735086306912));
#69626=CARTESIAN_POINT('Ctrl Pts',(-5.85859134437765,4.61596524726659,39.4856629361891));
#69627=CARTESIAN_POINT('Ctrl Pts',(-7.86866875051649,-1.43655507071012,
39.7508558180615));
#69628=CARTESIAN_POINT('Ctrl Pts',(-3.03518877528446,-7.39980700245872,
40.0690872763082));
#69629=CARTESIAN_POINT('Ctrl Pts',(4.57898399105715,-6.55062189246316,40.3873187345551));
#69630=CARTESIAN_POINT('Ctrl Pts',(7.99214386231922,0.308465653263491,40.7055501928019));
#69631=CARTESIAN_POINT('Ctrl Pts',(4.05221027390455,6.89632005294123,41.0237816510487));
#69632=CARTESIAN_POINT('Ctrl Pts',(-2.32248703255162,7.08775575820863,41.2889745329211));
#69633=CARTESIAN_POINT('Ctrl Pts',(-5.78745547810781,3.98654509523236,41.5011288384189));
#69634=CARTESIAN_POINT('Ctrl Pts',(-7.45005792185978,-0.35618066388343,
41.7132831439168));
#69635=CARTESIAN_POINT('Ctrl Pts',(-4.99918629725736,-6.24401911767182,
41.9784760257892));
#69636=CARTESIAN_POINT('Ctrl Pts',(2.5602735735563,-7.57723655456257,42.296707484036));
#69637=CARTESIAN_POINT('Ctrl Pts',(7.75243656531128,-1.9435711639145,42.6149389422828));
#69638=CARTESIAN_POINT('Ctrl Pts',(5.83208594208859,5.47323379176722,42.9331704005297));
#69639=CARTESIAN_POINT('Ctrl Pts',(-1.46225849090136,7.86393276181355,43.2514018587764));
#69640=CARTESIAN_POINT('Ctrl Pts',(-6.40089488270372,3.82867763137183,43.5165947406488));
#69641=CARTESIAN_POINT('Ctrl Pts',(-6.98364633268417,-0.784771691250313,
43.7287490461467));
#69642=CARTESIAN_POINT('Ctrl Pts',(-5.39150645671536,-5.15382244858969,
43.9409033516445));
#69643=CARTESIAN_POINT('Ctrl Pts',(0.31955499060767,-7.9923415207632,44.2060962335169));
#69644=CARTESIAN_POINT('Ctrl Pts',(6.90137725357106,-4.04233924592448,44.5243276917637));
#69645=CARTESIAN_POINT('Ctrl Pts',(7.12772627499534,3.61569629768823,44.8425591500105));
#69646=CARTESIAN_POINT('Ctrl Pts',(0.814705416041519,7.95649229625233,45.1607906082574));
#69647=CARTESIAN_POINT('Ctrl Pts',(-6.2603207618579,4.97875710747049,45.4790220665041));
#69648=CARTESIAN_POINT('Ctrl Pts',(-7.34330271032281,-1.30619026522004,
45.7442149483766));
#69649=CARTESIAN_POINT('Ctrl Pts',(-4.75832887350283,-5.17160410694695,
45.9563692538743));
#69650=CARTESIAN_POINT('Ctrl Pts',(-0.691486153294226,-7.42644427732359,
46.1685235593723));
#69651=CARTESIAN_POINT('Ctrl Pts',(5.48173622302567,-5.82496406492823,46.4337164412445));
#69652=CARTESIAN_POINT('Ctrl Pts',(7.86127883304989,1.47302738748871,46.7519478994915));
#69653=CARTESIAN_POINT('Ctrl Pts',(3.0109183688609,7.40352025353016,47.0701793577382));
#69654=CARTESIAN_POINT('Ctrl Pts',(-4.60182495543848,6.54161460610092,47.3884108159851));
#69655=CARTESIAN_POINT('Ctrl Pts',(-7.99125469997778,-0.345668477910065,
47.7066422742318));
#69656=CARTESIAN_POINT('Ctrl Pts',(-4.6879952360915,-5.80111440766116,47.9718351561042));
#69657=CARTESIAN_POINT('Ctrl Pts',(-0.201756218294636,-7.02470477214385,
48.1839894616021));
#69658=CARTESIAN_POINT('Ctrl Pts',(4.34731499750045,-6.06061713168695,48.3961437670999));
#69659=CARTESIAN_POINT('Ctrl Pts',(7.95824221253658,-0.803753235227211,
48.6613366489724));
#69660=CARTESIAN_POINT('Ctrl Pts',(4.96969229260987,6.26671150540889,48.9795681072191));
#69661=CARTESIAN_POINT('Ctrl Pts',(-2.58103328601835,7.5641264363336,49.297799565466));
#69662=CARTESIAN_POINT('Ctrl Pts',(-7.7637763300124,1.92179386844403,49.6160310237127));
#69663=CARTESIAN_POINT('Ctrl Pts',(-5.80702124690748,-5.50074018787491,
49.9342624819596));
#69664=CARTESIAN_POINT('Ctrl Pts',(0.26410876978471,-7.453889874563,50.1994553638319));
#69665=CARTESIAN_POINT('Ctrl Pts',(4.45366316330294,-5.43618130080664,50.4116096693298));
#69666=CARTESIAN_POINT('Ctrl Pts',(7.25622959650091,-1.72550275202747,50.6237639748277));
#69667=CARTESIAN_POINT('Ctrl Pts',(6.53575466830331,4.61124162154712,50.8889568567));
#69668=CARTESIAN_POINT('Ctrl Pts',(-0.356703040538174,7.99013626392697,
51.2071883149469));
#69669=CARTESIAN_POINT('Ctrl Pts',(-6.90845543503368,4.01882881826647,51.5254197731937));
#69670=CARTESIAN_POINT('Ctrl Pts',(-7.1220091321019,-3.63957421926061,51.8436512314404));
#69671=CARTESIAN_POINT('Ctrl Pts',(-0.777745171693893,-7.96082601395384,
52.1618826896873));
#69672=CARTESIAN_POINT('Ctrl Pts',(5.0868175702758,-5.45476990450777,52.4270755715598));
#69673=CARTESIAN_POINT('Ctrl Pts',(6.92709267685679,-1.18430137787557,52.6392298770574));
#69674=CARTESIAN_POINT('Ctrl Pts',(6.61008875479717,3.45498977684364,52.8513841825556));
#69675=CARTESIAN_POINT('Ctrl Pts',(1.91119504467174,7.76704396007644,53.1165770644276));
#69676=CARTESIAN_POINT('Ctrl Pts',(-5.50833831846516,5.79894158830544,53.4348085226747));
#69677=CARTESIAN_POINT('Ctrl Pts',(-7.85120765946141,-1.49541962551961,
53.7530399809213));
#69678=CARTESIAN_POINT('Ctrl Pts',(-2.99094532675873,-7.41780025530413,
54.0712714391683));
#69679=CARTESIAN_POINT('Ctrl Pts',(4.63257276104932,-6.5206524205881,54.389502897415));
#69680=CARTESIAN_POINT('Ctrl Pts',(7.41733421524318,-0.78318634038966,54.6546957792874));
#69681=CARTESIAN_POINT('Ctrl Pts',(6.00672129400615,3.64780509396192,54.8668500847852));
#69682=CARTESIAN_POINT('Ctrl Pts',(2.72545722329887,6.94277398655306,55.0790043902831));
#69683=CARTESIAN_POINT('Ctrl Pts',(-3.64971923139309,7.11752681122709,55.3441972721555));
#69684=CARTESIAN_POINT('Ctrl Pts',(-7.96126514899932,0.766662769787909,
55.6624287304023));
#69685=CARTESIAN_POINT('Ctrl Pts',(-4.94740594913963,-6.27701489107626,
55.9806601886491));
#69686=CARTESIAN_POINT('Ctrl Pts',(2.60547680487975,-7.5618122956394,56.2988916468959));
#69687=CARTESIAN_POINT('Ctrl Pts',(7.7732473784035,-1.88580581467994,56.6171231051428));
#69688=CARTESIAN_POINT('Ctrl Pts',(6.11386519220779,4.27210488119153,56.8823159870151));
#69689=CARTESIAN_POINT('Ctrl Pts',(2.14346794565811,6.69273694936065,57.094470292513));
#69690=CARTESIAN_POINT('Ctrl Pts',(-2.49446165009483,7.02907453229768,57.3066245980108));
#69691=CARTESIAN_POINT('Ctrl Pts',(-7.42252109479894,2.98090908512862,57.5718174798833));
#69692=CARTESIAN_POINT('Ctrl Pts',(-6.51371741399781,-4.64122828848479,
57.8900489381299));
#69693=CARTESIAN_POINT('Ctrl Pts',(0.380285772234508,-7.98330284404963,
58.2082803963769));
#69694=CARTESIAN_POINT('Ctrl Pts',(6.92539378082645,-4.00105430552253,58.5265118546236));
#69695=CARTESIAN_POINT('Ctrl Pts',(7.10556325834136,3.67295646016214,58.8447433128705));
#69696=CARTESIAN_POINT('Ctrl Pts',(1.81502103305887,7.23435735597458,59.1099361947428));
#69697=CARTESIAN_POINT('Ctrl Pts',(-2.76993786559711,6.45868616114241,59.3220905002406));
#69698=CARTESIAN_POINT('Ctrl Pts',(-6.49226518895258,3.67161005836745,59.5342448057386));
#69699=CARTESIAN_POINT('Ctrl Pts',(-7.55879607452801,-2.6161498963625,59.7994376876108));
#69700=CARTESIAN_POINT('Ctrl Pts',(-1.87489434462579,-7.7752354158405,60.1176691458578));
#69701=CARTESIAN_POINT('Ctrl Pts',(5.52166351530564,-5.77831927052477,60.4359006041045));
#69702=CARTESIAN_POINT('Ctrl Pts',(7.85234220304677,1.51994621664714,60.7541320623515));
#69703=CARTESIAN_POINT('Ctrl Pts',(2.95663988242443,7.43222167203017,61.0723635205981));
#69704=CARTESIAN_POINT('Ctrl Pts',(-3.37305910088342,6.65227028963328,61.3375564024706));
#69705=CARTESIAN_POINT('Ctrl Pts',(-6.3262638672153,3.06032158273721,61.5497107079684));
#69706=CARTESIAN_POINT('Ctrl Pts',(-7.30930351420548,-1.48469183388794,
61.7618650134663));
#69707=CARTESIAN_POINT('Ctrl Pts',(-3.99177876553422,-6.93147463845664,
62.0270578953387));
#69708=CARTESIAN_POINT('Ctrl Pts',(3.68249852080414,-7.09990980361901,62.3452893535855));
#69709=CARTESIAN_POINT('Ctrl Pts',(7.95780437732607,-0.742355077159724,
62.6635208118322));
#69710=CARTESIAN_POINT('Ctrl Pts',(4.93218084187855,6.29627721103956,62.9817522700792));
#69711=CARTESIAN_POINT('Ctrl Pts',(-2.64083450203343,7.5502073818808,63.2999837283258));
#69712=CARTESIAN_POINT('Ctrl Pts',(-6.90857133452179,2.81102647092016,63.5651766101983));
#69713=CARTESIAN_POINT('Ctrl Pts',(-6.78315393156382,-1.83739093502485,
63.7773309156961));
#69714=CARTESIAN_POINT('Ctrl Pts',(-4.54528381471436,-5.91359643094503,
63.989485221194));
#69715=CARTESIAN_POINT('Ctrl Pts',(1.53093669630508,-7.85085162313262,64.2546781030663));
#69716=CARTESIAN_POINT('Ctrl Pts',(7.4357193671895,-2.94611474108738,64.5729095613132));
#69717=CARTESIAN_POINT('Ctrl Pts',(6.49516621486331,4.65731225168266,64.8911410195599));
#69718=CARTESIAN_POINT('Ctrl Pts',(-0.404411270724643,7.98786367556194,
65.2093724778069));
#69719=CARTESIAN_POINT('Ctrl Pts',(-6.94448088124453,3.96910867406852,65.5276039360535));
#69720=CARTESIAN_POINT('Ctrl Pts',(-7.05935686076257,-2.40742775941292,
65.7927968179261));
#69721=CARTESIAN_POINT('Ctrl Pts',(-3.91676322470201,-5.83490775839923,
66.0049511234238));
#69722=CARTESIAN_POINT('Ctrl Pts',(0.445613595873354,-7.44524386622448,
66.2171054289218));
#69723=CARTESIAN_POINT('Ctrl Pts',(6.30359804819689,-4.9238491064726,66.482298310794));
#69724=CARTESIAN_POINT('Ctrl Pts',(7.54594708052756,2.65107473171896,66.800529769041));
#69725=CARTESIAN_POINT('Ctrl Pts',(1.85034153482128,7.77521560940999,67.1187612272876));
#69726=CARTESIAN_POINT('Ctrl Pts',(-5.54286956338981,5.76594411857648,67.4369926855345));
#69727=CARTESIAN_POINT('Ctrl Pts',(-7.84580733502515,-1.55658139471971,
67.7552241437814));
#69728=CARTESIAN_POINT('Ctrl Pts',(-3.75154110074661,-6.44640729967567,
68.0204170256537));
#69729=CARTESIAN_POINT('Ctrl Pts',(0.868573158644488,-6.97371947930176,
68.2325713311516));
#69730=CARTESIAN_POINT('Ctrl Pts',(5.21819086966696,-5.32923181627554,68.4447256366494));
#69731=CARTESIAN_POINT('Ctrl Pts',(7.98792816139811,0.415502181809365,68.7099185185218));
#69732=CARTESIAN_POINT('Ctrl Pts',(3.95917763219824,6.94941918853656,69.0281499767686));
#69733=CARTESIAN_POINT('Ctrl Pts',(-3.70102374668385,7.08379593074294,69.3463814350154));
#69734=CARTESIAN_POINT('Ctrl Pts',(-7.96570146350195,0.719106919648195,
69.6646128932623));
#69735=CARTESIAN_POINT('Ctrl Pts',(-4.90322564425964,-6.31965321033109,
69.9828443515091));
#69736=CARTESIAN_POINT('Ctrl Pts',(1.39427281500069,-7.32708884673901,70.2480372333814));
#69737=CARTESIAN_POINT('Ctrl Pts',(5.22836818999202,-4.69588636995774,70.4601915388793));
#69738=CARTESIAN_POINT('Ctrl Pts',(7.43421207706811,-0.602261222926253,
70.6723458443772));
#69739=CARTESIAN_POINT('Ctrl Pts',(5.75872064546006,5.55128583577292,70.9375387262495));
#69740=CARTESIAN_POINT('Ctrl Pts',(-1.56731762340354,7.84302433409703,71.2557701844964));
#69741=CARTESIAN_POINT('Ctrl Pts',(-7.4391409603632,2.92180141067608,71.5740016427431));
#69742=CARTESIAN_POINT('Ctrl Pts',(-6.48588522666362,-4.6800432492488,71.89223310099));
#69743=CARTESIAN_POINT('Ctrl Pts',(0.441600573455518,-7.98652817688489,
72.2104645592367));
#69744=CARTESIAN_POINT('Ctrl Pts',(5.85698884249447,-4.61799821676437,72.4756574411092));
#69745=CARTESIAN_POINT('Ctrl Pts',(7.02662058273795,-0.117391358426442,
72.687811746607));
#69746=CARTESIAN_POINT('Ctrl Pts',(6.00797953533027,4.41977792653008,72.8999660521049));
#69747=CARTESIAN_POINT('Ctrl Pts',(0.708132550329375,7.96731585161226,73.1651589339772));
#69748=CARTESIAN_POINT('Ctrl Pts',(-6.32593134632851,4.89409127288728,73.4833903922241));
#69749=CARTESIAN_POINT('Ctrl Pts',(-7.53259465664785,-2.67168746361502,
73.8016218504708));
#69750=CARTESIAN_POINT('Ctrl Pts',(-1.82841823496171,-7.78627045868244,
74.1198533087177));
#69751=CARTESIAN_POINT('Ctrl Pts',(5.5700503670788,-5.74059578517867,74.4380847669645));
#69752=CARTESIAN_POINT('Ctrl Pts',(7.45022067480577,0.353672707356798,74.7032776488368));
#69753=CARTESIAN_POINT('Ctrl Pts',(5.38225798952639,4.51851390470657,74.9154319543348));
#69754=CARTESIAN_POINT('Ctrl Pts',(1.63837574292985,7.27668056502784,75.1275862598326));
#69755=CARTESIAN_POINT('Ctrl Pts',(-4.68966200686914,6.47937198055273,75.3927791417049));
#69756=CARTESIAN_POINT('Ctrl Pts',(-7.98481911427963,-0.451714078618975,
75.7110105999518));
#69757=CARTESIAN_POINT('Ctrl Pts',(-3.93641975399691,-6.95786990334269,
76.0292420581986));
#69758=CARTESIAN_POINT('Ctrl Pts',(3.72640233843597,-7.07468376429424,76.3474735164454));
#69759=CARTESIAN_POINT('Ctrl Pts',(7.96656438966708,-0.688066392457169,
76.6657049746923));
#69760=CARTESIAN_POINT('Ctrl Pts',(4.88424055995273,6.3309887778437,76.983936432939));
#69761=CARTESIAN_POINT('Ctrl Pts',(-2.68513291585741,7.52976860837553,77.3021678911859));
#69762=CARTESIAN_POINT('Ctrl Pts',(-7.78912256814826,1.81409798934657,77.6203993494327));
#69763=CARTESIAN_POINT('Ctrl Pts',(-5.73116360124679,-5.57933282541807,
77.9386308076794));
#69764=CARTESIAN_POINT('Ctrl Pts',(0.366457134883102,-7.44983652765403,
78.2038236895519));
#69765=CARTESIAN_POINT('Ctrl Pts',(4.52781078590357,-5.37443936238026,78.4159779950496));
#69766=CARTESIAN_POINT('Ctrl Pts',(7.27925103524264,-1.62584650356412,78.6281323005476));
#69767=CARTESIAN_POINT('Ctrl Pts',(6.47184422235408,4.70054607701997,78.8933251824199));
#69768=CARTESIAN_POINT('Ctrl Pts',(-0.466311279410581,7.98446458370159,
79.2115566406668));
#69769=CARTESIAN_POINT('Ctrl Pts',(-6.96295945194999,3.92365796612018,79.5297880989135));
#69770=CARTESIAN_POINT('Ctrl Pts',(-7.07139022597889,-3.73697431858228,
79.8480195571604));
#69771=CARTESIAN_POINT('Ctrl Pts',(-0.668426236305269,-7.9707452571768,
80.1662510154071));
#69772=CARTESIAN_POINT('Ctrl Pts',(5.16119534842955,-5.38445146622561,80.4314438972796));
#69773=CARTESIAN_POINT('Ctrl Pts',(6.94269238652436,-1.08912807827487,80.6435982027774));
#69774=CARTESIAN_POINT('Ctrl Pts',(6.56205343067632,3.54537453650439,80.8557525082755));
#69775=CARTESIAN_POINT('Ctrl Pts',(1.80442728846643,7.7925403782906,81.1209453901475));
#69776=CARTESIAN_POINT('Ctrl Pts',(-5.58739884552956,5.72280404428344,81.4391768483945));
#69777=CARTESIAN_POINT('Ctrl Pts',(-7.82994662556973,-1.60302138236276,
81.7574083066413));
#69778=CARTESIAN_POINT('Ctrl Pts',(-2.88886868043504,-7.4581467527175,82.0756397648882));
#69779=CARTESIAN_POINT('Ctrl Pts',(4.72161988681341,-6.45646525177274,82.3938712231348));
#69780=CARTESIAN_POINT('Ctrl Pts',(7.42738348108055,-0.681324014282815,
82.6590641050074));
#69781=CARTESIAN_POINT('Ctrl Pts',(5.95609658300921,3.72989225361022,82.8712184105051));
#69782=CARTESIAN_POINT('Ctrl Pts',(2.62992441186326,6.97952184884766,83.0833727160031));
#69783=CARTESIAN_POINT('Ctrl Pts',(-3.74704986675743,7.06677123681013,83.3485655978754));
#69784=CARTESIAN_POINT('Ctrl Pts',(-7.97103643639252,0.657337582393124,
83.6667970561222));
#69785=CARTESIAN_POINT('Ctrl Pts',(-4.86080016327485,-6.34431740494078,
83.9850285143689));
#69786=CARTESIAN_POINT('Ctrl Pts',(2.70900273192573,-7.52534509372946,84.3032599726158));
#69787=CARTESIAN_POINT('Ctrl Pts',(7.79839444842538,-1.77895542426286,84.6214914308625));
#69788=CARTESIAN_POINT('Ctrl Pts',(6.05466308452315,4.35560359040991,84.886684312735));
#69789=CARTESIAN_POINT('Ctrl Pts',(2.05142121191431,6.7215216818231,85.0988386182328));
#69790=CARTESIAN_POINT('Ctrl Pts',(-2.59068723364047,6.99418096429851,85.3109929237309));
#69791=CARTESIAN_POINT('Ctrl Pts',(-7.46272936928494,2.87876861479598,85.576185805603));
#69792=CARTESIAN_POINT('Ctrl Pts',(-6.44941214782463,-4.73017943875191,
85.89441726385));
#69793=CARTESIAN_POINT('Ctrl Pts',(0.489805379921119,-7.97733240238224,
86.2126487220966));
#69794=CARTESIAN_POINT('Ctrl Pts',(6.97964839115342,-3.90563988498063,86.5308801803437));
#69795=CARTESIAN_POINT('Ctrl Pts',(7.05448992189358,3.77012072995617,86.8491116385901));
#69796=CARTESIAN_POINT('Ctrl Pts',(1.71557253344269,7.25858378658518,87.1143045204627));
#69797=CARTESIAN_POINT('Ctrl Pts',(-2.85831002962552,6.42006592504683,87.3264588259607));
#69798=CARTESIAN_POINT('Ctrl Pts',(-6.54203959894669,3.58217051383667,87.5386131314584));
#69799=CARTESIAN_POINT('Ctrl Pts',(-7.52218268870725,-2.71963342644761,
87.8038060133308));
#69800=CARTESIAN_POINT('Ctrl Pts',(-1.76801769993584,-7.80023255986408,
88.1220374715777));
#69801=CARTESIAN_POINT('Ctrl Pts',(5.6004398390903,-5.70200098010378,88.4402689298243));
#69802=CARTESIAN_POINT('Ctrl Pts',(7.83074445421797,1.62756132541459,88.7585003880712));
#69803=CARTESIAN_POINT('Ctrl Pts',(2.85436857570851,7.47209598509982,89.0767318463181));
#69804=CARTESIAN_POINT('Ctrl Pts',(-3.46403103994571,6.60535515007955,89.3419247281905));
#69805=CARTESIAN_POINT('Ctrl Pts',(-6.36766515477992,2.97321764827318,89.5540790336882));
#69806=CARTESIAN_POINT('Ctrl Pts',(-7.28824069935606,-1.58485810489139,
89.7662333391863));
#69807=CARTESIAN_POINT('Ctrl Pts',(-3.89628177039754,-6.98560138729692,
90.0314262210585));
#69808=CARTESIAN_POINT('Ctrl Pts',(3.7795843093107,-7.0487060531747,90.3496576793053));
#69809=CARTESIAN_POINT('Ctrl Pts',(7.96724241483808,-0.633079672380178,
90.6678891375522));
#69810=CARTESIAN_POINT('Ctrl Pts',(4.84531215134557,6.36336897651491,90.9861205957989));
#69811=CARTESIAN_POINT('Ctrl Pts',(-2.74419784445042,7.51325605626818,91.3043520540459));
#69812=CARTESIAN_POINT('Ctrl Pts',(-6.94649669459085,2.71595496583219,91.569544935918));
#69813=CARTESIAN_POINT('Ctrl Pts',(-6.75730054780259,-1.93030360670755,
91.7816992414161));
#69814=CARTESIAN_POINT('Ctrl Pts',(-4.46370311146622,-5.97541481715509,
91.9938535469138));
#69815=CARTESIAN_POINT('Ctrl Pts',(1.6385303148144,-7.82910319155211,92.2590464287863));
#69816=CARTESIAN_POINT('Ctrl Pts',(7.47544891365297,-2.84379642636655,92.577277887033));
#69817=CARTESIAN_POINT('Ctrl Pts',(6.43064197423995,4.74600730799249,92.8955093452797));
#69818=CARTESIAN_POINT('Ctrl Pts',(-0.513991195223748,7.98156172853921,
93.2137408035268));
#69819=CARTESIAN_POINT('Ctrl Pts',(-6.99829530210772,3.87343532810802,93.5319722617734));
#69820=CARTESIAN_POINT('Ctrl Pts',(-7.02565481334343,-2.50407710506977,
93.797165143646));
#69821=CARTESIAN_POINT('Ctrl Pts',(-3.83632155666589,-5.88810832281994,
94.0093194491437));
#69822=CARTESIAN_POINT('Ctrl Pts',(0.547743231317241,-7.43842759304252,
94.2214737546418));
#69823=CARTESIAN_POINT('Ctrl Pts',(6.37057478731908,-4.83688073614729,94.4866666365138));
#69824=CARTESIAN_POINT('Ctrl Pts',(7.50885562870737,2.75437864544419,94.8048980947609));
#69825=CARTESIAN_POINT('Ctrl Pts',(1.74346747397237,7.79987581539445,95.1231295530076));
#69826=CARTESIAN_POINT('Ctrl Pts',(-5.62147406522839,5.68933598139671,95.4413610112545));
#69827=CARTESIAN_POINT('Ctrl Pts',(-7.82370745446396,-1.66410337524508,
95.7595924695011));
#69828=CARTESIAN_POINT('Ctrl Pts',(-3.66272334045319,-6.49728292716958,
96.0247853513737));
#69829=CARTESIAN_POINT('Ctrl Pts',(0.964192204000728,-6.96114330416675,
96.2369396568714));
#69830=CARTESIAN_POINT('Ctrl Pts',(5.29083291191058,-5.25712039073047,96.4490939623694));
#69831=CARTESIAN_POINT('Ctrl Pts',(7.98147400706142,0.525081947070879,96.7142868442416));
#69832=CARTESIAN_POINT('Ctrl Pts',(3.86343745250282,7.00309685966486,97.0325183024886));
#69833=CARTESIAN_POINT('Ctrl Pts',(-3.79788665865216,7.03233947533876,97.3507497607354));
#69834=CARTESIAN_POINT('Ctrl Pts',(-7.97481972187845,0.609725330610525,
97.668981218982));
#69835=CARTESIAN_POINT('Ctrl Pts',(-4.81603888871812,-6.38634541806905,
97.9872126772292));
#69836=CARTESIAN_POINT('Ctrl Pts',(1.49469166773618,-7.30726518766016,98.2524055591011));
#69837=CARTESIAN_POINT('Ctrl Pts',(5.29231783318236,-4.62369491424136,98.4645598645992));
#69838=CARTESIAN_POINT('Ctrl Pts',(7.44177689490699,-0.500184316846411,
98.676714170097));
#69839=CARTESIAN_POINT('Ctrl Pts',(5.68199770515192,5.6297904450508,98.9419070519693));
#69840=CARTESIAN_POINT('Ctrl Pts',(-1.67480042471626,7.82077733429483,99.2601385102162));
#69841=CARTESIAN_POINT('Ctrl Pts',(-7.47853648893081,2.81943851717081,99.578369968463));
#69842=CARTESIAN_POINT('Ctrl Pts',(-6.42105000078872,-4.7686089651617,99.8966014267099));
#69843=CARTESIAN_POINT('Ctrl Pts',(0.551158827295702,-7.97971567937298,
100.214832884957));
#69844=CARTESIAN_POINT('Ctrl Pts',(5.91981014714418,-4.53718806378571,100.480025766829));
#69845=CARTESIAN_POINT('Ctrl Pts',(7.02757025506314,-0.020952745718006,
100.692180072327));
#69846=CARTESIAN_POINT('Ctrl Pts',(5.94675997122199,4.50180780898751,100.904334377825));
#69847=CARTESIAN_POINT('Ctrl Pts',(0.598731752276945,7.9762872732464,101.169527259698));
#69848=CARTESIAN_POINT('Ctrl Pts',(-6.39250081992776,4.80681264898825,101.487758717944));
#69849=CARTESIAN_POINT('Ctrl Pts',(-7.49521572953847,-2.77479417904354,
101.805990176191));
#69850=CARTESIAN_POINT('Ctrl Pts',(-1.72140562995735,-7.81065152419441,
102.124221634438));
#69851=CARTESIAN_POINT('Ctrl Pts',(5.64832647306271,-5.66357187914456,102.442453092685));
#69852=CARTESIAN_POINT('Ctrl Pts',(7.44462716948537,0.455800407799888,102.707645974557));
#69853=CARTESIAN_POINT('Ctrl Pts',(5.31979465006875,4.59205483291529,102.919800280055));
#69854=CARTESIAN_POINT('Ctrl Pts',(1.53823802277218,7.29822248836579,103.131954585553));
#69855=CARTESIAN_POINT('Ctrl Pts',(-4.77787174527572,6.4149497240613,103.397147467425));
#69856=CARTESIAN_POINT('Ctrl Pts',(-7.97831370836171,-0.562160961128552,
103.715378925672));
#69857=CARTESIAN_POINT('Ctrl Pts',(-3.83975269512832,-7.00956780469594,
104.033610383919));
#69858=CARTESIAN_POINT('Ctrl Pts',(3.82160958092987,-7.02600987660817,104.351841842166));
#69859=CARTESIAN_POINT('Ctrl Pts',(7.97820106506273,-0.57266582050002,104.670073300412));
#69860=CARTESIAN_POINT('Ctrl Pts',(5.32208684584968,5.22547790251025,104.935266182285));
#69861=CARTESIAN_POINT('Ctrl Pts',(1.00568407969865,6.9552701054123,105.147420487783));
#69862=CARTESIAN_POINT('Ctrl Pts',(-3.62391518544271,6.51900808659635,105.359574793281));
#69863=CARTESIAN_POINT('Ctrl Pts',(-7.81364537834605,1.71072624285364,105.624767675153));
#69864=CARTESIAN_POINT('Ctrl Pts',(-5.65529940502205,-5.65571420908154,
105.9429991334));
#69865=CARTESIAN_POINT('Ctrl Pts',(1.69692613162078,-7.810133370961,106.261230591646));
#69866=CARTESIAN_POINT('Ctrl Pts',(7.49229788260741,-2.79910468070165,106.579462049893));
#69867=CARTESIAN_POINT('Ctrl Pts',(6.39930365278937,4.79880726180303,106.89769350814));
#69868=CARTESIAN_POINT('Ctrl Pts',(0.592088537923887,7.43502917732339,107.162886390013));
#69869=CARTESIAN_POINT('Ctrl Pts',(-3.80114279899899,5.91087947170466,107.37504069551));
#69870=CARTESIAN_POINT('Ctrl Pts',(-7.01059819590207,2.5459262833012,107.587195001008));
#69871=CARTESIAN_POINT('Ctrl Pts',(-7.02126802134622,-3.83163591028142,
107.852387882881));
#69872=CARTESIAN_POINT('Ctrl Pts',(-0.561575788910652,-7.97835491868844,
108.170619341127));
#69873=CARTESIAN_POINT('Ctrl Pts',(6.40222739562009,-4.78426859019708,108.488850799374));
#69874=CARTESIAN_POINT('Ctrl Pts',(7.49227345438683,2.79917006627677,108.807082257621));
#69875=CARTESIAN_POINT('Ctrl Pts',(1.68518581163966,7.81919351063693,109.125313715868));
#69876=CARTESIAN_POINT('Ctrl Pts',(-4.42799259471567,6.0019254648432,109.39050659774));
#69877=CARTESIAN_POINT('Ctrl Pts',(-6.74567008963042,1.97056280013258,109.602660903238));
#69878=CARTESIAN_POINT('Ctrl Pts',(-6.96256832586624,-2.67448499940349,
109.814815208736));
#69879=CARTESIAN_POINT('Ctrl Pts',(-2.78895030028104,-7.49675893964188,
110.080008090608));
#69880=CARTESIAN_POINT('Ctrl Pts',(4.80728149506295,-6.39214824628434,110.398239548855));
#69881=CARTESIAN_POINT('Ctrl Pts',(7.97087579703635,0.585560070868035,110.716471007102));
#69882=CARTESIAN_POINT('Ctrl Pts',(3.82154826442267,7.02604322773049,111.034702465349));
#69883=CARTESIAN_POINT('Ctrl Pts',(-3.85455763969707,7.00871056463248,111.352933923595));
#69884=CARTESIAN_POINT('Ctrl Pts',(-7.2786606794505,1.62828941463469,111.618126805468));
#69885=CARTESIAN_POINT('Ctrl Pts',(-6.38528112390476,-2.9351946572768,111.830281110966));
#69886=CARTESIAN_POINT('Ctrl Pts',(-3.50335692154129,-6.5845818382551,112.042435416464));
#69887=CARTESIAN_POINT('Ctrl Pts',(2.8097620210391,-7.48898362674566,112.307628298336));
#69888=CARTESIAN_POINT('Ctrl Pts',(7.82090015176617,-1.67422680403625,112.625859756583));
#69889=CARTESIAN_POINT('Ctrl Pts',(5.63434107372123,5.66850440886771,112.94409121483));
#69890=CARTESIAN_POINT('Ctrl Pts',(-1.72147379386281,7.81063650109863,113.262322673076));
#69891=CARTESIAN_POINT('Ctrl Pts',(-7.50583189001486,2.76443954814953,113.580554131323));
#69892=CARTESIAN_POINT('Ctrl Pts',(-6.56328362939538,-3.5430969087086,113.845747013196));
#69893=CARTESIAN_POINT('Ctrl Pts',(-2.89654180789393,-6.40290779744046,
114.057901318693));
#69894=CARTESIAN_POINT('Ctrl Pts',(1.67225938963234,-7.26868462915931,114.270055624191));
#69895=CARTESIAN_POINT('Ctrl Pts',(7.03188342456394,-3.81211934229238,114.535248506064));
#69896=CARTESIAN_POINT('Ctrl Pts',(7.00281347638515,3.86395108537982,114.853479964311));
#69897=CARTESIAN_POINT('Ctrl Pts',(0.537365184297669,7.97426988677213,115.171711422557));
#69898=CARTESIAN_POINT('Ctrl Pts',(-6.42109161644814,4.76855292813543,115.489942880804));
#69899=CARTESIAN_POINT('Ctrl Pts',(-7.4797626739027,-2.83421747906345,115.808174339051));
#69900=CARTESIAN_POINT('Ctrl Pts',(-2.63234719477822,-6.97860845373441,
116.073367220923));
#69901=CARTESIAN_POINT('Ctrl Pts',(2.01130457693764,-6.73363472473754,116.285521526421));
#69902=CARTESIAN_POINT('Ctrl Pts',(6.02858315192499,-4.3916298665434,116.497675831919));
#69903=CARTESIAN_POINT('Ctrl Pts',(7.80886364361634,1.73242228453224,116.762868713792));
#69904=CARTESIAN_POINT('Ctrl Pts',(2.75382789980835,7.50905762885649,117.081100172038));
#69905=CARTESIAN_POINT('Ctrl Pts',(-4.82288283518692,6.37318936847433,117.399331630285));
#69906=CARTESIAN_POINT('Ctrl Pts',(-7.97481440046939,-0.609794927262758,
117.717563088532));
#69907=CARTESIAN_POINT('Ctrl Pts',(-3.78912212147895,-7.04430208928159,
118.035794546779));
#69908=CARTESIAN_POINT('Ctrl Pts',(2.58825904592296,-6.99507990058644,118.300987428651));
#69909=CARTESIAN_POINT('Ctrl Pts',(5.93374949616459,-3.76534190003606,118.513141734149));
#69910=CARTESIAN_POINT('Ctrl Pts',(7.43131413590726,0.637022698069072,118.725296039647));
#69911=CARTESIAN_POINT('Ctrl Pts',(4.76003559506075,6.42819566521531,118.990488921519));
#69912=CARTESIAN_POINT('Ctrl Pts',(-2.84434470672376,7.47524031483816,119.308720379766));
#69913=CARTESIAN_POINT('Ctrl Pts',(-7.82024863945352,1.64968263175073,119.626951838013));
#69914=CARTESIAN_POINT('Ctrl Pts',(-5.62142441387692,-5.68938504008292,
119.94518329626));
#69915=CARTESIAN_POINT('Ctrl Pts',(1.75792871045866,-7.8031612200109,120.263414754506));
#69916=CARTESIAN_POINT('Ctrl Pts',(6.54079565338119,-3.58444136862353,120.528607636379));
#69917=CARTESIAN_POINT('Ctrl Pts',(6.94906363216944,1.04771052464956,120.740761941877));
#69918=CARTESIAN_POINT('Ctrl Pts',(5.19321024840485,5.35357777754774,120.952916247375));
#69919=CARTESIAN_POINT('Ctrl Pts',(-0.620883826172455,7.97459351007532,
121.218109129247));
#69920=CARTESIAN_POINT('Ctrl Pts',(-7.04898324843627,3.77906731066201,121.536340587494));
#69921=CARTESIAN_POINT('Ctrl Pts',(-6.98622830803955,-3.88205558903035,
121.854572045741));
#69922=CARTESIAN_POINT('Ctrl Pts',(-0.513921539690748,-7.98156621386383,
122.172803503987));
#69923=CARTESIAN_POINT('Ctrl Pts',(6.44371489477547,-4.73900588007502,122.491034962234));
#69924=CARTESIAN_POINT('Ctrl Pts',(7.28879044406725,1.58232789486348,122.756227844106));
#69925=CARTESIAN_POINT('Ctrl Pts',(4.55981260870684,5.34745656185066,122.968382149604));
#69926=CARTESIAN_POINT('Ctrl Pts',(0.410789081138449,7.44724647337578,123.180536455102));
#69927=CARTESIAN_POINT('Ctrl Pts',(-5.69761270396623,5.6139868054832,123.445729336975));
#69928=CARTESIAN_POINT('Ctrl Pts',(-7.80010286333989,-1.76858980449572,
123.763960795221));
#69929=CARTESIAN_POINT('Ctrl Pts',(-2.72943467181251,-7.51185249726616,
124.082192253468));
#69930=CARTESIAN_POINT('Ctrl Pts',(4.84536768462038,-6.36332669097587,124.400423711715));
#69931=CARTESIAN_POINT('Ctrl Pts',(7.97252218387298,0.646937712759203,124.718655169962));
#69932=CARTESIAN_POINT('Ctrl Pts',(4.46577720920391,5.97386488147713,124.983848051834));
#69933=CARTESIAN_POINT('Ctrl Pts',(-0.0634342396665083,7.02731519178123,
125.196002357332));
#69934=CARTESIAN_POINT('Ctrl Pts',(-4.57289059627595,5.89227454374625,125.40815666283));
#69935=CARTESIAN_POINT('Ctrl Pts',(-7.98290165102412,0.50291113192436,125.673349544702));
#69936=CARTESIAN_POINT('Ctrl Pts',(-4.72970639284564,-6.44975906625399,
125.991581002949));
#69937=CARTESIAN_POINT('Ctrl Pts',(2.8645949836211,-7.46135625393853,126.309812461196));
#69938=CARTESIAN_POINT('Ctrl Pts',(7.83075865773387,-1.62749298602955,126.628043919442));
#69939=CARTESIAN_POINT('Ctrl Pts',(5.59533973146904,5.71592614245338,126.94627537769));
#69940=CARTESIAN_POINT('Ctrl Pts',(-0.545160946366092,7.43861729402364,
127.211468259562));
#69941=CARTESIAN_POINT('Ctrl Pts',(-4.65560265593447,5.26427075837259,127.42362256506));
#69942=CARTESIAN_POINT('Ctrl Pts',(-7.31616713073084,1.45049171648925,127.635776870558));
#69943=CARTESIAN_POINT('Ctrl Pts',(-6.35711562868407,-4.85455654618202,
127.90096975243));
#69944=CARTESIAN_POINT('Ctrl Pts',(0.657922218832197,-7.97098820280248,
128.219201210677));
#69945=CARTESIAN_POINT('Ctrl Pts',(7.05516932572682,-3.755306559217,128.537432668924));
#69946=CARTESIAN_POINT('Ctrl Pts',(6.97961430616004,3.90570079659165,128.855664127171));
#69947=CARTESIAN_POINT('Ctrl Pts',(0.476824099015226,7.98450231104828,129.173895585417));
#69948=CARTESIAN_POINT('Ctrl Pts',(-5.28900758248167,5.2589567878849,129.43908846729));
#69949=CARTESIAN_POINT('Ctrl Pts',(-6.96684468589892,0.922094263057371,
129.651242772787));
#69950=CARTESIAN_POINT('Ctrl Pts',(-6.47502293851151,-3.70193269119533,
129.863397078285));
#69951=CARTESIAN_POINT('Ctrl Pts',(-1.61677841934224,-7.833624060375,130.128589960158));
#69952=CARTESIAN_POINT('Ctrl Pts',(5.72321401184765,-5.58697914349428,130.446821418405));
#69953=CARTESIAN_POINT('Ctrl Pts',(7.78919398690618,1.7905861059219,130.765052876651));
#69954=CARTESIAN_POINT('Ctrl Pts',(2.70893705762593,7.52536873469137,131.083284334898));
#69955=CARTESIAN_POINT('Ctrl Pts',(-4.87530267885765,6.34121929648078,131.401515793145));
#69956=CARTESIAN_POINT('Ctrl Pts',(-7.44160280738336,0.502767701364091,
131.666708675017));
#69957=CARTESIAN_POINT('Ctrl Pts',(-5.86481005809476,-3.87184525644711,
131.878862980515));
#69958=CARTESIAN_POINT('Ctrl Pts',(-2.46156105428565,-7.0406636676107,132.091017286013));
#69959=CARTESIAN_POINT('Ctrl Pts',(3.91566946395988,-6.97475239887046,132.356210167885));
#69960=CARTESIAN_POINT('Ctrl Pts',(7.98452298698976,-0.465733019532299,
132.674441626132));
#69961=CARTESIAN_POINT('Ctrl Pts',(4.70704716486712,6.45921423673906,132.992673084379));
#69962=CARTESIAN_POINT('Ctrl Pts',(-2.88893378327778,7.45812149077002,133.310904542626));
#69963=CARTESIAN_POINT('Ctrl Pts',(-7.83886510894448,1.59117320877073,133.629136000873));
#69964=CARTESIAN_POINT('Ctrl Pts',(-5.94832241656495,-4.49974311855476,
133.894328882745));
#69965=CARTESIAN_POINT('Ctrl Pts',(-1.8894202492775,-6.76884582695023,134.106483188243));
#69966=CARTESIAN_POINT('Ctrl Pts',(2.75789712626501,-6.9299517419192,134.318637493741));
#69967=CARTESIAN_POINT('Ctrl Pts',(7.52970753859752,-2.69872984193025,134.583830375613));
#69968=CARTESIAN_POINT('Ctrl Pts',(6.33396264917428,4.88369038065638,134.90206183386));
#69969=CARTESIAN_POINT('Ctrl Pts',(-0.681230328833862,7.96326985650064,
135.220293292107));
#69970=CARTESIAN_POINT('Ctrl Pts',(-7.07142496626254,3.73690560782156,135.538524750354));
#69971=CARTESIAN_POINT('Ctrl Pts',(-6.96192060855357,-3.93843875371134,
135.8567562086));
#69972=CARTESIAN_POINT('Ctrl Pts',(-1.54077150979294,-7.29768804889607,
136.121949090473));
#69973=CARTESIAN_POINT('Ctrl Pts',(3.01165605383282,-6.34957561737892,136.334103395971));
#69974=CARTESIAN_POINT('Ctrl Pts',(6.62617463464419,-3.42403817379246,136.546257701469));
#69975=CARTESIAN_POINT('Ctrl Pts',(7.45470471451398,2.89948547089672,136.811450583341));
#69976=CARTESIAN_POINT('Ctrl Pts',(1.58019449830633,7.8404400337463,137.129682041588));
#69977=CARTESIAN_POINT('Ctrl Pts',(-5.73575162660879,5.56586874137625,137.447913499834));
#69978=CARTESIAN_POINT('Ctrl Pts',(-7.78940231799192,-1.81513803985067,
137.766144958081));
#69979=CARTESIAN_POINT('Ctrl Pts',(-2.67411191098722,-7.53848551527781,
138.084376416328));
#69980=CARTESIAN_POINT('Ctrl Pts',(3.62165189183669,-6.52026573681974,138.349569298201));
#69981=CARTESIAN_POINT('Ctrl Pts',(6.4372271930946,-2.81944830984448,138.561723603698));
#69982=CARTESIAN_POINT('Ctrl Pts',(7.24808047400849,1.75941954822804,138.773877909196));
#69983=CARTESIAN_POINT('Ctrl Pts',(3.72740723771489,7.07715152167648,139.039070791069));
#69984=CARTESIAN_POINT('Ctrl Pts',(-3.9477607112626,6.95591115109018,139.357302249315));
#69985=CARTESIAN_POINT('Ctrl Pts',(-7.98014753412108,0.441573212544696,
139.675533707562));
#69986=CARTESIAN_POINT('Ctrl Pts',(-4.69110611854187,-6.47788838741673,
139.993765165809));
#69987=CARTESIAN_POINT('Ctrl Pts',(2.92382844266543,-7.44519077085319,140.311996624056));
#69988=CARTESIAN_POINT('Ctrl Pts',(7.00971395453912,-2.54835986075936,140.577189505928));
#69989=CARTESIAN_POINT('Ctrl Pts',(6.70899796654445,2.09201553347577,140.789343811426));
#69990=CARTESIAN_POINT('Ctrl Pts',(4.31892338446397,6.08088221424489,141.001498116924));
#69991=CARTESIAN_POINT('Ctrl Pts',(-1.82606445310679,7.78749812132479,141.266690998797));
#69992=CARTESIAN_POINT('Ctrl Pts',(-7.54158359928277,2.6634622937598,141.584922457043));
#69993=CARTESIAN_POINT('Ctrl Pts',(-6.31481780085691,-4.89906294206899,
141.90315391529));
#69994=CARTESIAN_POINT('Ctrl Pts',(0.705510731853791,-7.96691716930022,
142.221385373537));
#69995=CARTESIAN_POINT('Ctrl Pts',(7.08929314563132,-3.70426255438861,142.539616831784));
#69996=CARTESIAN_POINT('Ctrl Pts',(6.96349635444189,2.67206778096168,142.804809713656));
#69997=CARTESIAN_POINT('Ctrl Pts',(3.69381931185978,5.97853507129855,143.016964019154));
#69998=CARTESIAN_POINT('Ctrl Pts',(-0.726210311352885,7.4231291439697,143.229118324652));
#69999=CARTESIAN_POINT('Ctrl Pts',(-6.48488964979702,4.68250409572428,143.494311206524));
#70000=CARTESIAN_POINT('Ctrl Pts',(-7.44054713237905,-2.93390063673488,
143.812542664771));
#70001=CARTESIAN_POINT('Ctrl Pts',(-1.55565991875539,-7.83949384752223,
144.130774123018));
#70002=CARTESIAN_POINT('Ctrl Pts',(5.7564756520609,-5.55270228289268,144.449005581264));
#70003=CARTESIAN_POINT('Ctrl Pts',(7.78148983349211,1.8515005667527,144.767237039512));
#70004=CARTESIAN_POINT('Ctrl Pts',(3.50564254954319,6.5833652502107,145.032429921384));
#70005=CARTESIAN_POINT('Ctrl Pts',(-1.13107777388849,6.93598196205286,145.244584226882));
#70006=CARTESIAN_POINT('Ctrl Pts',(-5.41555070126417,5.12855128734094,145.456738532379));
#70007=CARTESIAN_POINT('Ctrl Pts',(-7.96656314127199,-0.716596178392399,
145.721931414252));
#70008=CARTESIAN_POINT('Ctrl Pts',(-3.69415225913557,-7.09385323224563,
146.040162872499));
#70009=CARTESIAN_POINT('Ctrl Pts',(3.96566476044414,-6.93910978213129,146.358394330745));
#70010=CARTESIAN_POINT('Ctrl Pts',(7.98716182589273,-0.418043648415986,
146.676625788992));
#70011=CARTESIAN_POINT('Ctrl Pts',(4.66128955204064,6.50015524624547,146.994857247239));
#70012=CARTESIAN_POINT('Ctrl Pts',(-1.66973597467493,7.26926470625684,147.260050129111));
#70013=CARTESIAN_POINT('Ctrl Pts',(-5.40182421568405,4.49527282901404,147.472204434609));
#70014=CARTESIAN_POINT('Ctrl Pts',(-7.45164225692231,0.321334579947432,
147.684358740107));
#70015=CARTESIAN_POINT('Ctrl Pts',(-5.54516633579186,-5.76461334347584,
147.949551621979));
#70016=CARTESIAN_POINT('Ctrl Pts',(1.86212403554058,-7.77830379904534,148.267783080226));
#70017=CARTESIAN_POINT('Ctrl Pts',(7.54408560015588,-2.6390370489041,148.586014538473));
#70018=CARTESIAN_POINT('Ctrl Pts',(6.30468538270765,4.92142733395752,148.90424599672));
#70019=CARTESIAN_POINT('Ctrl Pts',(-0.742622404887226,7.96417992471234,
149.222477454967));
#70020=CARTESIAN_POINT('Ctrl Pts',(-6.02705982360509,4.39372101266743,149.487670336839));
#70021=CARTESIAN_POINT('Ctrl Pts',(-7.02604472395381,-0.14781019150323,
149.699824642337));
#70022=CARTESIAN_POINT('Ctrl Pts',(-5.83694466737079,-4.643318603884,149.911978947835));
#70023=CARTESIAN_POINT('Ctrl Pts',(-0.407007019060977,-7.988355204186,150.177171829707));
#70024=CARTESIAN_POINT('Ctrl Pts',(6.50606889048119,-4.65193452158739,150.495403287954));
#70025=CARTESIAN_POINT('Ctrl Pts',(7.42645459139895,2.95401266902674,150.813634746201));
#70026=CARTESIAN_POINT('Ctrl Pts',(1.53328191626781,7.84967999940523,151.131866204448));
#70027=CARTESIAN_POINT('Ctrl Pts',(-5.78257511906035,5.52641320801365,151.450097662695));
#70028=CARTESIAN_POINT('Ctrl Pts',(-7.43175585864685,-0.634639310737093,
151.715290544567));
#70029=CARTESIAN_POINT('Ctrl Pts',(-5.20769272559132,-4.71821693561009,
151.927444850065));
#70030=CARTESIAN_POINT('Ctrl Pts',(-1.3632546876904,-7.33369535060035,152.139599155562));
#70031=CARTESIAN_POINT('Ctrl Pts',(4.93206728293985,-6.29700846122896,152.404792037435));
#70032=CARTESIAN_POINT('Ctrl Pts',(7.95995131862168,0.751309809408091,152.723023495682));
#70033=CARTESIAN_POINT('Ctrl Pts',(3.67501525946745,7.10394148213151,153.041254953929));
#70034=CARTESIAN_POINT('Ctrl Pts',(-3.99821329042567,6.92411285836137,153.359486412175));
#70035=CARTESIAN_POINT('Ctrl Pts',(-7.30894614683688,1.48602192463945,153.624679294048));
#70036=CARTESIAN_POINT('Ctrl Pts',(-6.32629632928619,-3.07755403250854,
153.836847387308));
#70037=CARTESIAN_POINT('Ctrl Pts',(-4.84151887665322,-4.85041839127279,
153.94293832782));
#70038=CARTESIAN_POINT('Ctrl Pts',(-3.92409368265873,-5.50444119324983,
153.995990691956));
#70039=CARTESIAN_POINT('Ctrl Pts',(-3.08954740555787,6.44311816685693,-0.44193303580599));
#70040=CARTESIAN_POINT('Ctrl Pts',(-4.16319062916384,5.92829528072251,-0.388891808959014));
#70041=CARTESIAN_POINT('Ctrl Pts',(-6.03043332774519,4.35125203191573,-0.282812005737566));
#70042=CARTESIAN_POINT('Ctrl Pts',(-7.88075233109425,-0.222852525913893,
-0.0706550497671821));
#70043=CARTESIAN_POINT('Ctrl Pts',(-5.41860073246465,-6.48603369603572,
0.194537832105166));
#70044=CARTESIAN_POINT('Ctrl Pts',(2.5395922108837,-8.06399520298082,0.512769290351983));
#70045=CARTESIAN_POINT('Ctrl Pts',(8.15320687002302,-2.22505886794282,0.831000748598799));
#70046=CARTESIAN_POINT('Ctrl Pts',(6.27744628296401,5.66372553892937,1.14923220684562));
#70047=CARTESIAN_POINT('Ctrl Pts',(-0.0905190406078649,7.88427553034339,
1.41442508871796));
#70048=CARTESIAN_POINT('Ctrl Pts',(-4.56808658365247,5.85731890654616,1.62657939421585));
#70049=CARTESIAN_POINT('Ctrl Pts',(-7.6242973326671,2.00783018015323,1.83873369971372));
#70050=CARTESIAN_POINT('Ctrl Pts',(-7.0234902137228,-4.70709375975071,2.10392658158607));
#70051=CARTESIAN_POINT('Ctrl Pts',(0.174066138808668,-8.45242981178917,
2.42215803983288));
#70052=CARTESIAN_POINT('Ctrl Pts',(7.19841503602263,-4.42222996039016,2.74038949807971));
#70053=CARTESIAN_POINT('Ctrl Pts',(7.6184358430781,3.66529927552298,3.05862095632652));
#70054=CARTESIAN_POINT('Ctrl Pts',(1.02395302145998,8.39271879730463,3.37685241457334));
#70055=CARTESIAN_POINT('Ctrl Pts',(-5.23695462670971,5.89336609917461,3.64204529644568));
#70056=CARTESIAN_POINT('Ctrl Pts',(-7.2900284264346,1.42732283980118,3.85419960194356));
#70057=CARTESIAN_POINT('Ctrl Pts',(-7.07280455631803,-3.48321488042714,
4.06635390744144));
#70058=CARTESIAN_POINT('Ctrl Pts',(-2.2167783250272,-8.1591849761286,4.33154678931379));
#70059=CARTESIAN_POINT('Ctrl Pts',(5.67364854670524,-6.26775735988919,4.6497782475606));
#70060=CARTESIAN_POINT('Ctrl Pts',(8.33459469622863,1.38096864477367,4.96800970580742));
#70061=CARTESIAN_POINT('Ctrl Pts',(3.34892244672672,7.76271866306914,5.28624116405423));
#70062=CARTESIAN_POINT('Ctrl Pts',(-4.72987836523322,7.00818389443088,5.60447262230106));
#70063=CARTESIAN_POINT('Ctrl Pts',(-7.81826678136539,1.0158975263293,5.8696655041734));
#70064=CARTESIAN_POINT('Ctrl Pts',(-6.44009876682224,-3.7022866893791,6.08181980967128));
#70065=CARTESIAN_POINT('Ctrl Pts',(-3.05631451379665,-7.26748127780818,
6.29397411516916));
#70066=CARTESIAN_POINT('Ctrl Pts',(3.67611324854931,-7.61397296209672,6.55916699704151));
#70067=CARTESIAN_POINT('Ctrl Pts',(8.39347630220861,-1.01224335435673,6.87739845528832));
#70068=CARTESIAN_POINT('Ctrl Pts',(5.38742321439901,6.50755034044391,7.19562991353514));
#70069=CARTESIAN_POINT('Ctrl Pts',(-2.56134958238959,8.05695782776883,7.51386137178195));
#70070=CARTESIAN_POINT('Ctrl Pts',(-8.16638379749588,2.19010693620455,7.83209283002878));
#70071=CARTESIAN_POINT('Ctrl Pts',(-6.56916827614357,-4.35928558519119,
8.09728571190112));
#70072=CARTESIAN_POINT('Ctrl Pts',(-2.43496001820217,-7.01803167674481,
8.309440017399));
#70073=CARTESIAN_POINT('Ctrl Pts',(2.4575588939521,-7.49117794035554,8.52159432289688));
#70074=CARTESIAN_POINT('Ctrl Pts',(7.76796194168394,-3.33843676059349,8.78678720476922));
#70075=CARTESIAN_POINT('Ctrl Pts',(7.00107523470319,4.73920105696399,9.10501866301604));
#70076=CARTESIAN_POINT('Ctrl Pts',(-0.199216385661401,8.44587788003586,
9.42325012126286));
#70077=CARTESIAN_POINT('Ctrl Pts',(-7.21673588746628,4.40383971450563,9.74148157950967));
#70078=CARTESIAN_POINT('Ctrl Pts',(-7.60192050859073,-3.7009724819277,10.0597130377566));
#70079=CARTESIAN_POINT('Ctrl Pts',(-2.10162734494506,-7.5987173362343,10.3249059196288));
#70080=CARTESIAN_POINT('Ctrl Pts',(2.7631423545712,-6.89542190392953,10.5370602251268));
#70081=CARTESIAN_POINT('Ctrl Pts',(6.76739677982186,-4.04471055546355,10.7492145306247));
#70082=CARTESIAN_POINT('Ctrl Pts',(8.05404140503811,2.5727047589792,11.0144074124969));
#70083=CARTESIAN_POINT('Ctrl Pts',(2.17862688248009,8.16876159569394,11.3326388707437));
#70084=CARTESIAN_POINT('Ctrl Pts',(-5.6882536018224,6.24630381060562,11.6508703289905));
#70085=CARTESIAN_POINT('Ctrl Pts',(-8.33641596472343,-1.40685818882059,
11.9691017872373));
#70086=CARTESIAN_POINT('Ctrl Pts',(-3.31303691185947,-7.7788289061784,12.2873332454843));
#70087=CARTESIAN_POINT('Ctrl Pts',(3.3955670207164,-7.11529811468617,12.5525261273565));
#70088=CARTESIAN_POINT('Ctrl Pts',(6.607494252704,-3.39452774407344,12.7646804328544));
#70089=CARTESIAN_POINT('Ctrl Pts',(7.76167381937667,1.38338793352998,12.9768347383524));
#70090=CARTESIAN_POINT('Ctrl Pts',(4.3941922927382,7.22339718037018,13.2420276202246));
#70091=CARTESIAN_POINT('Ctrl Pts',(-3.71119940327893,7.59618852382226,13.5602590784714));
#70092=CARTESIAN_POINT('Ctrl Pts',(-8.3904362061758,0.986468754258332,13.8784905367182));
#70093=CARTESIAN_POINT('Ctrl Pts',(-5.37182327508643,-6.52829195131364,
14.1967219949651));
#70094=CARTESIAN_POINT('Ctrl Pts',(2.59900782415898,-8.04559202674982,14.5149534532119));
#70095=CARTESIAN_POINT('Ctrl Pts',(7.22916614717721,-3.14587022452307,14.7801463350843));
#70096=CARTESIAN_POINT('Ctrl Pts',(7.21462658934175,1.76945248061757,14.9923006405821));
#70097=CARTESIAN_POINT('Ctrl Pts',(4.95326237263331,6.13372109904654,15.20445494608));
#70098=CARTESIAN_POINT('Ctrl Pts',(-1.41851003486382,8.33511979589558,15.4696478279523));
#70099=CARTESIAN_POINT('Ctrl Pts',(-7.78279220363034,3.30200342450728,15.7878792861993));
#70100=CARTESIAN_POINT('Ctrl Pts',(-6.98187982577724,-4.75666841722636,
16.1061107444459));
#70101=CARTESIAN_POINT('Ctrl Pts',(0.224594842153657,-8.45130985452697,
16.4243422026929));
#70102=CARTESIAN_POINT('Ctrl Pts',(7.23771676190491,-4.37056618819351,16.7425736609397));
#70103=CARTESIAN_POINT('Ctrl Pts',(7.52096906921939,2.36481857927387,17.0077665428119));
#70104=CARTESIAN_POINT('Ctrl Pts',(4.28708610892083,6.06652219970378,17.2199208483098));
#70105=CARTESIAN_POINT('Ctrl Pts',(-0.281908331501364,7.87895109425512,
17.4320751538077));
#70106=CARTESIAN_POINT('Ctrl Pts',(-6.53623961524628,5.36320467845715,17.6972680356801));
#70107=CARTESIAN_POINT('Ctrl Pts',(-8.04134995603776,-2.6099371610976,18.015499493927));
#70108=CARTESIAN_POINT('Ctrl Pts',(-2.15268059899722,-8.16936390251621,
18.3337309521738));
#70109=CARTESIAN_POINT('Ctrl Pts',(5.71097687179014,-6.23376485522393,18.6519624104205));
#70110=CARTESIAN_POINT('Ctrl Pts',(8.33044027974437,1.44573769285852,18.9701938686673));
#70111=CARTESIAN_POINT('Ctrl Pts',(4.12801234393877,6.71690827251071,19.2353867505397));
#70112=CARTESIAN_POINT('Ctrl Pts',(-0.740832893651014,7.39141160594412,
19.4475410560375));
#70113=CARTESIAN_POINT('Ctrl Pts',(-5.37896326430388,5.76403477212821,19.6596953615354));
#70114=CARTESIAN_POINT('Ctrl Pts',(-8.45165952544785,-0.236313344621609,
19.9248882434079));
#70115=CARTESIAN_POINT('Ctrl Pts',(-4.36019707337875,-7.24318732200448,
20.2431197016547));
#70116=CARTESIAN_POINT('Ctrl Pts',(3.73118465974708,-7.57963068809433,20.5613511599015));
#70117=CARTESIAN_POINT('Ctrl Pts',(8.39937144392063,-0.962102098219144,
20.8795826181483));
#70118=CARTESIAN_POINT('Ctrl Pts',(5.34181870698094,6.55372913940518,21.197814076395));
#70119=CARTESIAN_POINT('Ctrl Pts',(-1.28738765542055,7.77817302955547,21.4630069582675));
#70120=CARTESIAN_POINT('Ctrl Pts',(-5.40579452639309,5.09501564700433,21.6751612637654));
#70121=CARTESIAN_POINT('Ctrl Pts',(-7.84069466388574,0.825136255867873,
21.8873155692632));
#70122=CARTESIAN_POINT('Ctrl Pts',(-6.22634521833476,-5.7200540166208,22.1525084511356));
#70123=CARTESIAN_POINT('Ctrl Pts',(1.45715369581518,-8.32777186329684,22.4707399093824));
#70124=CARTESIAN_POINT('Ctrl Pts',(7.78702502643142,-3.27639765150152,22.7889713676291));
#70125=CARTESIAN_POINT('Ctrl Pts',(6.97264937688021,4.78092478161278,23.107202825876));
#70126=CARTESIAN_POINT('Ctrl Pts',(-0.263928110367578,8.45084224698918,
23.4254342841228));
#70127=CARTESIAN_POINT('Ctrl Pts',(-6.07205589142636,5.02866581753332,23.6906271659952));
#70128=CARTESIAN_POINT('Ctrl Pts',(-7.42228714546869,0.302411036523226,
23.902781471493));
#70129=CARTESIAN_POINT('Ctrl Pts',(-6.46102277639563,-4.51802250281368,
24.1149357769908));
#70130=CARTESIAN_POINT('Ctrl Pts',(-0.950548267340358,-8.40136005194374,
24.3801286588633));
#70131=CARTESIAN_POINT('Ctrl Pts',(6.56059897106672,-5.33231865525546,24.6983601171101));
#70132=CARTESIAN_POINT('Ctrl Pts',(8.02775655195335,2.63204579663869,25.0165915753568));
#70133=CARTESIAN_POINT('Ctrl Pts',(2.12980675111955,8.18162601829445,25.3348230336038));
#70134=CARTESIAN_POINT('Ctrl Pts',(-5.74036823307002,6.20762154771861,25.6530544918505));
#70135=CARTESIAN_POINT('Ctrl Pts',(-7.88183268470767,-0.184543174642897,
25.9182473737229));
#70136=CARTESIAN_POINT('Ctrl Pts',(-5.80236750001345,-4.63835426628759,
26.1304016792208));
#70137=CARTESIAN_POINT('Ctrl Pts',(-1.91589231730585,-7.6476597257934,26.3425559847187));
#70138=CARTESIAN_POINT('Ctrl Pts',(4.79095222080362,-6.96657516638674,26.607748866591));
#70139=CARTESIAN_POINT('Ctrl Pts',(8.44980016043421,0.275605422791958,26.9259803248378));
#70140=CARTESIAN_POINT('Ctrl Pts',(4.33543727924364,7.25096710313725,27.2442117830847));
#70141=CARTESIAN_POINT('Ctrl Pts',(-3.75649528803494,7.57389095850464,27.5624432413314));
#70142=CARTESIAN_POINT('Ctrl Pts',(-8.40442114458738,0.923091520571846,
27.8806746995783));
#70143=CARTESIAN_POINT('Ctrl Pts',(-5.83005137872459,-5.30733865270204,
28.1458675814506));
#70144=CARTESIAN_POINT('Ctrl Pts',(-1.33968524960494,-7.30664371218358,
28.3580218869484));
#70145=CARTESIAN_POINT('Ctrl Pts',(3.56789413603829,-7.030467558211,28.5701761924464));
#70146=CARTESIAN_POINT('Ctrl Pts',(8.18521430748699,-2.11864566915973,28.8353690743186));
#70147=CARTESIAN_POINT('Ctrl Pts',(6.19917809397479,5.74850172301705,29.1536005325656));
#70148=CARTESIAN_POINT('Ctrl Pts',(-1.48094927695439,8.31741123019191,29.4718319908123));
#70149=CARTESIAN_POINT('Ctrl Pts',(-7.80237196108085,3.25546815086346,29.7900634490592));
#70150=CARTESIAN_POINT('Ctrl Pts',(-6.95088340951852,-4.81369011863248,
30.108294907306));
#70151=CARTESIAN_POINT('Ctrl Pts',(-0.92194426360296,-7.82990175084229,
30.3734877891782));
#70152=CARTESIAN_POINT('Ctrl Pts',(3.77935100285112,-6.39517825412621,30.5856420946763));
#70153=CARTESIAN_POINT('Ctrl Pts',(7.30365686831716,-2.96882788368026,30.797796400174));
#70154=CARTESIAN_POINT('Ctrl Pts',(7.56928208179731,3.76727507585018,31.0629892820465));
#70155=CARTESIAN_POINT('Ctrl Pts',(0.911383413585489,8.40502595913824,31.3812207402932));
#70156=CARTESIAN_POINT('Ctrl Pts',(-6.57177213448138,5.30889360841674,31.6994521985401));
#70157=CARTESIAN_POINT('Ctrl Pts',(-8.02562084627201,-2.65791104671155,
32.0176836567869));
#70158=CARTESIAN_POINT('Ctrl Pts',(-2.09188894873834,-8.19209334401688,
32.3359151150337));
#70159=CARTESIAN_POINT('Ctrl Pts',(4.43785238624996,-6.51634934997266,32.6011079969061));
#70160=CARTESIAN_POINT('Ctrl Pts',(7.04676415458615,-2.35051352994202,32.8132623024038));
#70161=CARTESIAN_POINT('Ctrl Pts',(7.46112804553437,2.54733408511215,33.0254166079019));
#70162=CARTESIAN_POINT('Ctrl Pts',(3.24492014212853,7.80748909715203,33.2906094897741));
#70163=CARTESIAN_POINT('Ctrl Pts',(-4.82292670845914,6.94366323097387,33.6088409480209));
#70164=CARTESIAN_POINT('Ctrl Pts',(-8.44287682142809,-0.30061821506101,
33.9270724062678));
#70165=CARTESIAN_POINT('Ctrl Pts',(-4.31686528271657,-7.26909590191398,
34.2453038645147));
#70166=CARTESIAN_POINT('Ctrl Pts',(3.79198779968982,-7.55693200035196,34.5635353227614));
#70167=CARTESIAN_POINT('Ctrl Pts',(7.62340536575552,-2.01023214639604,34.8287282046339));
#70168=CARTESIAN_POINT('Ctrl Pts',(6.86174558348796,2.845741810545,35.0408825101316));
#70169=CARTESIAN_POINT('Ctrl Pts',(3.96315757784307,6.81547684804362,35.2530368156296));
#70170=CARTESIAN_POINT('Ctrl Pts',(-2.66923038574688,8.02256828445513,35.5182296975018));
#70171=CARTESIAN_POINT('Ctrl Pts',(-8.19433312038786,2.08038116999304,35.8364611557488));
#70172=CARTESIAN_POINT('Ctrl Pts',(-6.17755021440263,-5.76284770591486,
36.1546926139953));
#70173=CARTESIAN_POINT('Ctrl Pts',(1.50685855823589,-8.31892170811928,36.4729240722423));
#70174=CARTESIAN_POINT('Ctrl Pts',(7.81805028258378,-3.21939163661875,36.791155530489));
#70175=CARTESIAN_POINT('Ctrl Pts',(7.07401192966089,3.48076110528274,37.0563484123616));
#70176=CARTESIAN_POINT('Ctrl Pts',(3.31494171537135,6.64777860104349,37.2685027178592));
#70177=CARTESIAN_POINT('Ctrl Pts',(-1.47648862131544,7.74450282485324,37.4806570233573));
#70178=CARTESIAN_POINT('Ctrl Pts',(-7.27564087051258,4.30713856919719,37.7458499052295));
#70179=CARTESIAN_POINT('Ctrl Pts',(-7.55107762627309,-3.80214515534913,
38.0640813634764));
#70180=CARTESIAN_POINT('Ctrl Pts',(-0.88564717289864,-8.40167658376415,
38.3823128217233));
#70181=CARTESIAN_POINT('Ctrl Pts',(6.59232492751021,-5.29304573478011,38.70054427997));
#70182=CARTESIAN_POINT('Ctrl Pts',(8.0138036740729,2.69543009635854,39.0187757382169));
#70183=CARTESIAN_POINT('Ctrl Pts',(3.05883722745604,7.26641985223558,39.2839686200891));
#70184=CARTESIAN_POINT('Ctrl Pts',(-1.85595651526812,7.19285925889241,39.4961229255871));
#70185=CARTESIAN_POINT('Ctrl Pts',(-6.19275653750488,4.87925292644519,39.7082772310848));
#70186=CARTESIAN_POINT('Ctrl Pts',(-8.317485720007,-1.51849400012624,39.9734701129573));
#70187=CARTESIAN_POINT('Ctrl Pts',(-3.20831135435621,-7.82188080667661,
40.2917015712041));
#70188=CARTESIAN_POINT('Ctrl Pts',(4.84016231529167,-6.92425946182438,40.6099330294509));
#70189=CARTESIAN_POINT('Ctrl Pts',(8.44800366551446,0.326060067780617,40.9281644876977));
#70190=CARTESIAN_POINT('Ctrl Pts',(4.28334222170055,7.28967572274216,41.2463959459445));
#70191=CARTESIAN_POINT('Ctrl Pts',(-2.45495818169829,7.4920306312205,41.5115888278169));
#70192=CARTESIAN_POINT('Ctrl Pts',(-6.11756318896782,4.21393160051117,41.7237431333147));
#70193=CARTESIAN_POINT('Ctrl Pts',(-7.87499796254952,-0.376496670469604,
41.9358974388127));
#70194=CARTESIAN_POINT('Ctrl Pts',(-5.28433232576479,-6.60016852828897,
42.2010903206851));
#70195=CARTESIAN_POINT('Ctrl Pts',(2.70630770751061,-8.00943067218986,42.5193217789319));
#70196=CARTESIAN_POINT('Ctrl Pts',(8.19462382668053,-2.05442952476689,42.8375532371787));
#70197=CARTESIAN_POINT('Ctrl Pts',(6.16473930713995,5.78541877268626,43.1557846954255));
#70198=CARTESIAN_POINT('Ctrl Pts',(-1.54566350454616,8.31247959766842,43.4740161536723));
#70199=CARTESIAN_POINT('Ctrl Pts',(-6.76599224978972,4.04705961517972,43.7392090355446));
#70200=CARTESIAN_POINT('Ctrl Pts',(-7.38198296145935,-0.829533882083435,
43.9513633410425));
#70201=CARTESIAN_POINT('Ctrl Pts',(-5.6990298339995,-5.44778868938746,44.1635176465404));
#70202=CARTESIAN_POINT('Ctrl Pts',(0.337781924161787,-8.44821259809727,
44.4287105284128));
#70203=CARTESIAN_POINT('Ctrl Pts',(7.29502137845032,-4.27290816520776,44.7469419866596));
#70204=CARTESIAN_POINT('Ctrl Pts',(7.53428100585627,3.82193014821406,45.0651734449063));
#70205=CARTESIAN_POINT('Ctrl Pts',(0.861174981281068,8.41031858801809,45.3834049031532));
#70206=CARTESIAN_POINT('Ctrl Pts',(-6.61739999361422,5.26273788587781,45.7016363613999));
#70207=CARTESIAN_POINT('Ctrl Pts',(-7.76215359514146,-1.38069338321955,
45.9668292432723));
#70208=CARTESIAN_POINT('Ctrl Pts',(-5.02973675869332,-5.46658458665463,
46.1789835487703));
#70209=CARTESIAN_POINT('Ctrl Pts',(-0.730927478072492,-7.85003743142875,
46.3911378542681));
#70210=CARTESIAN_POINT('Ctrl Pts',(5.79440616976952,-6.15721120887338,46.6563307361405));
#70211=CARTESIAN_POINT('Ctrl Pts',(8.30967429282036,1.55704664271416,46.9745621943871));
#70212=CARTESIAN_POINT('Ctrl Pts',(3.18265660064284,7.82580585597539,47.2927936526342));
#70213=CARTESIAN_POINT('Ctrl Pts',(-4.86430609374981,6.91473841346546,47.6110251108809));
#70214=CARTESIAN_POINT('Ctrl Pts',(-8.44706378669732,-0.365384885300918,
47.9292565691279));
#70215=CARTESIAN_POINT('Ctrl Pts',(-4.95539139693606,-6.13200120321307,
48.194449451));
#70216=CARTESIAN_POINT('Ctrl Pts',(-0.213264087965808,-7.42538331223274,
48.406603756498));
#70217=CARTESIAN_POINT('Ctrl Pts',(4.59527927258509,-6.40630557029426,48.6187580619957));
#70218=CARTESIAN_POINT('Ctrl Pts',(8.41216831688165,-0.849598104630865,
48.8839509438682));
#70219=CARTESIAN_POINT('Ctrl Pts',(5.25315602768194,6.62415525551567,49.202182402115));
#70220=CARTESIAN_POINT('Ctrl Pts',(-2.72825152258647,7.99557277263729,49.5204138603617));
#70221=CARTESIAN_POINT('Ctrl Pts',(-8.20661039441647,2.03141008528623,49.8386453186087));
#70222=CARTESIAN_POINT('Ctrl Pts',(-6.13824495963909,-5.81449409204312,
50.1568767768553));
#70223=CARTESIAN_POINT('Ctrl Pts',(0.279173134727941,-7.87904848404171,
50.4220696587278));
#70224=CARTESIAN_POINT('Ctrl Pts',(4.70769337698525,-5.74625286365732,50.6342239642257));
#70225=CARTESIAN_POINT('Ctrl Pts',(7.67011396254657,-1.82392282034684,50.8463782697236));
#70226=CARTESIAN_POINT('Ctrl Pts',(6.90854423367506,4.87425987225694,51.1115711515959));
#70227=CARTESIAN_POINT('Ctrl Pts',(-0.377048842699031,8.44588155674506,
51.4298026098427));
#70228=CARTESIAN_POINT('Ctrl Pts',(-7.3025032886826,4.24805673829975,51.7480340680896));
#70229=CARTESIAN_POINT('Ctrl Pts',(-7.52823776577549,-3.84717003033372,
52.0662655263364));
#70230=CARTESIAN_POINT('Ctrl Pts',(-0.822106580473215,-8.41489949442549,
52.3844969845832));
#70231=CARTESIAN_POINT('Ctrl Pts',(5.37696195411409,-5.76590173321082,52.6496898664556));
#70232=CARTESIAN_POINT('Ctrl Pts',(7.32220357060287,-1.25185213801433,52.8618441719534));
#70233=CARTESIAN_POINT('Ctrl Pts',(6.9871182240826,3.65205717038036,53.0739984774512));
#70234=CARTESIAN_POINT('Ctrl Pts',(2.02020672062951,8.21006440515927,53.3391913593236));
#70235=CARTESIAN_POINT('Ctrl Pts',(-5.82252560851519,6.12970444952542,53.6574228175704));
#70236=CARTESIAN_POINT('Ctrl Pts',(-8.29902867471625,-1.58071610014923,
53.9756542758171));
#70237=CARTESIAN_POINT('Ctrl Pts',(-3.16154432641485,-7.8409003674617,54.2938857340642));
#70238=CARTESIAN_POINT('Ctrl Pts',(4.89680770770741,-6.89258057658212,54.6121171923107));
#70239=CARTESIAN_POINT('Ctrl Pts',(7.84040774518007,-0.827858105205332,
54.8773100741832));
#70240=CARTESIAN_POINT('Ctrl Pts',(6.34933559551319,3.85587038168426,55.0894643796811));
#70241=CARTESIAN_POINT('Ctrl Pts',(2.88091318290485,7.33877931849697,55.3016186851791));
#70242=CARTESIAN_POINT('Ctrl Pts',(-3.85789369862079,7.52349978009444,55.5668115670513));
#70243=CARTESIAN_POINT('Ctrl Pts',(-8.41536367707005,0.810392055117173,
55.8850430252982));
#70244=CARTESIAN_POINT('Ctrl Pts',(-5.22959850487317,-6.63504633072462,
56.203274483545));
#70245=CARTESIAN_POINT('Ctrl Pts',(2.75408926280945,-7.99312663685644,56.5215059417917));
#70246=CARTESIAN_POINT('Ctrl Pts',(8.21662165708924,-1.99336932734302,56.8397374000387));
#70247=CARTESIAN_POINT('Ctrl Pts',(6.46259081968553,4.51577928494635,57.1049302819109));
#70248=CARTESIAN_POINT('Ctrl Pts',(2.2657281167326,7.07448054671492,57.3170845874089));
#70249=CARTESIAN_POINT('Ctrl Pts',(-2.63674197143089,7.43000231689924,57.5292388929067));
#70250=CARTESIAN_POINT('Ctrl Pts',(-7.8458904765042,3.1509356327352,57.794431774779));
#70251=CARTESIAN_POINT('Ctrl Pts',(-6.88525000770043,-4.90595693334218,
58.1126632330257));
#70252=CARTESIAN_POINT('Ctrl Pts',(0.401976697758393,-8.43865836892884,
58.4308946912727));
#70253=CARTESIAN_POINT('Ctrl Pts',(7.3204077721116,-4.22926839422082,58.7491261495195));
#70254=CARTESIAN_POINT('Ctrl Pts',(7.5108538442389,3.88245634378822,59.0673576077664));
#70255=CARTESIAN_POINT('Ctrl Pts',(1.91854708879243,7.64699416248759,59.3325504896385));
#70256=CARTESIAN_POINT('Ctrl Pts',(-2.92793093379394,6.82707985537983,59.5447047951366));
#70257=CARTESIAN_POINT('Ctrl Pts',(-6.86257418017123,3.88103314526963,59.7568591006344));
#70258=CARTESIAN_POINT('Ctrl Pts',(-7.98993837505287,-2.76537113129454,
60.0220519825068));
#70259=CARTESIAN_POINT('Ctrl Pts',(-1.98183548353321,-8.21872308917607,
60.3402834407536));
#70260=CARTESIAN_POINT('Ctrl Pts',(5.83661085443811,-6.10790586591585,60.6585148990004));
#70261=CARTESIAN_POINT('Ctrl Pts',(8.30022793095247,1.6066416509548,60.9767463572473));
#70262=CARTESIAN_POINT('Ctrl Pts',(3.1252821513995,7.85614435999515,61.294977815494));
#70263=CARTESIAN_POINT('Ctrl Pts',(-3.5654532925281,7.03170572989474,61.5601706973665));
#70264=CARTESIAN_POINT('Ctrl Pts',(-6.68710439400672,3.23487769914977,61.7723250028642));
#70265=CARTESIAN_POINT('Ctrl Pts',(-7.72621513627836,-1.56937641150137,
61.9844793083622));
#70266=CARTESIAN_POINT('Ctrl Pts',(-4.21946379145455,-7.32683547266784,
62.2496721902343));
#70267=CARTESIAN_POINT('Ctrl Pts',(3.89254266914332,-7.5048779250062,62.5679036484814));
#70268=CARTESIAN_POINT('Ctrl Pts',(8.41170550821265,-0.784697888450407,
62.886135106728));
#70269=CARTESIAN_POINT('Ctrl Pts',(5.2135049805116,6.6554073442974,63.2043665649751));
#70270=CARTESIAN_POINT('Ctrl Pts',(-2.79146370955416,7.98085979636165,63.5225980232217));
#70271=CARTESIAN_POINT('Ctrl Pts',(-7.30262579890221,2.97136317104487,63.7877909050942));
#70272=CARTESIAN_POINT('Ctrl Pts',(-7.17005477688813,-1.94219293614828,
63.999945210592));
#70273=CARTESIAN_POINT('Ctrl Pts',(-4.80453993183803,-6.25089903105207,
64.2120995160899));
#70274=CARTESIAN_POINT('Ctrl Pts',(1.61825901095675,-8.29865233061352,64.4772923979622));
#70275=CARTESIAN_POINT('Ctrl Pts',(7.85984155839847,-3.11415667191275,64.7955238562089));
#70276=CARTESIAN_POINT('Ctrl Pts',(6.86564067621341,4.92295830148474,65.1137553144559));
#70277=CARTESIAN_POINT('Ctrl Pts',(-0.427478278208905,8.44347934337543,
65.4319867727027));
#70278=CARTESIAN_POINT('Ctrl Pts',(-7.34058357188119,4.19550063224483,65.7502182309494));
#70279=CARTESIAN_POINT('Ctrl Pts',(-7.46201190359825,-2.54474379920436,
66.0154111128219));
#70280=CARTESIAN_POINT('Ctrl Pts',(-4.14016947758362,-6.1677220755876,66.2275654183197));
#70281=CARTESIAN_POINT('Ctrl Pts',(0.471030721693415,-7.86990932045876,
66.4397197238176));
#70282=CARTESIAN_POINT('Ctrl Pts',(6.66314575093835,-5.20469801551421,66.7049126056898));
#70283=CARTESIAN_POINT('Ctrl Pts',(7.97635649386006,2.80228802645955,67.0231440639369));
#70284=CARTESIAN_POINT('Ctrl Pts',(1.95588221857694,8.21870215301671,67.3413755221834));
#70285=CARTESIAN_POINT('Ctrl Pts',(-5.8590264634452,6.09482485400949,67.6596069804306));
#70286=CARTESIAN_POINT('Ctrl Pts',(-8.29332032393845,-1.6453664441987,67.9778384386769));
#70287=CARTESIAN_POINT('Ctrl Pts',(-3.96552333346447,-6.814100626219,68.2430313205496));
#70288=CARTESIAN_POINT('Ctrl Pts',(0.918115258484746,-7.37148989536762,
68.4551856260474));
#70289=CARTESIAN_POINT('Ctrl Pts',(5.51582858788926,-5.63320314221727,68.6673399315454));
#70290=CARTESIAN_POINT('Ctrl Pts',(8.44354750738623,0.439201798094404,68.9325328134176));
#70291=CARTESIAN_POINT('Ctrl Pts',(4.18500313876025,7.34580355275531,69.2507642716645));
#70292=CARTESIAN_POINT('Ctrl Pts',(-3.91212454590034,7.48784494118263,69.5689957299112));
#70293=CARTESIAN_POINT('Ctrl Pts',(-8.42005303224499,0.760123691181521,
69.8872271881581));
#70294=CARTESIAN_POINT('Ctrl Pts',(-5.18289822219567,-6.68011667524811,
70.2054586464048));
#70295=CARTESIAN_POINT('Ctrl Pts',(1.47380002847441,-7.74501491729134,70.4706515282772));
#70296=CARTESIAN_POINT('Ctrl Pts',(5.5265864071793,-4.96373262914806,70.682805833775));
#70297=CARTESIAN_POINT('Ctrl Pts',(7.85824829472714,-0.636613292568681,
70.8949601392731));
#70298=CARTESIAN_POINT('Ctrl Pts',(6.08718936490711,5.86792278728112,71.1601530211452));
#70299=CARTESIAN_POINT('Ctrl Pts',(-1.65671505113536,8.29037858484482,71.4783844793922));
#70300=CARTESIAN_POINT('Ctrl Pts',(-7.86345831407396,3.08845654589225,71.7966159376389));
#70301=CARTESIAN_POINT('Ctrl Pts',(-6.85583031447803,-4.94698584078679,
72.1148473958858));
#70302=CARTESIAN_POINT('Ctrl Pts',(0.46678880254388,-8.4420676698729,72.4330788541326));
#70303=CARTESIAN_POINT('Ctrl Pts',(6.19106263133698,-4.88140185344963,72.698271736005));
#70304=CARTESIAN_POINT('Ctrl Pts',(7.42740839776675,-0.124087184035522,
72.9104260415028));
#70305=CARTESIAN_POINT('Ctrl Pts',(6.35066560502015,4.67187537753541,73.1225803470006));
#70306=CARTESIAN_POINT('Ctrl Pts',(0.748523360428059,8.42175950261246,73.3877732288731));
#70307=CARTESIAN_POINT('Ctrl Pts',(-6.6867529066314,5.17324284008979,73.7060046871199));
#70308=CARTESIAN_POINT('Ctrl Pts',(-7.96224246790876,-2.82407647742015,
74.0242361453667));
#70309=CARTESIAN_POINT('Ctrl Pts',(-1.93270844683755,-8.23038755417868,
74.3424676036136));
#70310=CARTESIAN_POINT('Ctrl Pts',(5.88775761908401,-6.06803068999685,74.6606990618602));
#70311=CARTESIAN_POINT('Ctrl Pts',(7.8751699986775,0.373845663894274,74.9258919437329));
#70312=CARTESIAN_POINT('Ctrl Pts',(5.68925384822416,4.77624310663567,75.1380462492305));
#70313=CARTESIAN_POINT('Ctrl Pts',(1.73182621837097,7.69173142340001,75.3502005547285));
#70314=CARTESIAN_POINT('Ctrl Pts',(-4.95715323779993,6.84894556265586,75.6153934366008));
#70315=CARTESIAN_POINT('Ctrl Pts',(-8.44026112492043,-0.477479166752036,
75.9336248948477));
#70316=CARTESIAN_POINT('Ctrl Pts',(-4.16094718559222,-7.354736283558,76.2518563530945));
#70317=CARTESIAN_POINT('Ctrl Pts',(3.93895069415804,-7.47821303053569,76.5700878113412));
#70318=CARTESIAN_POINT('Ctrl Pts',(8.42096517841398,-0.727312659247321,
76.8883192695882));
#70319=CARTESIAN_POINT('Ctrl Pts',(5.16283025738198,6.69209880639428,77.2065507278348));
#70320=CARTESIAN_POINT('Ctrl Pts',(-2.83828883793128,7.95925522611546,77.5247821860818));
#70321=CARTESIAN_POINT('Ctrl Pts',(-8.23340234365653,1.91757139606222,77.8430136443285));
#70322=CARTESIAN_POINT('Ctrl Pts',(-6.05806050855332,-5.89756953481354,
78.1612451025754));
#70323=CARTESIAN_POINT('Ctrl Pts',(0.387359295838887,-7.87476394035296,
78.4264379844476));
#70324=CARTESIAN_POINT('Ctrl Pts',(4.78607026788089,-5.68098925840602,78.6385922899456));
#70325=CARTESIAN_POINT('Ctrl Pts',(7.69444850934977,-1.71858233013379,78.8507465954435));
#70326=CARTESIAN_POINT('Ctrl Pts',(6.8409884325102,4.96865811885738,79.1159394773158));
#70327=CARTESIAN_POINT('Ctrl Pts',(-0.492908969808402,8.43988637245421,
79.4341709355625));
#70328=CARTESIAN_POINT('Ctrl Pts',(-7.36011613232335,4.14745748462858,79.7524023938093));
#70329=CARTESIAN_POINT('Ctrl Pts',(-7.47473163377407,-3.95012568406894,
80.0706338520563));
#70330=CARTESIAN_POINT('Ctrl Pts',(-0.706552258280965,-8.4253845162857,
80.3888653103029));
#70331=CARTESIAN_POINT('Ctrl Pts',(5.45558212828763,-5.69157243751812,80.6540581921753));
#70332=CARTESIAN_POINT('Ctrl Pts',(7.33869306412585,-1.15125029728964,80.8662124976733));
#70333=CARTESIAN_POINT('Ctrl Pts',(6.93634303769482,3.74759734008634,81.0783668031711));
#70334=CARTESIAN_POINT('Ctrl Pts',(1.90734909302426,8.23701510052229,81.3435596850435));
#70335=CARTESIAN_POINT('Ctrl Pts',(-5.90609562851779,6.04922413509894,81.6617911432904));
#70336=CARTESIAN_POINT('Ctrl Pts',(-8.2765549435943,-1.69445529852785,81.9800226015371));
#70337=CARTESIAN_POINT('Ctrl Pts',(-3.05364538250673,-7.88354816809072,
82.298254059784));
#70338=CARTESIAN_POINT('Ctrl Pts',(4.99093394690154,-6.8247322686972,82.6164855180308));
#70339=CARTESIAN_POINT('Ctrl Pts',(7.85103020594809,-0.720185706015227,
82.8816783999031));
#70340=CARTESIAN_POINT('Ctrl Pts',(6.29582332753661,3.94263966881761,83.0938327054011));
#70341=CARTESIAN_POINT('Ctrl Pts',(2.77993132433371,7.37762322330055,83.3059870108988));
#70342=CARTESIAN_POINT('Ctrl Pts',(-3.96077592627955,7.46984918444621,83.5711798927711));
#70343=CARTESIAN_POINT('Ctrl Pts',(-8.42569230392369,0.694831124313766,
83.8894113510182));
#70344=CARTESIAN_POINT('Ctrl Pts',(-5.13805285591533,-6.70618767823044,
84.2076428092648));
#70345=CARTESIAN_POINT('Ctrl Pts',(2.8635201522212,-7.95457940088155,84.5258742675119));
#70346=CARTESIAN_POINT('Ctrl Pts',(8.24320307796721,-1.88042435219548,84.8441057257583));
#70347=CARTESIAN_POINT('Ctrl Pts',(6.4000119132817,4.60404063430321,85.1092986076311));
#70348=CARTESIAN_POINT('Ctrl Pts',(2.16843117645446,7.1049071167996,85.3214529131286));
#70349=CARTESIAN_POINT('Ctrl Pts',(-2.73845611678586,7.39311847253433,85.5336072186269));
#70350=CARTESIAN_POINT('Ctrl Pts',(-7.88839217017907,3.04296922439314,85.7988001004986));
#70351=CARTESIAN_POINT('Ctrl Pts',(-6.81727686636293,-4.99998172274208,
86.1170315587459));
#70352=CARTESIAN_POINT('Ctrl Pts',(0.517743138293131,-8.432347382295,86.4352630169924));
#70353=CARTESIAN_POINT('Ctrl Pts',(7.3777569833882,-4.12841167938097,86.7534944752395));
#70354=CARTESIAN_POINT('Ctrl Pts',(7.45686736189402,3.98516271663605,87.071725933486));
#70355=CARTESIAN_POINT('Ctrl Pts',(1.8134261971067,7.67260243207413,87.3369188153587));
#70356=CARTESIAN_POINT('Ctrl Pts',(-3.0213437124554,6.78625677940435,87.5490731208563));
#70357=CARTESIAN_POINT('Ctrl Pts',(-6.9151876472613,3.78649210433562,87.7612274263544));
#70358=CARTESIAN_POINT('Ctrl Pts',(-7.95123661705785,-2.87475720548686,
88.0264203082266));
#70359=CARTESIAN_POINT('Ctrl Pts',(-1.86886275660877,-8.2451460325035,88.3446517664734));
#70360=CARTESIAN_POINT('Ctrl Pts',(5.91988046063556,-6.02723449558902,88.6628832247204));
#70361=CARTESIAN_POINT('Ctrl Pts',(8.27739827918244,1.72039496283128,88.981114682967));
#70362=CARTESIAN_POINT('Ctrl Pts',(3.01717744396469,7.89829304359937,89.2993461412138));
#70363=CARTESIAN_POINT('Ctrl Pts',(-3.66161413346099,6.98211462170826,89.5645390230864));
#70364=CARTESIAN_POINT('Ctrl Pts',(-6.73086714842256,3.14280548794969,89.776693328584));
#70365=CARTESIAN_POINT('Ctrl Pts',(-7.7039509303132,-1.67525601516913,89.9888476340821));
#70366=CARTESIAN_POINT('Ctrl Pts',(-4.11851979208988,-7.38404952943188,
90.2540405159544));
#70367=CARTESIAN_POINT('Ctrl Pts',(3.9951660842497,-7.45075359004759,90.5722719742013));
#70368=CARTESIAN_POINT('Ctrl Pts',(8.42168187711568,-0.669189579787365,
90.890503432448));
#70369=CARTESIAN_POINT('Ctrl Pts',(5.12168143120076,6.72632592264454,91.2087348906947));
#70370=CARTESIAN_POINT('Ctrl Pts',(-2.9007227407555,7.94180082299996,91.5269663489418));
#70371=CARTESIAN_POINT('Ctrl Pts',(-7.34271436417314,2.870868931038,91.7921592308139));
#70372=CARTESIAN_POINT('Ctrl Pts',(-7.14272675520292,-2.04040520615619,
92.004313536312));
#70373=CARTESIAN_POINT('Ctrl Pts',(-4.71830598861224,-6.31624344455306,
92.2164678418096));
#70374=CARTESIAN_POINT('Ctrl Pts',(1.73198960680328,-8.27566340137542,92.4816607236824));
#70375=CARTESIAN_POINT('Ctrl Pts',(7.90183721812814,-3.00600227520748,92.7998921819287));
#70376=CARTESIAN_POINT('Ctrl Pts',(6.79743607045418,5.01671238971521,93.118123640176));
#70377=CARTESIAN_POINT('Ctrl Pts',(-0.543308475935934,8.43681794282195,
93.4363550984225));
#70378=CARTESIAN_POINT('Ctrl Pts',(-7.3974674859525,4.09437022327196,93.7545865566693));
#70379=CARTESIAN_POINT('Ctrl Pts',(-7.42638754234585,-2.64690587742072,
94.0197794385418));
#70380=CARTESIAN_POINT('Ctrl Pts',(-4.05513953841633,-6.22395711977298,
94.2319337440395));
#70381=CARTESIAN_POINT('Ctrl Pts',(0.578985677141032,-7.86270425735951,
94.4440880495374));
#70382=CARTESIAN_POINT('Ctrl Pts',(6.73394274200306,-5.11276910082636,94.70928093141));
#70383=CARTESIAN_POINT('Ctrl Pts',(7.93714940170376,2.91148423924637,95.0275123896566));
#70384=CARTESIAN_POINT('Ctrl Pts',(1.84291222287195,8.24476893986864,95.3457438479035));
#70385=CARTESIAN_POINT('Ctrl Pts',(-5.94211444723251,6.01384710450294,95.6639753061503));
#70386=CARTESIAN_POINT('Ctrl Pts',(-8.26995989960118,-1.75902131593898,
95.982206764397));
#70387=CARTESIAN_POINT('Ctrl Pts',(-3.87163954240068,-6.86787812259019,
96.2473996462695));
#70388=CARTESIAN_POINT('Ctrl Pts',(1.01918826962898,-7.35819639421587,96.4595539517673));
#70389=CARTESIAN_POINT('Ctrl Pts',(5.5926140224005,-5.55697858997884,96.6717082572652));
#70390=CARTESIAN_POINT('Ctrl Pts',(8.43672521784369,0.555031827501162,96.9369011391376));
#70391=CARTESIAN_POINT('Ctrl Pts',(4.08380208395726,7.40254291709361,97.2551325973842));
#70392=CARTESIAN_POINT('Ctrl Pts',(-4.01451237192768,7.43345348735528,97.5733640556311));
#70393=CARTESIAN_POINT('Ctrl Pts',(-8.42969138229406,0.644503141670811,
97.8915955138779));
#70394=CARTESIAN_POINT('Ctrl Pts',(-5.09073846592904,-6.7506129056886,98.2098269721248));
#70395=CARTESIAN_POINT('Ctrl Pts',(1.57994662075434,-7.72406054666849,98.475019853997));
#70396=CARTESIAN_POINT('Ctrl Pts',(5.59418364133663,-4.88742348193836,98.6871741594951));
#70397=CARTESIAN_POINT('Ctrl Pts',(7.86624459833887,-0.528714074088318,
98.8993284649929));
#70398=CARTESIAN_POINT('Ctrl Pts',(6.00609026407533,5.95090518078709,99.1645213468653));
#70399=CARTESIAN_POINT('Ctrl Pts',(-1.77032850893993,8.26686264980742,99.4827528051121));
#70400=CARTESIAN_POINT('Ctrl Pts',(-7.90510090403196,2.98025502769608,99.8009842633589));
#70401=CARTESIAN_POINT('Ctrl Pts',(-6.78729698533865,-5.04060321123964,
100.119215721606));
#70402=CARTESIAN_POINT('Ctrl Pts',(0.582596093550364,-8.43486659780217,
100.437447179853));
#70403=CARTESIAN_POINT('Ctrl Pts',(6.25746716822917,-4.79598241151577,100.702640061725));
#70404=CARTESIAN_POINT('Ctrl Pts',(7.42841223796564,-0.0221478586563569,
100.914794367223));
#70405=CARTESIAN_POINT('Ctrl Pts',(6.28595416952829,4.75858412047349,101.126948672721));
#70406=CARTESIAN_POINT('Ctrl Pts',(0.632882506249434,8.43124264057339,101.392141554594));
#70407=CARTESIAN_POINT('Ctrl Pts',(-6.75711940236345,5.08098597543341,101.71037301284));
#70408=CARTESIAN_POINT('Ctrl Pts',(-7.92273150330738,-2.93306424401754,
102.028604471087));
#70409=CARTESIAN_POINT('Ctrl Pts',(-1.81959200462792,-8.25615927880757,
102.346835929334));
#70410=CARTESIAN_POINT('Ctrl Pts',(5.9704984758136,-5.98661345680911,102.665067387581));
#70411=CARTESIAN_POINT('Ctrl Pts',(7.86925744826999,0.481798573971578,102.930260269453));
#70412=CARTESIAN_POINT('Ctrl Pts',(5.62322769431742,4.8539786982085,103.142414574951));
#70413=CARTESIAN_POINT('Ctrl Pts',(1.62597679404605,7.71450206547757,103.354568880449));
#70414=CARTESIAN_POINT('Ctrl Pts',(-5.05039432632765,6.78084875804923,103.619761762321));
#70415=CARTESIAN_POINT('Ctrl Pts',(-8.43338466048396,-0.594225772463747,
103.937993220568));
#70416=CARTESIAN_POINT('Ctrl Pts',(-4.05876638382929,-7.40938295504631,
104.256224678815));
#70417=CARTESIAN_POINT('Ctrl Pts',(4.03958841382724,-7.42676285788232,104.574456137062));
#70418=CARTESIAN_POINT('Ctrl Pts',(8.43326559218159,-0.605329813131043,
104.892687595308));
#70419=CARTESIAN_POINT('Ctrl Pts',(5.62565063348024,5.52353126206922,105.157880477181));
#70420=CARTESIAN_POINT('Ctrl Pts',(1.06304677918724,7.35198819708387,105.370034782679));
#70421=CARTESIAN_POINT('Ctrl Pts',(-3.83061782890051,6.89084245226548,105.582189088177));
#70422=CARTESIAN_POINT('Ctrl Pts',(-8.25932389787385,1.80830348142917,105.847381970049));
#70423=CARTESIAN_POINT('Ctrl Pts',(-5.97786913326917,-5.97830759712599,
106.165613428296));
#70424=CARTESIAN_POINT('Ctrl Pts',(1.79371623271613,-8.25561157089681,106.483844886542));
#70425=CARTESIAN_POINT('Ctrl Pts',(7.91964722679908,-2.95876137993589,106.802076344789));
#70426=CARTESIAN_POINT('Ctrl Pts',(6.76431025852604,5.07252397306689,107.120307803036));
#70427=CARTESIAN_POINT('Ctrl Pts',(0.625860372993087,7.85911200114565,107.385500684908));
#70428=CARTESIAN_POINT('Ctrl Pts',(-4.01795423759709,6.24802710056353,107.597654990406));
#70429=CARTESIAN_POINT('Ctrl Pts',(-7.41047211820897,2.6911420695088,107.809809295904));
#70430=CARTESIAN_POINT('Ctrl Pts',(-7.42175053436507,-4.05018662984695,
108.075002177777));
#70431=CARTESIAN_POINT('Ctrl Pts',(-0.593607222905992,-8.4334282213855,
108.393233636023));
#70432=CARTESIAN_POINT('Ctrl Pts',(6.7674007672284,-5.05715603761144,108.71146509427));
#70433=CARTESIAN_POINT('Ctrl Pts',(7.91962140522928,2.95883049500652,109.029696552517));
#70434=CARTESIAN_POINT('Ctrl Pts',(1.78130626263137,8.26518848724278,109.347928010764));
#70435=CARTESIAN_POINT('Ctrl Pts',(-4.68055859797518,6.34426621950518,109.613120892636));
#70436=CARTESIAN_POINT('Ctrl Pts',(-7.13043291328011,2.08296072310835,109.825275198134));
#70437=CARTESIAN_POINT('Ctrl Pts',(-7.35970269699859,-2.82703358042056,
110.037429503632));
#70438=CARTESIAN_POINT('Ctrl Pts',(-2.94802780900771,-7.92436273578246,
110.302622385504));
#70439=CARTESIAN_POINT('Ctrl Pts',(5.0814815637804,-6.75674671845169,110.620853843751));
#70440=CARTESIAN_POINT('Ctrl Pts',(8.42552250194139,0.618959532047456,110.939085301998));
#70441=CARTESIAN_POINT('Ctrl Pts',(4.03952359991809,7.42679811130282,111.257316760245));
#70442=CARTESIAN_POINT('Ctrl Pts',(-4.07441578005489,7.40847681930506,111.575548218491));
#70443=CARTESIAN_POINT('Ctrl Pts',(-7.69382448055576,1.72116458115858,111.840741100364));
#70444=CARTESIAN_POINT('Ctrl Pts',(-6.74948790579361,-3.10261372303192,
112.052895405862));
#70445=CARTESIAN_POINT('Ctrl Pts',(-3.70318310388795,-6.96015643158348,
112.26504971136));
#70446=CARTESIAN_POINT('Ctrl Pts',(2.97002659885532,-7.91614393079309,112.530242593232));
#70447=CARTESIAN_POINT('Ctrl Pts',(8.26699247260189,-1.76972216980235,112.848474051479));
#70448=CARTESIAN_POINT('Ctrl Pts',(5.95571537043626,5.99182733057143,113.166705509726));
#70449=CARTESIAN_POINT('Ctrl Pts',(-1.81966405650071,8.25614339881686,113.484936967973));
#70450=CARTESIAN_POINT('Ctrl Pts',(-7.93395319352799,2.92211900063055,113.803168426219));
#70451=CARTESIAN_POINT('Ctrl Pts',(-6.93764340508899,-3.74518979984444,
114.068361308092));
#70452=CARTESIAN_POINT('Ctrl Pts',(-3.06175617355554,-6.76811997813982,
114.280515613589));
#70453=CARTESIAN_POINT('Ctrl Pts',(1.76764253705638,-7.68327941143772,114.492669919087));
#70454=CARTESIAN_POINT('Ctrl Pts',(7.43297142413431,-4.02955686632436,114.75786280096));
#70455=CARTESIAN_POINT('Ctrl Pts',(7.40224337005944,4.08434501367814,115.076094259207));
#70456=CARTESIAN_POINT('Ctrl Pts',(0.568015682008036,8.42911018542453,115.394325717453));
#70457=CARTESIAN_POINT('Ctrl Pts',(-6.78734097469309,5.04054397794511,115.7125571757));
#70458=CARTESIAN_POINT('Ctrl Pts',(-7.90639702874043,-2.99587695923303,
116.030788633947));
#70459=CARTESIAN_POINT('Ctrl Pts',(-2.78249229912331,-7.37665772951092,
116.295981515819));
#70460=CARTESIAN_POINT('Ctrl Pts',(2.12602634926904,-7.11771106936877,116.508135821317));
#70461=CARTESIAN_POINT('Ctrl Pts',(6.37244442075708,-4.64212179476106,116.720290126815));
#70462=CARTESIAN_POINT('Ctrl Pts',(8.25426942022403,1.83123703252574,116.985483008687));
#70463=CARTESIAN_POINT('Ctrl Pts',(2.91090207991093,7.93736292363641,117.303714466934));
#70464=CARTESIAN_POINT('Ctrl Pts',(-5.09797278075856,6.73670645491388,117.621945925181));
#70465=CARTESIAN_POINT('Ctrl Pts',(-8.42968575735979,-0.6445767080121,117.940177383428));
#70466=CARTESIAN_POINT('Ctrl Pts',(-4.00524791880345,-7.44609843071264,
118.258408841675));
#70467=CARTESIAN_POINT('Ctrl Pts',(2.73588942891193,-7.39406868278906,118.523601723547));
#70468=CARTESIAN_POINT('Ctrl Pts',(6.27220159664381,-3.98011130948106,118.735756029045));
#70469=CARTESIAN_POINT('Ctrl Pts',(7.85518505938354,0.673357509701594,118.947910334543));
#70470=CARTESIAN_POINT('Ctrl Pts',(5.03154082906854,6.79485022766188,119.213103216415));
#70471=CARTESIAN_POINT('Ctrl Pts',(-3.00658182864851,7.90161672115188,119.531334674662));
#70472=CARTESIAN_POINT('Ctrl Pts',(-8.26630379901193,1.74377803503611,119.849566132909));
#70473=CARTESIAN_POINT('Ctrl Pts',(-5.94206196384213,-6.01389896142331,
120.167797591156));
#70474=CARTESIAN_POINT('Ctrl Pts',(1.85819830642578,-8.24824173899719,120.486029049402));
#70475=CARTESIAN_POINT('Ctrl Pts',(6.91387274892134,-3.78889248524638,120.751221931275));
#70476=CARTESIAN_POINT('Ctrl Pts',(7.34542771599016,1.10747034902265,120.963376236773));
#70477=CARTESIAN_POINT('Ctrl Pts',(5.48942310975583,5.65893776031443,121.17553054227));
#70478=CARTESIAN_POINT('Ctrl Pts',(-0.656298100951151,8.4294522677116,121.440723424143));
#70479=CARTESIAN_POINT('Ctrl Pts',(-7.45104659610839,3.99461959677861,121.758954882389));
#70480=CARTESIAN_POINT('Ctrl Pts',(-7.38471220878525,-4.10348217084607,
122.077186340637));
#70481=CARTESIAN_POINT('Ctrl Pts',(-0.543234847355393,-8.43682268398279,
122.395417798883));
#70482=CARTESIAN_POINT('Ctrl Pts',(6.81125465061382,-5.00931161093324,122.71364925713));
#70483=CARTESIAN_POINT('Ctrl Pts',(7.70453203163159,1.67258148578646,122.978842139003));
#70484=CARTESIAN_POINT('Ctrl Pts',(4.81989742627491,5.65246739972814,123.1909964445));
#70485=CARTESIAN_POINT('Ctrl Pts',(0.434219869285401,7.87202615329449,123.403150749998));
#70486=CARTESIAN_POINT('Ctrl Pts',(-6.02259591881576,5.93420012550998,123.66834363187));
#70487=CARTESIAN_POINT('Ctrl Pts',(-8.24500893828536,-1.86946749314901,
123.986575090117));
#70488=CARTESIAN_POINT('Ctrl Pts',(-2.88511749906848,-7.94031720711482,
124.304806548364));
#70489=CARTESIAN_POINT('Ctrl Pts',(5.12174013201059,-6.72628122520153,124.623038006611));
#70490=CARTESIAN_POINT('Ctrl Pts',(8.42726279619414,0.683838061839922,124.941269464858));
#70491=CARTESIAN_POINT('Ctrl Pts',(4.72049838974924,6.31460510288725,125.20646234673));
#70492=CARTESIAN_POINT('Ctrl Pts',(-0.0670524327962581,7.42814262625973,
125.418616652228));
#70493=CARTESIAN_POINT('Ctrl Pts',(-4.83372136248423,6.2283609756417,125.630770957726));
#70494=CARTESIAN_POINT('Ctrl Pts',(-8.43823429245977,0.531596422575805,
125.895963839598));
#70495=CARTESIAN_POINT('Ctrl Pts',(-4.99948169501149,-6.81764357249575,
126.214195297845));
#70496=CARTESIAN_POINT('Ctrl Pts',(3.02798715072524,-7.88694073440878,126.532426756092));
#70497=CARTESIAN_POINT('Ctrl Pts',(8.27741329284568,-1.72032272546982,126.850658214339));
#70498=CARTESIAN_POINT('Ctrl Pts',(5.91448945058515,6.04195392814753,127.168889672586));
#70499=CARTESIAN_POINT('Ctrl Pts',(-0.57625610256022,7.86290477859779,127.434082554458));
#70500=CARTESIAN_POINT('Ctrl Pts',(-4.92115119297959,5.56453680378123,127.646236859956));
#70501=CARTESIAN_POINT('Ctrl Pts',(-7.73347024311397,1.53322557110968,127.858391165454));
#70502=CARTESIAN_POINT('Ctrl Pts',(-6.71971589330665,-5.13145311234377,
128.123584047326));
#70503=CARTESIAN_POINT('Ctrl Pts',(0.695449107532702,-8.42564131916249,
128.441815505573));
#70504=CARTESIAN_POINT('Ctrl Pts',(7.45758551789534,-3.96950356799327,128.76004696382));
#70505=CARTESIAN_POINT('Ctrl Pts',(7.37772095423774,4.12847606529929,129.078278422067));
#70506=CARTESIAN_POINT('Ctrl Pts',(0.504021424748521,8.43992625171176,129.396509880313));
#70507=CARTESIAN_POINT('Ctrl Pts',(-5.59068457894054,5.55891973245065,129.661702762186));
#70508=CARTESIAN_POINT('Ctrl Pts',(-7.36422297414272,0.974689125777787,
129.873857067684));
#70509=CARTESIAN_POINT('Ctrl Pts',(-6.84434845783166,-3.91308533523255,
130.086011373181));
#70510=CARTESIAN_POINT('Ctrl Pts',(-1.70899701609721,-8.28044213372148,
130.351204255054));
#70511=CARTESIAN_POINT('Ctrl Pts',(6.04965748659407,-5.90565198731203,130.669435713301));
#70512=CARTESIAN_POINT('Ctrl Pts',(8.23347783603216,1.89271843035402,130.987667171547));
#70513=CARTESIAN_POINT('Ctrl Pts',(2.86345073195746,7.95460439028861,131.305898629794));
#70514=CARTESIAN_POINT('Ctrl Pts',(-5.15338257306271,6.70291285834692,131.624130088041));
#70515=CARTESIAN_POINT('Ctrl Pts',(-7.86606058112608,0.531444810953261,
131.889322969913));
#70516=CARTESIAN_POINT('Ctrl Pts',(-6.19932995725014,-4.09268945632841,
132.101477275411));
#70517=CARTESIAN_POINT('Ctrl Pts',(-2.60196477537556,-7.44225247897018,
132.313631580909));
#70518=CARTESIAN_POINT('Ctrl Pts',(4.13901333038334,-7.37258173110669,132.578824462781));
#70519=CARTESIAN_POINT('Ctrl Pts',(8.4399481069777,-0.492297726859653,132.897055921028));
#70520=CARTESIAN_POINT('Ctrl Pts',(4.97553001892583,6.82763805161073,133.215287379275));
#70521=CARTESIAN_POINT('Ctrl Pts',(-3.05371419871836,7.88352146523951,133.533518837522));
#70522=CARTESIAN_POINT('Ctrl Pts',(-8.28598212377782,1.68193132302526,133.851750295769));
#70523=CARTESIAN_POINT('Ctrl Pts',(-6.28760573439148,-4.75640166321992,
134.116943177641));
#70524=CARTESIAN_POINT('Ctrl Pts',(-1.99718992382571,-7.15493055961901,
134.329097483139));
#70525=CARTESIAN_POINT('Ctrl Pts',(2.91520340889385,-7.32522571241372,134.541251788637));
#70526=CARTESIAN_POINT('Ctrl Pts',(7.95919067301005,-2.85266131211001,134.806444670509));
#70527=CARTESIAN_POINT('Ctrl Pts',(6.69524230284883,5.16224869669132,135.124676128756));
#70528=CARTESIAN_POINT('Ctrl Pts',(-0.720086676891106,8.41748273005637,
135.442907587003));
#70529=CARTESIAN_POINT('Ctrl Pts',(-7.47476835559155,3.95005305414921,135.76113904525));
#70530=CARTESIAN_POINT('Ctrl Pts',(-7.35901803486954,-4.16308134599907,
136.079370503496));
#70531=CARTESIAN_POINT('Ctrl Pts',(-1.6286547873363,-7.71393714238848,136.344563385369));
#70532=CARTESIAN_POINT('Ctrl Pts',(3.18343636205135,-6.71174581115595,136.556717690867));
#70533=CARTESIAN_POINT('Ctrl Pts',(7.00412161819763,-3.61934013468348,136.768871996364));
#70534=CARTESIAN_POINT('Ctrl Pts',(7.87990980123138,3.0648677386468,137.034064878237));
#70535=CARTESIAN_POINT('Ctrl Pts',(1.67032640351384,8.28764687990933,137.352296336484));
#70536=CARTESIAN_POINT('Ctrl Pts',(-6.06291022794655,5.8833374797724,137.670527794731));
#70537=CARTESIAN_POINT('Ctrl Pts',(-8.23369805000805,-1.9186707694759,137.988759252977));
#70538=CARTESIAN_POINT('Ctrl Pts',(-2.82663921160395,-7.96846933220942,
138.306990711224));
#70539=CARTESIAN_POINT('Ctrl Pts',(3.82822544044891,-6.89217183695629,138.572183593096));
#70540=CARTESIAN_POINT('Ctrl Pts',(6.80439690023717,-2.98026537892912,138.784337898594));
#70541=CARTESIAN_POINT('Ctrl Pts',(7.66150002642696,1.85977417932761,138.996492204092));
#70542=CARTESIAN_POINT('Ctrl Pts',(3.94001291137149,7.48082154506875,139.261685085965));
#70543=CARTESIAN_POINT('Ctrl Pts',(-4.17293501391588,7.3526658070377,139.579916544211));
#70544=CARTESIAN_POINT('Ctrl Pts',(-8.43532308489233,0.466759881006833,
139.898148002458));
#70545=CARTESIAN_POINT('Ctrl Pts',(-4.95867971941822,-6.84737734761105,
140.216379460705));
#70546=CARTESIAN_POINT('Ctrl Pts',(3.0905991967229,-7.86985319660759,140.534610918952));
#70547=CARTESIAN_POINT('Ctrl Pts',(7.40953744105551,-2.69371445454605,140.799803800824));
#70548=CARTESIAN_POINT('Ctrl Pts',(7.09166906773478,2.21134093674737,141.011958106322));
#70549=CARTESIAN_POINT('Ctrl Pts',(4.56526824486317,6.42772654252474,141.22411241182));
#70550=CARTESIAN_POINT('Ctrl Pts',(-1.93022040882533,8.23168524084186,141.489305293693));
#70551=CARTESIAN_POINT('Ctrl Pts',(-7.97174412624228,2.81538215631022,141.807536751939));
#70552=CARTESIAN_POINT('Ctrl Pts',(-6.67500546132707,-5.17849808576631,
142.125768210186));
#70553=CARTESIAN_POINT('Ctrl Pts',(0.745751997391611,-8.42133808006394,
142.443999668433));
#70554=CARTESIAN_POINT('Ctrl Pts',(7.49365570889798,-3.91554809029897,142.76223112668));
#70555=CARTESIAN_POINT('Ctrl Pts',(7.3606836589212,2.82447848749324,143.027424008552));
#70556=CARTESIAN_POINT('Ctrl Pts',(3.90450918100473,6.31954167327552,143.23957831405));
#70557=CARTESIAN_POINT('Ctrl Pts',(-0.76763224961116,7.84653320788012,143.451732619548));
#70558=CARTESIAN_POINT('Ctrl Pts',(-6.85477795141283,4.94958705022387,143.71692550142));
#70559=CARTESIAN_POINT('Ctrl Pts',(-7.86494469201523,-3.10124589351471,
144.035156959667));
#70560=CARTESIAN_POINT('Ctrl Pts',(-1.64439240863728,-8.2866467246535,144.353388417914));
#70561=CARTESIAN_POINT('Ctrl Pts',(6.08481632047936,-5.86942002640229,144.67161987616));
#70562=CARTESIAN_POINT('Ctrl Pts',(8.22533424935467,1.95710735993869,144.989851334407));
#70563=CARTESIAN_POINT('Ctrl Pts',(3.70559910065562,6.95887045119629,145.25504421628));
#70564=CARTESIAN_POINT('Ctrl Pts',(-1.1955927401216,7.3315998871873,145.467198521778));
#70565=CARTESIAN_POINT('Ctrl Pts',(-5.72444552590752,5.42107609930576,145.679352827275));
#70566=CARTESIAN_POINT('Ctrl Pts',(-8.42096385881222,-0.757469741041528,
145.944545709148));
#70567=CARTESIAN_POINT('Ctrl Pts',(-3.90486111908968,-7.49847589595874,
146.262777167394));
#70568=CARTESIAN_POINT('Ctrl Pts',(4.19186028299498,-7.33490611339408,146.581008625642));
#70569=CARTESIAN_POINT('Ctrl Pts',(8.44273746126223,-0.441888226112777,
146.899240083888));
#70570=CARTESIAN_POINT('Ctrl Pts',(4.92716246104114,6.87091427440382,147.217471542135));
#70571=CARTESIAN_POINT('Ctrl Pts',(-1.76497519032476,7.68389257525593,147.482664424007));
#70572=CARTESIAN_POINT('Ctrl Pts',(-5.70993610234189,4.7516763951212,147.694818729505));
#70573=CARTESIAN_POINT('Ctrl Pts',(-7.87667266568883,0.339663018585871,
147.906973035003));
#70574=CARTESIAN_POINT('Ctrl Pts',(-5.86145424027185,-6.09341817350986,
148.172165916875));
#70575=CARTESIAN_POINT('Ctrl Pts',(1.96833677532543,-8.22196648831977,148.490397375122));
#70576=CARTESIAN_POINT('Ctrl Pts',(7.97438883746259,-2.78956373241462,148.808628833369));
#70577=CARTESIAN_POINT('Ctrl Pts',(6.664295105365,5.20213810875714,149.126860291616));
#70578=CARTESIAN_POINT('Ctrl Pts',(-0.784980464148565,8.41844470718301,
149.445091749863));
#70579=CARTESIAN_POINT('Ctrl Pts',(-6.37083420409281,4.64433221669856,149.710284631735));
#70580=CARTESIAN_POINT('Ctrl Pts',(-7.42679969286816,-0.156241061364189,
149.922438937233));
#70581=CARTESIAN_POINT('Ctrl Pts',(-6.16987516676678,-4.90816647717152,
150.134593242731));
#70582=CARTESIAN_POINT('Ctrl Pts',(-0.430222084104789,-8.44399890804918,
150.399786124603));
#70583=CARTESIAN_POINT('Ctrl Pts',(6.87716522396635,-4.917273833794,150.71801758285));
#70584=CARTESIAN_POINT('Ctrl Pts',(7.85004833380309,3.12250508572264,151.036249041097));
#70585=CARTESIAN_POINT('Ctrl Pts',(1.62073799871939,8.29741387924024,151.354480499344));
#70586=CARTESIAN_POINT('Ctrl Pts',(-6.11240446161866,5.8416314624366,151.67271195759));
#70587=CARTESIAN_POINT('Ctrl Pts',(-7.85565197732039,-0.670838177559451,
151.937904839463));
#70588=CARTESIAN_POINT('Ctrl Pts',(-5.50473164554611,-4.98733689650615,
152.150059144961));
#70589=CARTESIAN_POINT('Ctrl Pts',(-1.44101267407513,-7.75199824614526,
152.362213450459));
#70590=CARTESIAN_POINT('Ctrl Pts',(5.21338494434369,-6.65618030389132,152.627406332331));
#70591=CARTESIAN_POINT('Ctrl Pts',(8.41397490779385,0.79416338508947,152.945637790578));
#70592=CARTESIAN_POINT('Ctrl Pts',(3.88463257389226,7.50913956436645,153.263869248825));
#70593=CARTESIAN_POINT('Ctrl Pts',(-4.22626533191902,7.31905378776502,153.582100707071));
#70594=CARTESIAN_POINT('Ctrl Pts',(-7.72583738521557,1.57078236861736,153.847293588944));
#70595=CARTESIAN_POINT('Ctrl Pts',(-6.68713870766457,-3.25309306180461,
154.059461682204));
#70596=CARTESIAN_POINT('Ctrl Pts',(-5.11767179385483,-5.12707892333455,
154.165552622715));
#70597=CARTESIAN_POINT('Ctrl Pts',(-4.14791805377987,-5.81840619716922,
154.218604986852));
#70598=CARTESIAN_POINT('Ctrl Pts',(-3.25626140427607,6.79079303725207,-0.219318740910142));
#70599=CARTESIAN_POINT('Ctrl Pts',(-4.38783911844251,6.24818997146264,-0.166277514063165));
#70600=CARTESIAN_POINT('Ctrl Pts',(-6.35583945430648,4.58604843748734,-0.0601977108417193));
#70601=CARTESIAN_POINT('Ctrl Pts',(-8.30600288127432,-0.23487779396911,
0.151959245128665));
#70602=CARTESIAN_POINT('Ctrl Pts',(-5.71099197201566,-6.83602431645478,
0.417152127001014));
#70603=CARTESIAN_POINT('Ctrl Pts',(2.67663026760001,-8.49913365837745,0.73538358524783));
#70604=CARTESIAN_POINT('Ctrl Pts',(8.59315924532233,-2.34512449975285,1.05361504349465));
#70605=CARTESIAN_POINT('Ctrl Pts',(6.61618139014667,5.96934387336162,1.37184650174147));
#70606=CARTESIAN_POINT('Ctrl Pts',(-0.0954035072434517,8.3097161946593,
1.63703938361381));
#70607=CARTESIAN_POINT('Ctrl Pts',(-4.81458352345695,6.17338366571372,1.84919368911169));
#70608=CARTESIAN_POINT('Ctrl Pts',(-8.03570940339818,2.11617400989208,2.06134799460957));
#70609=CARTESIAN_POINT('Ctrl Pts',(-7.40248233935818,-4.96109161769496,
2.32654087648192));
#70610=CARTESIAN_POINT('Ctrl Pts',(0.18345886150707,-8.90852845273233,2.64477233472873));
#70611=CARTESIAN_POINT('Ctrl Pts',(7.58684621947925,-4.66085638140519,2.96300379297555));
#70612=CARTESIAN_POINT('Ctrl Pts',(8.02953162399686,3.86308122171422,3.28123525122236));
#70613=CARTESIAN_POINT('Ctrl Pts',(1.07920619621232,8.84559539285239,3.59946670946919));
#70614=CARTESIAN_POINT('Ctrl Pts',(-5.51954412358968,6.21137598843296,3.86465959134152));
#70615=CARTESIAN_POINT('Ctrl Pts',(-7.68340312835726,1.50434211377469,4.07681389683941));
#70616=CARTESIAN_POINT('Ctrl Pts',(-7.45445771613391,-3.67117143356693,
4.28896820233728));
#70617=CARTESIAN_POINT('Ctrl Pts',(-2.33639713332563,-8.59945993394335,
4.55416108420963));
#70618=CARTESIAN_POINT('Ctrl Pts',(5.9798023331272,-6.60596964644571,4.87239254245645));
#70619=CARTESIAN_POINT('Ctrl Pts',(8.78433487726616,1.4554866160667,5.19062400070327));
#70620=CARTESIAN_POINT('Ctrl Pts',(3.52963249230927,8.18160003932308,5.50885545895009));
#70621=CARTESIAN_POINT('Ctrl Pts',(-4.98510569539155,7.38635008106619,5.8270869171969));
#70622=CARTESIAN_POINT('Ctrl Pts',(-8.24014557041358,1.07071602129575,6.09227979906925));
#70623=CARTESIAN_POINT('Ctrl Pts',(-6.78761070841664,-3.90206450061349,
6.30443410456712));
#70624=CARTESIAN_POINT('Ctrl Pts',(-3.22123524393854,-7.65963932084413,
6.51658841006501));
#70625=CARTESIAN_POINT('Ctrl Pts',(3.87447872379791,-8.02482792303879,6.78178129193735));
#70626=CARTESIAN_POINT('Ctrl Pts',(8.84639377321643,-1.06686466781347,7.10001275018417));
#70627=CARTESIAN_POINT('Ctrl Pts',(5.6781320946836,6.85870201306817,7.41824420843098));
#70628=CARTESIAN_POINT('Ctrl Pts',(-2.69956168110274,8.49171654179624,7.73647566667781));
#70629=CARTESIAN_POINT('Ctrl Pts',(-8.60704720841996,2.30828653891773,8.05470712492461));
#70630=CARTESIAN_POINT('Ctrl Pts',(-6.92364489287862,-4.59451548655276,
8.31990000679697));
#70631=CARTESIAN_POINT('Ctrl Pts',(-2.56635205336581,-7.39672925615521,
8.53205431229485));
#70632=CARTESIAN_POINT('Ctrl Pts',(2.59017037923298,-7.89540680161064,8.74420861779272));
#70633=CARTESIAN_POINT('Ctrl Pts',(8.18712624868128,-3.51858099169413,9.00940149966508));
#70634=CARTESIAN_POINT('Ctrl Pts',(7.37885783341021,4.9949314456656,9.32763295791187));
#70635=CARTESIAN_POINT('Ctrl Pts',(-0.209966232129463,8.90162297445633,
9.64586441615873));
#70636=CARTESIAN_POINT('Ctrl Pts',(-7.60615567604954,4.6414737858246,9.9640958744055));
#70637=CARTESIAN_POINT('Ctrl Pts',(-8.01212511125873,-3.90067937766853,
10.2823273326523));
#70638=CARTESIAN_POINT('Ctrl Pts',(-2.21503253104398,-8.00874909362732,
10.5475202145246));
#70639=CARTESIAN_POINT('Ctrl Pts',(2.91224332325345,-7.26750337980572,10.7596745200225));
#70640=CARTESIAN_POINT('Ctrl Pts',(7.13256993626704,-4.26296578247275,10.9718288255204));
#70641=CARTESIAN_POINT('Ctrl Pts',(8.48864274698747,2.71152959044796,11.2370217073928));
#70642=CARTESIAN_POINT('Ctrl Pts',(2.29618701398579,8.60955331416399,11.5552531656396));
#70643=CARTESIAN_POINT('Ctrl Pts',(-5.99519548657091,6.58335844961113,11.8734846238864));
#70644=CARTESIAN_POINT('Ctrl Pts',(-8.78625442260016,-1.48277317684341,
12.1917160821332));
#70645=CARTESIAN_POINT('Ctrl Pts',(-3.49181055050968,-8.19857960168739,
12.5099475403801));
#70646=CARTESIAN_POINT('Ctrl Pts',(3.57879403802026,-7.49924425470446,12.7751404222524));
#70647=CARTESIAN_POINT('Ctrl Pts',(6.96403896420184,-3.57769868132897,12.9872947277503));
#70648=CARTESIAN_POINT('Ctrl Pts',(8.18049881518126,1.45803645122659,13.1994490332481));
#70649=CARTESIAN_POINT('Ctrl Pts',(4.63130578286872,7.61317641667533,13.4646419151205));
#70650=CARTESIAN_POINT('Ctrl Pts',(-3.91145815038478,8.00608382484316,13.7828733733673));
#70651=CARTESIAN_POINT('Ctrl Pts',(-8.84318963161335,1.03969925343594,14.1011048316142));
#70652=CARTESIAN_POINT('Ctrl Pts',(-5.66169037244258,-6.88056285482645,
14.4193362898609));
#70653=CARTESIAN_POINT('Ctrl Pts',(2.73925198622831,-8.47973743472043,14.7375677481078));
#70654=CARTESIAN_POINT('Ctrl Pts',(7.61925668070438,-3.31562343938954,15.0027606299801));
#70655=CARTESIAN_POINT('Ctrl Pts',(7.60393255881819,1.86493329377995,15.214914935478));
#70656=CARTESIAN_POINT('Ctrl Pts',(5.22054364993401,6.4647007013025,15.4270692409758));
#70657=CARTESIAN_POINT('Ctrl Pts',(-1.49505376412002,8.78488831165459,15.6922621228482));
#70658=CARTESIAN_POINT('Ctrl Pts',(-8.202756761262,3.48018168896353,16.010493581095));
#70659=CARTESIAN_POINT('Ctrl Pts',(-7.35862662766388,-5.01334135611222,
16.3287250393419));
#70660=CARTESIAN_POINT('Ctrl Pts',(0.236714126732794,-8.90734806184376,
16.6469564975886));
#70661=CARTESIAN_POINT('Ctrl Pts',(7.62826869219535,-4.60640479827018,16.9651879558355));
#70662=CARTESIAN_POINT('Ctrl Pts',(7.92680547927285,2.49242573651805,17.2303808377078));
#70663=CARTESIAN_POINT('Ctrl Pts',(4.51842007932001,6.39387570539983,17.4425351432057));
#70664=CARTESIAN_POINT('Ctrl Pts',(-0.297120289451444,8.30410444851726,
17.6546894487036));
#70665=CARTESIAN_POINT('Ctrl Pts',(-6.88893937990305,5.6526067107022,17.9198823305759));
#70666=CARTESIAN_POINT('Ctrl Pts',(-8.47526645909824,-2.75077107733645,
18.2381137888227));
#70667=CARTESIAN_POINT('Ctrl Pts',(-2.26884065207606,-8.61018812185635,
18.5563452470696));
#70668=CARTESIAN_POINT('Ctrl Pts',(6.01914491904821,-6.57014288399595,18.8745767053164));
#70669=CARTESIAN_POINT('Ctrl Pts',(8.77995628575123,1.52375064434829,19.1928081635632));
#70670=CARTESIAN_POINT('Ctrl Pts',(4.35076258993752,7.07935703607947,19.4580010454356));
#70671=CARTESIAN_POINT('Ctrl Pts',(-0.780808721133584,7.79025701054246,
19.6701553509334));
#70672=CARTESIAN_POINT('Ctrl Pts',(-5.66921564014895,6.07506585839019,19.8823096564313));
#70673=CARTESIAN_POINT('Ctrl Pts',(-8.90771660123625,-0.249064967258383,
20.1475025383036));
#70674=CARTESIAN_POINT('Ctrl Pts',(-4.59547615923811,-7.63403444729592,
20.4657339965505));
#70675=CARTESIAN_POINT('Ctrl Pts',(3.93252182436328,-7.98863251746972,20.7839654547973));
#70676=CARTESIAN_POINT('Ctrl Pts',(8.85260702063095,-1.01401775669988,21.1021969130441));
#70677=CARTESIAN_POINT('Ctrl Pts',(5.63006673821769,6.90737265022453,21.420428371291));
#70678=CARTESIAN_POINT('Ctrl Pts',(-1.35685593532154,8.1978883335326,21.6856212531632));
#70679=CARTESIAN_POINT('Ctrl Pts',(-5.69749473468943,5.36994602370365,21.8977755586612));
#70680=CARTESIAN_POINT('Ctrl Pts',(-8.26378367614365,0.869661147913093,
22.109929864159));
#70681=CARTESIAN_POINT('Ctrl Pts',(-6.56232287864745,-6.02871187255083,
22.3751227460314));
#70682=CARTESIAN_POINT('Ctrl Pts',(1.53578266229113,-8.77714387980692,22.6933542042781));
#70683=CARTESIAN_POINT('Ctrl Pts',(8.20721798994993,-3.45319421169897,23.011585662525));
#70684=CARTESIAN_POINT('Ctrl Pts',(7.34889809770717,5.03890660978577,23.3298171207718));
#70685=CARTESIAN_POINT('Ctrl Pts',(-0.27816984382537,8.90685522189735,23.6480485790186));
#70686=CARTESIAN_POINT('Ctrl Pts',(-6.39970799874712,5.30001591403834,23.913241460891));
#70687=CARTESIAN_POINT('Ctrl Pts',(-7.82279861437396,0.318729333844981,
24.1253957663889));
#70688=CARTESIAN_POINT('Ctrl Pts',(-6.80966379123187,-4.76181795207178,
24.3375500718868));
#70689=CARTESIAN_POINT('Ctrl Pts',(-1.00184047355013,-8.85470293524363,
24.6027429537591));
#70690=CARTESIAN_POINT('Ctrl Pts',(6.91461318249575,-5.62005405748759,24.9209744120059));
#70691=CARTESIAN_POINT('Ctrl Pts',(8.4609395460387,2.77407270931146,25.2392058702527));
#70692=CARTESIAN_POINT('Ctrl Pts',(2.2447325164063,8.62311190942198,25.5574373284995));
#70693=CARTESIAN_POINT('Ctrl Pts',(-6.05012225740613,6.54258886651866,25.8756687867463));
#70694=CARTESIAN_POINT('Ctrl Pts',(-8.30714153147531,-0.194501245047355,
26.1408616686187));
#70695=CARTESIAN_POINT('Ctrl Pts',(-6.11546704534361,-4.88864289620552,
26.3530159741166));
#70696=CARTESIAN_POINT('Ctrl Pts',(-2.01927511983364,-8.0603324465377,26.5651702796144));
#70697=CARTESIAN_POINT('Ctrl Pts',(5.04947513615378,-7.34249611884268,26.8303631614868));
#70698=CARTESIAN_POINT('Ctrl Pts',(8.90575690367034,0.29047727166572,27.1485946197336));
#70699=CARTESIAN_POINT('Ctrl Pts',(4.56938031041736,7.64223403050698,27.4668260779804));
#70700=CARTESIAN_POINT('Ctrl Pts',(-3.95919823070793,7.9825830683173,27.7850575362273));
#70701=CARTESIAN_POINT('Ctrl Pts',(-8.85792920644842,0.972902142767944,
28.103288994474));
#70702=CARTESIAN_POINT('Ctrl Pts',(-6.14464476425655,-5.59372611765914,
28.3684818763464));
#70703=CARTESIAN_POINT('Ctrl Pts',(-1.41197554189225,-7.70091498579245,
28.5806361818443));
#70704=CARTESIAN_POINT('Ctrl Pts',(3.76042003719523,-7.40983618591857,28.7927904873422));
#70705=CARTESIAN_POINT('Ctrl Pts',(8.62689382504626,-2.23296917516404,29.0579833692145));
#70706=CARTESIAN_POINT('Ctrl Pts',(6.53368979848841,6.0586946357904,29.3762148274614));
#70707=CARTESIAN_POINT('Ctrl Pts',(-1.56086226855208,8.76622418016329,29.6944462857081));
#70708=CARTESIAN_POINT('Ctrl Pts',(-8.22339305523067,3.43113534151757,30.012677743955));
#70709=CARTESIAN_POINT('Ctrl Pts',(-7.32595762451067,-5.07343998582116,
30.3309092022018));
#70710=CARTESIAN_POINT('Ctrl Pts',(-0.971692979062693,-8.25240837045328,
30.5961020840741));
#70711=CARTESIAN_POINT('Ctrl Pts',(3.98328725484426,-6.74026625547534,30.808256389572));
#70712=CARTESIAN_POINT('Ctrl Pts',(7.69776696987758,-3.12902777804056,31.0204106950699));
#70713=CARTESIAN_POINT('Ctrl Pts',(7.97772549360841,3.97055970292418,31.2856035769423));
#70714=CARTESIAN_POINT('Ctrl Pts',(0.960562258670931,8.85856665718801,31.603835035189));
#70715=CARTESIAN_POINT('Ctrl Pts',(-6.92638925711606,5.59536497980034,31.9220664934359));
#70716=CARTESIAN_POINT('Ctrl Pts',(-8.45868859628192,-2.80133366519539,
32.2402979516827));
#70717=CARTESIAN_POINT('Ctrl Pts',(-2.20476864460852,-8.63414405888652,
32.5585294099295));
#70718=CARTESIAN_POINT('Ctrl Pts',(4.67732180358315,-6.86797582290539,32.8237222918018));
#70719=CARTESIAN_POINT('Ctrl Pts',(7.42701215729331,-2.47734877736705,33.0358765972997));
#70720=CARTESIAN_POINT('Ctrl Pts',(7.86373539481082,2.68478989842535,33.2480309027976));
#70721=CARTESIAN_POINT('Ctrl Pts',(3.4200181553324,8.22878631531108,33.5132237846699));
#70722=CARTESIAN_POINT('Ctrl Pts',(-5.08317498807606,7.3183478404094,33.8314552429168));
#70723=CARTESIAN_POINT('Ctrl Pts',(-8.89845997676324,-0.316839770565183,
34.1496867011636));
#70724=CARTESIAN_POINT('Ctrl Pts',(-4.54980615681072,-7.66134107112282,
34.4679181594104));
#70725=CARTESIAN_POINT('Ctrl Pts',(3.99660594150553,-7.96470899369072,34.7861496176572));
#70726=CARTESIAN_POINT('Ctrl Pts',(8.03476930536867,-2.11870558780435,35.0513424995296));
#70727=CARTESIAN_POINT('Ctrl Pts',(7.23200986308717,2.99929989989564,35.2634968050274));
#70728=CARTESIAN_POINT('Ctrl Pts',(4.17701215284028,7.18324443641673,35.4756511105253));
#70729=CARTESIAN_POINT('Ctrl Pts',(-2.81326380316848,8.4554713162329,35.7408439923976));
#70730=CARTESIAN_POINT('Ctrl Pts',(-8.6365046950554,2.19263989859547,36.0590754506445));
#70731=CARTESIAN_POINT('Ctrl Pts',(-6.51089486438885,-6.07381473730833,
36.3773069088913));
#70732=CARTESIAN_POINT('Ctrl Pts',(1.58816963159744,-8.76781616446756,36.6955383671382));
#70733=CARTESIAN_POINT('Ctrl Pts',(8.23991738921627,-3.39311211496841,37.0137698253849));
#70734=CARTESIAN_POINT('Ctrl Pts',(7.45573024013204,3.66858525111086,37.2789627072573));
#70735=CARTESIAN_POINT('Ctrl Pts',(3.49381813846497,7.00649708232563,37.4911170127552));
#70736=CARTESIAN_POINT('Ctrl Pts',(-1.55616091301732,8.16240126256267,37.7032713182531));
#70737=CARTESIAN_POINT('Ctrl Pts',(-7.66823921050773,4.53955458346809,37.9684642001254));
#70738=CARTESIAN_POINT('Ctrl Pts',(-7.95853871375751,-4.00731139471962,
38.2866956583722));
#70739=CARTESIAN_POINT('Ctrl Pts',(-0.933437273603877,-8.85503654732807,
38.604927116619));
#70740=CARTESIAN_POINT('Ctrl Pts',(6.94805109229926,-5.578661944537,38.9231585748658));
#70741=CARTESIAN_POINT('Ctrl Pts',(8.44623376174194,2.84087726730062,39.2413900331127));
#70742=CARTESIAN_POINT('Ctrl Pts',(3.22389408487697,7.65852062005342,39.506582914985));
#70743=CARTESIAN_POINT('Ctrl Pts',(-1.95610514271807,7.58099064898092,39.7187372204829));
#70744=CARTESIAN_POINT('Ctrl Pts',(-6.52692173063208,5.1425406056238,39.9308915259807));
#70745=CARTESIAN_POINT('Ctrl Pts',(-8.76630268949753,-1.60043292954236,
40.1960844078531));
#70746=CARTESIAN_POINT('Ctrl Pts',(-3.38143393342795,-8.2439546108945,40.5143158660999));
#70747=CARTESIAN_POINT('Ctrl Pts',(5.10134063952619,-7.2978970311856,40.8325473243467));
#70748=CARTESIAN_POINT('Ctrl Pts',(8.90386346870972,0.343654482297748,41.1507787825936));
#70749=CARTESIAN_POINT('Ctrl Pts',(4.51447416949656,7.68303139254309,41.4690102408403));
#70750=CARTESIAN_POINT('Ctrl Pts',(-2.58742933084496,7.89630550423239,41.7342031227127));
#70751=CARTESIAN_POINT('Ctrl Pts',(-6.44767089982784,4.44131810578996,41.9463574282106));
#70752=CARTESIAN_POINT('Ctrl Pts',(-8.29993800323926,-0.396812677055769,
42.1585117337085));
#70753=CARTESIAN_POINT('Ctrl Pts',(-5.56947835427224,-6.95631793890613,
42.4237046155808));
#70754=CARTESIAN_POINT('Ctrl Pts',(2.85234184146494,-8.44162478981714,42.7419360738277));
#70755=CARTESIAN_POINT('Ctrl Pts',(8.63681108804976,-2.16528788561929,43.0601675320744));
#70756=CARTESIAN_POINT('Ctrl Pts',(6.49739267219132,6.0976037536053,43.3783989903213));
#70757=CARTESIAN_POINT('Ctrl Pts',(-1.62906851819094,8.76102643352332,43.6966304485681));
#70758=CARTESIAN_POINT('Ctrl Pts',(-7.13108961687574,4.26544159898762,43.9618233304404));
#70759=CARTESIAN_POINT('Ctrl Pts',(-7.78031959023451,-0.874296072916558,
44.1739776359383));
#70760=CARTESIAN_POINT('Ctrl Pts',(-6.00655321128364,-5.74175493018522,
44.3861319414362));
#70761=CARTESIAN_POINT('Ctrl Pts',(0.356008857715901,-8.90408367543134,
44.6513248233086));
#70762=CARTESIAN_POINT('Ctrl Pts',(7.68866550332958,-4.50347708449103,44.9695562815553));
#70763=CARTESIAN_POINT('Ctrl Pts',(7.94083573671719,4.02816399873989,45.2877877398022));
#70764=CARTESIAN_POINT('Ctrl Pts',(0.907644546520611,8.86414487978386,45.606019198049));
#70765=CARTESIAN_POINT('Ctrl Pts',(-6.97447922537052,5.54671866428513,45.9242506562958));
#70766=CARTESIAN_POINT('Ctrl Pts',(-8.18100447996011,-1.45519650121904,
46.1894435381681));
#70767=CARTESIAN_POINT('Ctrl Pts',(-5.30114464388381,-5.76156506636232,
46.401597843666));
#70768=CARTESIAN_POINT('Ctrl Pts',(-0.770368802850766,-8.27363058553387,
46.6137521491639));
#70769=CARTESIAN_POINT('Ctrl Pts',(6.10707611651337,-6.48945835281855,46.8789450310363));
#70770=CARTESIAN_POINT('Ctrl Pts',(8.75806975259084,1.64106589793963,47.197176489283));
#70771=CARTESIAN_POINT('Ctrl Pts',(3.35439483242474,8.24809145842061,47.51540794753));
#70772=CARTESIAN_POINT('Ctrl Pts',(-5.12678723206113,7.28786222083,47.8336394057766));
#70773=CARTESIAN_POINT('Ctrl Pts',(-8.90287287341688,-0.385101292691789,
48.1518708640236));
#70774=CARTESIAN_POINT('Ctrl Pts',(-5.2227875577806,-6.46288799876496,48.4170637458958));
#70775=CARTESIAN_POINT('Ctrl Pts',(-0.224771957636989,-7.82606185232166,
48.6292180513938));
#70776=CARTESIAN_POINT('Ctrl Pts',(4.84324354766974,-6.75199400890155,48.8413723568916));
#70777=CARTESIAN_POINT('Ctrl Pts',(8.86609442122669,-0.895442974034532,
49.106565238764));
#70778=CARTESIAN_POINT('Ctrl Pts',(5.53661976275402,6.98159900562246,49.4247966970108));
#70779=CARTESIAN_POINT('Ctrl Pts',(-2.87546975915461,8.42701910894097,49.7430281552576));
#70780=CARTESIAN_POINT('Ctrl Pts',(-8.64944445882054,2.14102630212842,50.0612596135045));
#70781=CARTESIAN_POINT('Ctrl Pts',(-6.46946867237072,-6.12824799621133,
50.3794910717512));
#70782=CARTESIAN_POINT('Ctrl Pts',(0.294237499671178,-8.30420709352041,
50.6446839536236));
#70783=CARTESIAN_POINT('Ctrl Pts',(4.96172359066756,-6.05632442650801,50.8568382591214));
#70784=CARTESIAN_POINT('Ctrl Pts',(8.08399832859222,-1.9223428886662,51.0689925646194));
#70785=CARTESIAN_POINT('Ctrl Pts',(7.28133379904682,5.13727812296675,51.3341854464917));
#70786=CARTESIAN_POINT('Ctrl Pts',(-0.397394644859894,8.90162684956315,
51.6524169047385));
#70787=CARTESIAN_POINT('Ctrl Pts',(-7.69655114233151,4.47728465833303,51.9706483629853));
#70788=CARTESIAN_POINT('Ctrl Pts',(-7.93446639944908,-4.05476584140684,
52.2888798212321));
#70789=CARTESIAN_POINT('Ctrl Pts',(-0.866467989252532,-8.86897297489713,
52.607111279479));
#70790=CARTESIAN_POINT('Ctrl Pts',(5.66710633795237,-6.07703356191387,52.8723041613512));
#70791=CARTESIAN_POINT('Ctrl Pts',(7.71731446434895,-1.31940289815309,53.0844584668492));
#70792=CARTESIAN_POINT('Ctrl Pts',(7.36414769336802,3.84912456391707,53.296612772347));
#70793=CARTESIAN_POINT('Ctrl Pts',(2.12921839658729,8.65308485024211,53.5618056542195));
#70794=CARTESIAN_POINT('Ctrl Pts',(-6.13671289856523,6.46046731074539,53.8800371124662));
#70795=CARTESIAN_POINT('Ctrl Pts',(-8.74684968997108,-1.66601257477884,
54.1982685707131));
#70796=CARTESIAN_POINT('Ctrl Pts',(-3.33214332607097,-8.26400047961927,
54.5165000289599));
#70797=CARTESIAN_POINT('Ctrl Pts',(5.16104265436551,-7.26450873257612,54.8347314872066));
#70798=CARTESIAN_POINT('Ctrl Pts',(8.26348127511696,-0.872529870021032,
55.0999243690791));
#70799=CARTESIAN_POINT('Ctrl Pts',(6.69194989702022,4.06393566940663,55.3120786745769));
#70800=CARTESIAN_POINT('Ctrl Pts',(3.03636914251083,7.73478465044085,55.5242329800748));
#70801=CARTESIAN_POINT('Ctrl Pts',(-4.06606816584847,7.92947274896181,55.7894258619471));
#70802=CARTESIAN_POINT('Ctrl Pts',(-8.86946220514079,0.854121340446415,
56.1076573201939));
#70803=CARTESIAN_POINT('Ctrl Pts',(-5.51179106060672,-6.99307777037299,
56.4258887784408));
#70804=CARTESIAN_POINT('Ctrl Pts',(2.90270172073915,-8.42444097807349,56.7441202366875));
#70805=CARTESIAN_POINT('Ctrl Pts',(8.65999593577497,-2.10093284000611,57.0623516949345));
#70806=CARTESIAN_POINT('Ctrl Pts',(6.81131644716327,4.75945368870117,57.3275445768066));
#70807=CARTESIAN_POINT('Ctrl Pts',(2.38798828780706,7.4562241440692,57.5396988823047));
#70808=CARTESIAN_POINT('Ctrl Pts',(-2.77902229276694,7.8309301015008,57.7518531878024));
#70809=CARTESIAN_POINT('Ctrl Pts',(-8.26925985820949,3.32096218034177,58.0170460696748));
#70810=CARTESIAN_POINT('Ctrl Pts',(-7.25678260140303,-5.17068557819958,
58.3352775279216));
#70811=CARTESIAN_POINT('Ctrl Pts',(0.423667623282275,-8.89401389380803,
58.6535089861685));
#70812=CARTESIAN_POINT('Ctrl Pts',(7.71542176339676,-4.45748248291911,58.9717404444153));
#70813=CARTESIAN_POINT('Ctrl Pts',(7.91614443013644,4.0919562274143,59.2899719026621));
#70814=CARTESIAN_POINT('Ctrl Pts',(2.02207314452598,8.05963096900062,59.5551647845345));
#70815=CARTESIAN_POINT('Ctrl Pts',(-3.08592400199076,7.19547354961726,59.7673190900323));
#70816=CARTESIAN_POINT('Ctrl Pts',(-7.23288317138988,4.0904562321718,59.9794733955303));
#70817=CARTESIAN_POINT('Ctrl Pts',(-8.42108067557773,-2.91459236622659,
60.2446662774025));
#70818=CARTESIAN_POINT('Ctrl Pts',(-2.08877662244061,-8.66221076251164,
60.5628977356495));
#70819=CARTESIAN_POINT('Ctrl Pts',(6.15155819357058,-6.43749246130692,60.8811291938961));
#70820=CARTESIAN_POINT('Ctrl Pts',(8.74811365885818,1.69333708526246,61.1993606521431));
#70821=CARTESIAN_POINT('Ctrl Pts',(3.29392442037457,8.28006704796012,61.5175921103899));
#70822=CARTESIAN_POINT('Ctrl Pts',(-3.75784748417278,7.41114117015618,61.7827849922621));
#70823=CARTESIAN_POINT('Ctrl Pts',(-7.04794492079813,3.40943381556233,61.9949392977601));
#70824=CARTESIAN_POINT('Ctrl Pts',(-8.14312675835125,-1.65406098911481,
62.2070936032579));
#70825=CARTESIAN_POINT('Ctrl Pts',(-4.44714881737489,-7.72219630687904,
62.4722864851303));
#70826=CARTESIAN_POINT('Ctrl Pts',(4.10258681748251,-7.90984604639341,62.7905179433771));
#70827=CARTESIAN_POINT('Ctrl Pts',(8.86560663909921,-0.82704069974108,63.1087494016239));
#70828=CARTESIAN_POINT('Ctrl Pts',(5.49482911914465,7.01453747755524,63.4269808598707));
#70829=CARTESIAN_POINT('Ctrl Pts',(-2.94209291707492,8.4115122108425,63.7452123181176));
#70830=CARTESIAN_POINT('Ctrl Pts',(-7.69668026328262,3.13169987116955,64.0104051999898));
#70831=CARTESIAN_POINT('Ctrl Pts',(-7.55695562221244,-2.04699493727171,
64.2225595054878));
#70832=CARTESIAN_POINT('Ctrl Pts',(-5.06379604896171,-6.58820163115909,
64.4347138109856));
#70833=CARTESIAN_POINT('Ctrl Pts',(1.70558132560844,-8.74645303809441,64.699906692858));
#70834=CARTESIAN_POINT('Ctrl Pts',(8.28396374960744,-3.28219860273811,65.0181381511048));
#70835=CARTESIAN_POINT('Ctrl Pts',(7.23611513756351,5.18860435128682,65.3363696093517));
#70836=CARTESIAN_POINT('Ctrl Pts',(-0.450545285693165,8.89909501118893,
65.6546010675985));
#70837=CARTESIAN_POINT('Ctrl Pts',(-7.73668626251787,4.42189259042114,65.9728325258452));
#70838=CARTESIAN_POINT('Ctrl Pts',(-7.86466694643391,-2.68205983899581,
66.2380254077176));
#70839=CARTESIAN_POINT('Ctrl Pts',(-4.36357573046525,-6.50053639277595,
66.4501797132155));
#70840=CARTESIAN_POINT('Ctrl Pts',(0.496447847513485,-8.29457477469306,
66.6623340187134));
#70841=CARTESIAN_POINT('Ctrl Pts',(7.02269345367981,-5.48554692455582,66.9275269005857));
#70842=CARTESIAN_POINT('Ctrl Pts',(8.40676590719256,2.95350132120013,67.2457583588326));
#70843=CARTESIAN_POINT('Ctrl Pts',(2.06142290233261,8.66218869662343,67.5639898170793));
#70844=CARTESIAN_POINT('Ctrl Pts',(-6.17518336350058,6.42370558944248,67.8822212753262));
#70845=CARTESIAN_POINT('Ctrl Pts',(-8.74083331285178,-1.73415149367768,
68.200452733573));
#70846=CARTESIAN_POINT('Ctrl Pts',(-4.17950556618231,-7.18179395276235,
68.4656456154453));
#70847=CARTESIAN_POINT('Ctrl Pts',(0.967657358324997,-7.7692603114335,68.6777999209432));
#70848=CARTESIAN_POINT('Ctrl Pts',(5.81346630611157,-5.93717446815899,68.8899542264411));
#70849=CARTESIAN_POINT('Ctrl Pts',(8.89916685337432,0.462901414379444,69.1551471083135));
#70850=CARTESIAN_POINT('Ctrl Pts',(4.41082864532226,7.74218791697406,69.4733785665602));
#70851=CARTESIAN_POINT('Ctrl Pts',(-4.12322534511683,7.89189395162231,69.7916100248071));
#70852=CARTESIAN_POINT('Ctrl Pts',(-8.87440460098803,0.801140462714857,
70.1098414830539));
#70853=CARTESIAN_POINT('Ctrl Pts',(-5.46257080013168,-7.04058014016515,
70.4280729413007));
#70854=CARTESIAN_POINT('Ctrl Pts',(1.55332724194812,-8.16294098784365,70.6932658231731));
#70855=CARTESIAN_POINT('Ctrl Pts',(5.82480462436658,-5.23157888833839,70.9054201286709));
#70856=CARTESIAN_POINT('Ctrl Pts',(8.28228451238616,-0.670965362211112,
71.1175744341688));
#70857=CARTESIAN_POINT('Ctrl Pts',(6.41565808435416,6.18455973878933,71.3827673160413));
#70858=CARTESIAN_POINT('Ctrl Pts',(-1.7461124788672,8.73773283559258,71.7009987742879));
#70859=CARTESIAN_POINT('Ctrl Pts',(-8.28777566778471,3.25511168110842,72.0192302325349));
#70860=CARTESIAN_POINT('Ctrl Pts',(-7.22577540229245,-5.21392843232479,
72.3374616907816));
#70861=CARTESIAN_POINT('Ctrl Pts',(0.491977031632255,-8.89760716286088,
72.6556931490285));
#70862=CARTESIAN_POINT('Ctrl Pts',(6.52513642017948,-5.1448054901349,72.9208860309008));
#70863=CARTESIAN_POINT('Ctrl Pts',(7.82819621279558,-0.130783009644597,
73.1330403363986));
#70864=CARTESIAN_POINT('Ctrl Pts',(6.69335167471002,4.92397282854073,73.3451946418965));
#70865=CARTESIAN_POINT('Ctrl Pts',(0.788914170526756,8.87620315361264,73.6103875237689));
#70866=CARTESIAN_POINT('Ctrl Pts',(-7.04757446693429,5.45239440729228,73.9286189820157));
#70867=CARTESIAN_POINT('Ctrl Pts',(-8.39189027916964,-2.97646549122528,
74.2468504402625));
#70868=CARTESIAN_POINT('Ctrl Pts',(-2.0369986587134,-8.67450464967492,74.5650818985094));
#70869=CARTESIAN_POINT('Ctrl Pts',(6.20546487108924,-6.39546559481504,74.8833133567561));
#70870=CARTESIAN_POINT('Ctrl Pts',(8.30011932254924,0.394018620431757,75.1485062386285));
#70871=CARTESIAN_POINT('Ctrl Pts',(5.99624970692194,5.03397230856475,75.3606605441264));
#70872=CARTESIAN_POINT('Ctrl Pts',(1.82527669381207,8.10678228177219,75.5728148496243));
#70873=CARTESIAN_POINT('Ctrl Pts',(-5.22464446873074,7.21851914475899,75.8380077314966));
#70874=CARTESIAN_POINT('Ctrl Pts',(-8.89570313556121,-0.503244254885089,
76.1562391897434));
#70875=CARTESIAN_POINT('Ctrl Pts',(-4.38547461718753,-7.75160266377331,
76.4744706479903));
#70876=CARTESIAN_POINT('Ctrl Pts',(4.15149904988012,-7.88174229677711,76.792702106237));
#70877=CARTESIAN_POINT('Ctrl Pts',(8.87536596716089,-0.766558926037482,
77.1109335644839));
#70878=CARTESIAN_POINT('Ctrl Pts',(5.44141995481121,7.05320883494485,77.4291650227306));
#70879=CARTESIAN_POINT('Ctrl Pts',(-2.99144476000515,8.38874184385539,77.7473964809775));
#70880=CARTESIAN_POINT('Ctrl Pts',(-8.67768211916483,2.02104480277786,78.0656279392244));
#70881=CARTESIAN_POINT('Ctrl Pts',(-6.38495741585981,-6.215806244209,78.3838593974711));
#70882=CARTESIAN_POINT('Ctrl Pts',(0.408261456794656,-8.29969135305192,
78.6490522793435));
#70883=CARTESIAN_POINT('Ctrl Pts',(5.04432974985822,-5.98753915443177,78.8612065848413));
#70884=CARTESIAN_POINT('Ctrl Pts',(8.1096459834569,-1.81131815670348,79.0733608903393));
#70885=CARTESIAN_POINT('Ctrl Pts',(7.21013264266632,5.23677016069477,79.3385537722116));
#70886=CARTESIAN_POINT('Ctrl Pts',(-0.519506660206221,8.89530816120681,
79.6567852304584));
#70887=CARTESIAN_POINT('Ctrl Pts',(-7.75727281269671,4.37125700313697,79.9750166887053));
#70888=CARTESIAN_POINT('Ctrl Pts',(-7.87807304156925,-4.16327704955559,
80.2932481469521));
#70889=CARTESIAN_POINT('Ctrl Pts',(-0.744678280256665,-8.88002377539462,
80.6114796051989));
#70890=CARTESIAN_POINT('Ctrl Pts',(5.74996890814574,-5.99869340881063,80.8766724870712));
#70891=CARTESIAN_POINT('Ctrl Pts',(7.73469374172735,-1.2133725163044,81.0888267925691));
#70892=CARTESIAN_POINT('Ctrl Pts',(7.31063264471332,3.94982014366829,81.300981098067));
#70893=CARTESIAN_POINT('Ctrl Pts',(2.01027089758208,8.68148982275397,81.5661739799393));
#70894=CARTESIAN_POINT('Ctrl Pts',(-6.22479241150601,6.37564422591442,81.8844054381861));
#70895=CARTESIAN_POINT('Ctrl Pts',(-8.72316326161886,-1.78588921469291,
82.202636896433));
#70896=CARTESIAN_POINT('Ctrl Pts',(-3.21842208457843,-8.30894958346396,
82.5208683546798));
#70897=CARTESIAN_POINT('Ctrl Pts',(5.26024800698969,-7.19299928562165,82.8390998129265));
#70898=CARTESIAN_POINT('Ctrl Pts',(8.27467693081562,-0.759047397747646,
83.1042926947989));
#70899=CARTESIAN_POINT('Ctrl Pts',(6.635550072064,4.155387084025,83.3164470002968));
#70900=CARTESIAN_POINT('Ctrl Pts',(2.92993823680416,7.77572459775343,83.5286013057947));
#70901=CARTESIAN_POINT('Ctrl Pts',(-4.17450198580167,7.87292713208229,83.7937941876671));
#70902=CARTESIAN_POINT('Ctrl Pts',(-8.88034817145485,0.73232466623441,84.1120256459139));
#70903=CARTESIAN_POINT('Ctrl Pts',(-5.41530554855583,-7.06805795152009,
84.4302571041607));
#70904=CARTESIAN_POINT('Ctrl Pts',(3.01803757251667,-8.38381370803362,84.7484885624074));
#70905=CARTESIAN_POINT('Ctrl Pts',(8.68801170750906,-1.9818932801281,85.0667200206544));
#70906=CARTESIAN_POINT('Ctrl Pts',(6.74536074204024,4.85247767819652,85.3319129025265));
#70907=CARTESIAN_POINT('Ctrl Pts',(2.28544114099461,7.48829255177608,85.5440672080246));
#70908=CARTESIAN_POINT('Ctrl Pts',(-2.88622499993125,7.79205598077012,85.7562215135223));
#70909=CARTESIAN_POINT('Ctrl Pts',(-8.31405497107321,3.2071698339903,86.0214143953948));
#70910=CARTESIAN_POINT('Ctrl Pts',(-7.18514158490123,-5.26978400673226,
86.3396458536415));
#70911=CARTESIAN_POINT('Ctrl Pts',(0.545680896665126,-8.88736236220775,
86.6578773118885));
#70912=CARTESIAN_POINT('Ctrl Pts',(7.77586557562302,-4.35118347378131,86.9761087701351));
#70913=CARTESIAN_POINT('Ctrl Pts',(7.85924480189443,4.20020470331594,87.294340228382));
#70914=CARTESIAN_POINT('Ctrl Pts',(1.91127986077075,8.08662107756309,87.5595331102544));
#70915=CARTESIAN_POINT('Ctrl Pts',(-3.18437739528528,7.15244763376184,87.7716874157523));
#70916=CARTESIAN_POINT('Ctrl Pts',(-7.28833569557586,3.99081369483458,87.9838417212501));
#70917=CARTESIAN_POINT('Ctrl Pts',(-8.38029054540848,-3.02988098452613,
88.2490346031225));
#70918=CARTESIAN_POINT('Ctrl Pts',(-1.96970781328168,-8.69005950514289,
88.5672660613693));
#70919=CARTESIAN_POINT('Ctrl Pts',(6.23932108218079,-6.35246801107428,88.8854975196161));
#70920=CARTESIAN_POINT('Ctrl Pts',(8.72405210414693,1.81322860024798,89.2037289778631));
#70921=CARTESIAN_POINT('Ctrl Pts',(3.17998631222084,8.32449010209889,89.5219604361096));
#70922=CARTESIAN_POINT('Ctrl Pts',(-3.85919722697625,7.35887409333698,89.7871533179823));
#70923=CARTESIAN_POINT('Ctrl Pts',(-7.09406914206523,3.3123933276262,89.9993076234798));
#70924=CARTESIAN_POINT('Ctrl Pts',(-8.11966116127032,-1.76565392544688,
90.2114619289779));
#70925=CARTESIAN_POINT('Ctrl Pts',(-4.34075781378223,-7.7824976715668,90.4766548108502));
#70926=CARTESIAN_POINT('Ctrl Pts',(4.21074785918872,-7.85280112692049,90.7948862690971));
#70927=CARTESIAN_POINT('Ctrl Pts',(8.87612133939328,-0.705299487194537,
91.1131177273438));
#70928=CARTESIAN_POINT('Ctrl Pts',(5.39805071105593,7.08928286877416,91.4313491855907));
#70929=CARTESIAN_POINT('Ctrl Pts',(-3.05724763706058,8.37034558973175,91.7495806438375));
#70930=CARTESIAN_POINT('Ctrl Pts',(-7.73893203375542,3.02578289624382,92.0147735257097));
#70931=CARTESIAN_POINT('Ctrl Pts',(-7.52815296260325,-2.15050680560483,
92.2269278312078));
#70932=CARTESIAN_POINT('Ctrl Pts',(-4.97290886575827,-6.65707207195101,
92.4390821367053));
#70933=CARTESIAN_POINT('Ctrl Pts',(1.82544889879216,-8.72222361119875,92.7042750185781));
#70934=CARTESIAN_POINT('Ctrl Pts',(8.32822552260333,-3.1682081240484,93.0225064768246));
#70935=CARTESIAN_POINT('Ctrl Pts',(7.16423016666839,5.28741747143791,93.3407379350716));
#70936=CARTESIAN_POINT('Ctrl Pts',(-0.572625756648104,8.89207415710469,
93.6589693933183));
#70937=CARTESIAN_POINT('Ctrl Pts',(-7.79663966979729,4.31530511843589,93.9772008515652));
#70938=CARTESIAN_POINT('Ctrl Pts',(-7.82712027134826,-2.78973464977167,
94.2423937334375));
#70939=CARTESIAN_POINT('Ctrl Pts',(-4.27395752016678,-6.55980591672602,
94.4545480389354));
#70940=CARTESIAN_POINT('Ctrl Pts',(0.610228122964827,-8.28698092167651,
94.6667023444334));
#70941=CARTESIAN_POINT('Ctrl Pts',(7.09731069668704,-5.38865746550544,94.9318952263055));
#70942=CARTESIAN_POINT('Ctrl Pts',(8.36544317470014,3.06858983304855,95.2501266845525));
#70943=CARTESIAN_POINT('Ctrl Pts',(1.94235697177152,8.68966206434282,95.5683581427993));
#70944=CARTESIAN_POINT('Ctrl Pts',(-6.26275482923662,6.33835822760918,95.886589601046));
#70945=CARTESIAN_POINT('Ctrl Pts',(-8.71621234473839,-1.85393925663286,
96.2048210592929));
#70946=CARTESIAN_POINT('Ctrl Pts',(-4.08055574434818,-7.23847331801081,
96.4700139411653));
#70947=CARTESIAN_POINT('Ctrl Pts',(1.07418433525722,-7.755249484265,96.6821682466631));
#70948=CARTESIAN_POINT('Ctrl Pts',(5.89439513289042,-5.85683678922722,96.8943225521609));
#70949=CARTESIAN_POINT('Ctrl Pts',(8.89197642862596,0.584981707931448,97.1595154340334));
#70950=CARTESIAN_POINT('Ctrl Pts',(4.30416671541171,7.80198897452233,97.47774689228));
#70951=CARTESIAN_POINT('Ctrl Pts',(-4.23113808520321,7.83456749937178,97.7959783505271));
#70952=CARTESIAN_POINT('Ctrl Pts',(-8.88456304270969,0.679280952731093,
98.1142098087737));
#70953=CARTESIAN_POINT('Ctrl Pts',(-5.36543804313997,-7.11488039330814,
98.4324412670207));
#70954=CARTESIAN_POINT('Ctrl Pts',(1.6652015737725,-8.14085590567682,98.6976341488928));
#70955=CARTESIAN_POINT('Ctrl Pts',(5.8960494494909,-5.15115204963536,98.9097884543909));
#70956=CARTESIAN_POINT('Ctrl Pts',(8.29071230177075,-0.557243831330223,
99.1219427598887));
#70957=CARTESIAN_POINT('Ctrl Pts',(6.33018282299873,6.27201991652337,99.3871356417611));
#70958=CARTESIAN_POINT('Ctrl Pts',(-1.86585659316359,8.71294796532002,99.7053671000079));
#70959=CARTESIAN_POINT('Ctrl Pts',(-8.33166531913313,3.14107153822133,100.023598558254));
#70960=CARTESIAN_POINT('Ctrl Pts',(-7.15354396988856,-5.31259745731755,
100.341830016501));
#70961=CARTESIAN_POINT('Ctrl Pts',(0.614033359805018,-8.89001751623139,
100.660061474748));
#70962=CARTESIAN_POINT('Ctrl Pts',(6.59512418931417,-5.05477675924581,100.92525435662));
#70963=CARTESIAN_POINT('Ctrl Pts',(7.82925422086814,-0.0233429715947194,
101.137408662118));
#70964=CARTESIAN_POINT('Ctrl Pts',(6.62514836783461,5.01536043195949,101.349562967616));
#70965=CARTESIAN_POINT('Ctrl Pts',(0.667033260221919,8.88619800790035,101.614755849489));
#70966=CARTESIAN_POINT('Ctrl Pts',(-7.12173798479913,5.35515930187859,101.932987307735));
#70967=CARTESIAN_POINT('Ctrl Pts',(-8.3502472770763,-3.09133430899154,102.251218765982));
#70968=CARTESIAN_POINT('Ctrl Pts',(-1.91777837929849,-8.70166703342075,
102.569450224229));
#70969=CARTESIAN_POINT('Ctrl Pts',(6.29267047856448,-6.30965503447365,102.887681682476));
#70970=CARTESIAN_POINT('Ctrl Pts',(8.29388772705463,0.507796740143256,103.152874564348));
#70971=CARTESIAN_POINT('Ctrl Pts',(5.92666073856608,5.1159025635017,103.365028869846));
#70972=CARTESIAN_POINT('Ctrl Pts',(1.71371556531993,8.13078164258935,103.577183175344));
#70973=CARTESIAN_POINT('Ctrl Pts',(-5.32291690737959,7.14674779203716,103.842376057216));
#70974=CARTESIAN_POINT('Ctrl Pts',(-8.88845561260621,-0.626290583798954,
104.160607515463));
#70975=CARTESIAN_POINT('Ctrl Pts',(-4.27778007253026,-7.8091981053967,104.47883897371));
#70976=CARTESIAN_POINT('Ctrl Pts',(4.25756724672461,-7.82751583915647,104.797070431957));
#70977=CARTESIAN_POINT('Ctrl Pts',(8.88833011930044,-0.637993805762063,
105.115301890203));
#70978=CARTESIAN_POINT('Ctrl Pts',(5.92921442111081,5.8215846216282,105.380494772076));
#70979=CARTESIAN_POINT('Ctrl Pts',(1.12040947867581,7.74870628875543,105.592649077574));
#70980=CARTESIAN_POINT('Ctrl Pts',(-4.03732047235829,7.26267681793464,105.804803383071));
#70981=CARTESIAN_POINT('Ctrl Pts',(-8.70500241740163,1.90588072000468,106.069996264944));
#70982=CARTESIAN_POINT('Ctrl Pts',(-6.30043886151629,-6.30090098517042,
106.388227723191));
#70983=CARTESIAN_POINT('Ctrl Pts',(1.89050633381148,-8.70108977083264,106.706459181437));
#70984=CARTESIAN_POINT('Ctrl Pts',(8.34699657099074,-3.11841807917011,107.024690639684));
#70985=CARTESIAN_POINT('Ctrl Pts',(7.12931686426273,5.34624068433073,107.342922097931));
#70986=CARTESIAN_POINT('Ctrl Pts',(0.659632208062281,8.28319482496793,107.608114979804));
#70987=CARTESIAN_POINT('Ctrl Pts',(-4.2347656761952,6.58517472942241,107.820269285301));
#70988=CARTESIAN_POINT('Ctrl Pts',(-7.81034604051588,2.83635785571642,108.032423590799));
#70989=CARTESIAN_POINT('Ctrl Pts',(-7.82223304738392,-4.2687373494125,108.297616472671));
#70990=CARTESIAN_POINT('Ctrl Pts',(-0.625638656901327,-8.88850152408258,
108.615847930918));
#70991=CARTESIAN_POINT('Ctrl Pts',(7.13257413883672,-5.3300434850258,108.934079389165));
#70992=CARTESIAN_POINT('Ctrl Pts',(8.34696935607174,3.11849092373627,109.252310847412));
#70993=CARTESIAN_POINT('Ctrl Pts',(1.87742671362308,8.71118346384865,109.570542305659));
#70994=CARTESIAN_POINT('Ctrl Pts',(-4.93312460123469,6.68660697416714,109.835735187531));
#70995=CARTESIAN_POINT('Ctrl Pts',(-7.51519573692979,2.19535864608411,110.047889493029));
#70996=CARTESIAN_POINT('Ctrl Pts',(-7.75683706813093,-2.97958216143764,
110.260043798527));
#70997=CARTESIAN_POINT('Ctrl Pts',(-3.10710531773438,-8.35196653192304,
110.525236680399));
#70998=CARTESIAN_POINT('Ctrl Pts',(5.35568163249784,-7.12134519061905,110.843468138646));
#70999=CARTESIAN_POINT('Ctrl Pts',(8.88016920684646,0.652358993226878,111.161699596893));
#71000=CARTESIAN_POINT('Ctrl Pts',(4.25749893541349,7.82755299487516,111.47993105514));
#71001=CARTESIAN_POINT('Ctrl Pts',(-4.29427392041267,7.80824307397762,111.798162513386));
#71002=CARTESIAN_POINT('Ctrl Pts',(-8.10898828166102,1.81403974768247,112.063355395259));
#71003=CARTESIAN_POINT('Ctrl Pts',(-7.11369468768244,-3.27003278878704,
112.275509700757));
#71004=CARTESIAN_POINT('Ctrl Pts',(-3.90300928623461,-7.33573102491184,
112.487664006255));
#71005=CARTESIAN_POINT('Ctrl Pts',(3.13029117667154,-8.34330423484054,112.752856888127));
#71006=CARTESIAN_POINT('Ctrl Pts',(8.71308479343764,-1.86521753556844,113.071088346374));
#71007=CARTESIAN_POINT('Ctrl Pts',(6.27708966715128,6.31515025227515,113.389319804621));
#71008=CARTESIAN_POINT('Ctrl Pts',(-1.9178543191386,8.70165029653508,113.707551262868));
#71009=CARTESIAN_POINT('Ctrl Pts',(-8.36207449704115,3.07979845311157,114.025782721114));
#71010=CARTESIAN_POINT('Ctrl Pts',(-7.31200318078258,-3.9472826909803,114.290975602987));
#71011=CARTESIAN_POINT('Ctrl Pts',(-3.22697053921716,-7.13333215883917,
114.503129908485));
#71012=CARTESIAN_POINT('Ctrl Pts',(1.86302568448042,-8.09787419371614,114.715284213982));
#71013=CARTESIAN_POINT('Ctrl Pts',(7.83405942370468,-4.24699439035632,114.980477095855));
#71014=CARTESIAN_POINT('Ctrl Pts',(7.80167326373373,4.30473894197645,115.298708554102));
#71015=CARTESIAN_POINT('Ctrl Pts',(0.598666179718408,8.88395048407695,115.616940012348));
#71016=CARTESIAN_POINT('Ctrl Pts',(-7.15359033293806,5.31253502775477,115.935171470595));
#71017=CARTESIAN_POINT('Ctrl Pts',(-8.33303138357817,-3.15753643940262,
116.253402928842));
#71018=CARTESIAN_POINT('Ctrl Pts',(-2.9326374034684,-7.77470700528744,116.518595810714));
#71019=CARTESIAN_POINT('Ctrl Pts',(2.24074812160043,-7.501787414,116.730750116212));
#71020=CARTESIAN_POINT('Ctrl Pts',(6.71630568958916,-4.89261372297871,116.94290442171));
#71021=CARTESIAN_POINT('Ctrl Pts',(8.69967519683171,1.93005178051923,117.208097303583));
#71022=CARTESIAN_POINT('Ctrl Pts',(3.06797626001352,8.36566821841633,117.526328761829));
#71023=CARTESIAN_POINT('Ctrl Pts',(-5.3730627263302,7.10022354135342,117.844560220076));
#71024=CARTESIAN_POINT('Ctrl Pts',(-8.88455711425019,-0.679358488761448,
118.162791678323));
#71025=CARTESIAN_POINT('Ctrl Pts',(-4.22137371612796,-7.84789477214366,
118.48102313657));
#71026=CARTESIAN_POINT('Ctrl Pts',(2.8835198119009,-7.79305746499169,118.746216018442));
#71027=CARTESIAN_POINT('Ctrl Pts',(6.61065369712302,-4.19488071892606,118.95837032394));
#71028=CARTESIAN_POINT('Ctrl Pts',(8.27905598285984,0.709692321334109,119.170524629438));
#71029=CARTESIAN_POINT('Ctrl Pts',(5.30304606307633,7.16150479010844,119.43571751131));
#71030=CARTESIAN_POINT('Ctrl Pts',(-3.16881895057326,8.32799312746558,119.753948969557));
#71031=CARTESIAN_POINT('Ctrl Pts',(-8.71235895857032,1.83787343832149,120.072180427804));
#71032=CARTESIAN_POINT('Ctrl Pts',(-6.26269951380734,-6.3384128827637,120.390411886051));
#71033=CARTESIAN_POINT('Ctrl Pts',(1.9584679023929,-8.69332225798348,120.708643344297));
#71034=CARTESIAN_POINT('Ctrl Pts',(7.28694984446149,-3.99334360186924,120.97383622617));
#71035=CARTESIAN_POINT('Ctrl Pts',(7.74179179981089,1.16723017339574,121.185990531668));
#71036=CARTESIAN_POINT('Ctrl Pts',(5.7856359711068,5.96429774308113,121.398144837166));
#71037=CARTESIAN_POINT('Ctrl Pts',(-0.691712375729838,8.88431102534787,
121.663337719038));
#71038=CARTESIAN_POINT('Ctrl Pts',(-7.85310994378053,4.21017188289523,121.981569177285));
#71039=CARTESIAN_POINT('Ctrl Pts',(-7.78319610953094,-4.3249087526618,122.299800635532));
#71040=CARTESIAN_POINT('Ctrl Pts',(-0.572548155020054,-8.89207915410175,
122.618032093778));
#71041=CARTESIAN_POINT('Ctrl Pts',(7.17879440645219,-5.27961734179148,122.936263552025));
#71042=CARTESIAN_POINT('Ctrl Pts',(8.12027361919589,1.76283507670944,123.201456433897));
#71043=CARTESIAN_POINT('Ctrl Pts',(5.079982243843,5.95747823760563,123.413610739396));
#71044=CARTESIAN_POINT('Ctrl Pts',(0.457650657432336,8.29680583321317,123.625765044893));
#71045=CARTESIAN_POINT('Ctrl Pts',(-6.34757913366529,6.25441344553678,123.890957926766));
#71046=CARTESIAN_POINT('Ctrl Pts',(-8.68991501323083,-1.97034518180233,
124.209189385012));
#71047=CARTESIAN_POINT('Ctrl Pts',(-3.04080032632442,-8.36878191696348,
124.527420843259));
#71048=CARTESIAN_POINT('Ctrl Pts',(5.39811257940079,-7.08923575942719,124.845652301506));
#71049=CARTESIAN_POINT('Ctrl Pts',(8.88200340851531,0.720738410920663,125.163883759753));
#71050=CARTESIAN_POINT('Ctrl Pts',(4.97521957029455,6.65534532429735,125.429076641625));
#71051=CARTESIAN_POINT('Ctrl Pts',(-0.0706706259259978,7.82897006073825,
125.641230947123));
#71052=CARTESIAN_POINT('Ctrl Pts',(-5.09455212869252,6.56444740753711,125.853385252621));
#71053=CARTESIAN_POINT('Ctrl Pts',(-8.8935669338954,0.560281713227264,126.118578134493));
#71054=CARTESIAN_POINT('Ctrl Pts',(-5.26925699717732,-7.18552807873753,
126.43680959274));
#71055=CARTESIAN_POINT('Ctrl Pts',(3.19137931782936,-8.312525214879,126.755041050987));
#71056=CARTESIAN_POINT('Ctrl Pts',(8.72406792795749,-1.8131524649101,127.073272509233));
#71057=CARTESIAN_POINT('Ctrl Pts',(6.23363916970125,6.36798171384168,127.391503967481));
#71058=CARTESIAN_POINT('Ctrl Pts',(-0.607351258754355,8.28719226317197,
127.656696849353));
#71059=CARTESIAN_POINT('Ctrl Pts',(-5.18669973002471,5.86480284918986,127.868851154851));
#71060=CARTESIAN_POINT('Ctrl Pts',(-8.15077335549712,1.61595942573011,128.081005460349));
#71061=CARTESIAN_POINT('Ctrl Pts',(-7.08231615792921,-5.40834967850552,
128.346198342221));
#71062=CARTESIAN_POINT('Ctrl Pts',(0.732975996233196,-8.88029443552249,
128.664429800468));
#71063=CARTESIAN_POINT('Ctrl Pts',(7.86000171006385,-4.18370057676953,128.982661258715));
#71064=CARTESIAN_POINT('Ctrl Pts',(7.77582760231544,4.35125133400693,129.300892716962));
#71065=CARTESIAN_POINT('Ctrl Pts',(0.53121875048182,8.89535019237527,129.619124175208));
#71066=CARTESIAN_POINT('Ctrl Pts',(-5.89236157539941,5.8588826770164,129.884317057081));
#71067=CARTESIAN_POINT('Ctrl Pts',(-7.76160126238651,1.02728398849821,130.096471362578));
#71068=CARTESIAN_POINT('Ctrl Pts',(-7.21367397715182,-4.12423797926977,
130.308625668076));
#71069=CARTESIAN_POINT('Ctrl Pts',(-1.80121561285219,-8.72726020706794,
130.573818549949));
#71070=CARTESIAN_POINT('Ctrl Pts',(6.37610096134052,-6.2243248311298,130.892050008196));
#71071=CARTESIAN_POINT('Ctrl Pts',(8.67776168515813,1.99485075478615,131.210281466442));
#71072=CARTESIAN_POINT('Ctrl Pts',(3.01796440628899,8.38384004588583,131.528512924689));
#71073=CARTESIAN_POINT('Ctrl Pts',(-5.43146246726779,7.06460642021306,131.846744382936));
#71074=CARTESIAN_POINT('Ctrl Pts',(-8.29051835486879,0.560121920542435,
132.111937264808));
#71075=CARTESIAN_POINT('Ctrl Pts',(-6.53384985640553,-4.31353365620972,
132.324091570306));
#71076=CARTESIAN_POINT('Ctrl Pts',(-2.74236849646545,-7.84384129032964,
132.536245875804));
#71077=CARTESIAN_POINT('Ctrl Pts',(4.3623571968068,-7.77041106334294,132.801438757677));
#71078=CARTESIAN_POINT('Ctrl Pts',(8.89537322696565,-0.518862434187001,
133.119670215923));
#71079=CARTESIAN_POINT('Ctrl Pts',(5.24401287298454,7.19606186648241,133.43790167417));
#71080=CARTESIAN_POINT('Ctrl Pts',(-3.21849461415895,8.308921439709,133.756133132417));
#71081=CARTESIAN_POINT('Ctrl Pts',(-8.73309913861114,1.77268943727978,134.074364590664));
#71082=CARTESIAN_POINT('Ctrl Pts',(-6.62688905221802,-5.01306020788507,
134.339557472536));
#71083=CARTESIAN_POINT('Ctrl Pts',(-2.10495959837391,-7.54101529228778,
134.551711778034));
#71084=CARTESIAN_POINT('Ctrl Pts',(3.07250969152268,-7.72049968290824,134.763866083532));
#71085=CARTESIAN_POINT('Ctrl Pts',(8.38867380742258,-3.00659278228975,135.029058965404));
#71086=CARTESIAN_POINT('Ctrl Pts',(7.05652195652337,5.44080701272625,135.347290423651));
#71087=CARTESIAN_POINT('Ctrl Pts',(-0.758943024948333,8.87169560361212,
135.665521881898));
#71088=CARTESIAN_POINT('Ctrl Pts',(-7.87811174492057,4.16320050047685,135.983753340144));
#71089=CARTESIAN_POINT('Ctrl Pts',(-7.7561154611855,-4.38772393828678,136.301984798392));
#71090=CARTESIAN_POINT('Ctrl Pts',(-1.71653806487965,-8.13018623588088,
136.567177680264));
#71091=CARTESIAN_POINT('Ctrl Pts',(3.35521667026988,-7.07391600493298,136.779331985762));
#71092=CARTESIAN_POINT('Ctrl Pts',(7.38206860175106,-3.81464209557449,136.99148629126));
#71093=CARTESIAN_POINT('Ctrl Pts',(8.3051148879488,3.23025000639687,137.256679173132));
#71094=CARTESIAN_POINT('Ctrl Pts',(1.76045830872135,8.73485372607235,137.574910631379));
#71095=CARTESIAN_POINT('Ctrl Pts',(-6.39006882928428,6.20080621816854,137.893142089625));
#71096=CARTESIAN_POINT('Ctrl Pts',(-8.67799378202421,-2.02220349910113,
138.211373547872));
#71097=CARTESIAN_POINT('Ctrl Pts',(-2.97916651222067,-8.39845314914106,
138.529605006119));
#71098=CARTESIAN_POINT('Ctrl Pts',(4.03479898906111,-7.26407793709282,138.794797887992));
#71099=CARTESIAN_POINT('Ctrl Pts',(7.17156660737976,-3.14108244801377,139.006952193489));
#71100=CARTESIAN_POINT('Ctrl Pts',(8.07491957884542,1.96012881042716,139.219106498987));
#71101=CARTESIAN_POINT('Ctrl Pts',(4.15261858502811,7.88449156846104,139.48429938086));
#71102=CARTESIAN_POINT('Ctrl Pts',(-4.39810931656918,7.74942046298518,139.802530839106));
#71103=CARTESIAN_POINT('Ctrl Pts',(-8.89049863566354,0.491946549468975,
140.120762297353));
#71104=CARTESIAN_POINT('Ctrl Pts',(-5.22625332029457,-7.21686630780536,
140.4389937556));
#71105=CARTESIAN_POINT('Ctrl Pts',(3.25736995078038,-8.29451562236199,140.757225213847));
#71106=CARTESIAN_POINT('Ctrl Pts',(7.80936092757189,-2.83906904833273,141.022418095719));
#71107=CARTESIAN_POINT('Ctrl Pts',(7.4743401689251,2.33066634001897,141.234572401217));
#71108=CARTESIAN_POINT('Ctrl Pts',(4.8116131052624,6.7745708708046,141.446726706715));
#71109=CARTESIAN_POINT('Ctrl Pts',(-2.03437636454388,8.67587236035892,141.711919588587));
#71110=CARTESIAN_POINT('Ctrl Pts',(-8.40190465320179,2.96730201886063,142.030151046834));
#71111=CARTESIAN_POINT('Ctrl Pts',(-7.03519312179721,-5.4579332294636,142.348382505081));
#71112=CARTESIAN_POINT('Ctrl Pts',(0.785993262929414,-8.87575899082768,
142.666613963328));
#71113=CARTESIAN_POINT('Ctrl Pts',(7.89801827216467,-4.12683362620934,142.984845421574));
#71114=CARTESIAN_POINT('Ctrl Pts',(7.75787096340047,2.97688919402482,143.250038303447));
#71115=CARTESIAN_POINT('Ctrl Pts',(4.11519905014968,6.66054827525247,143.462192608945));
#71116=CARTESIAN_POINT('Ctrl Pts',(-0.809054187869451,8.26993727179055,
143.674346914443));
#71117=CARTESIAN_POINT('Ctrl Pts',(-7.22466625302864,5.21667000472345,143.939539796315));
#71118=CARTESIAN_POINT('Ctrl Pts',(-8.28934225165142,-3.26859115029452,
144.257771254562));
#71119=CARTESIAN_POINT('Ctrl Pts',(-1.73312489851915,-8.73379960178476,
144.576002712809));
#71120=CARTESIAN_POINT('Ctrl Pts',(6.41315698889781,-6.18613776991189,144.894234171056));
#71121=CARTESIAN_POINT('Ctrl Pts',(8.66917866521723,2.06271415312468,145.212465629302));
#71122=CARTESIAN_POINT('Ctrl Pts',(3.90555565176804,7.33437565218188,145.477658511175));
#71123=CARTESIAN_POINT('Ctrl Pts',(-1.26010770635471,7.72721781232174,145.689812816672));
#71124=CARTESIAN_POINT('Ctrl Pts',(-6.03334035055086,5.71360091127059,145.90196712217));
#71125=CARTESIAN_POINT('Ctrl Pts',(-8.87536457635244,-0.798343303690664,
146.167160004043));
#71126=CARTESIAN_POINT('Ctrl Pts',(-4.11556997904378,-7.90309855967184,
146.48539146229));
#71127=CARTESIAN_POINT('Ctrl Pts',(4.41805580554583,-7.73070244465686,146.803622920536));
#71128=CARTESIAN_POINT('Ctrl Pts',(8.89831309663174,-0.465732803809564,
147.121854378783));
#71129=CARTESIAN_POINT('Ctrl Pts',(5.19303537004166,7.24167330256215,147.44008583703));
#71130=CARTESIAN_POINT('Ctrl Pts',(-1.86021440597459,8.09852044425502,147.705278718902));
#71131=CARTESIAN_POINT('Ctrl Pts',(-6.01804798899972,5.00807996122836,147.9174330244));
#71132=CARTESIAN_POINT('Ctrl Pts',(-8.30170307445535,0.357991457224306,
148.129587329898));
#71133=CARTESIAN_POINT('Ctrl Pts',(-6.17774214475184,-6.42222300354386,
148.39478021177));
#71134=CARTESIAN_POINT('Ctrl Pts',(2.07454951511027,-8.66562917759421,148.713011670017));
#71135=CARTESIAN_POINT('Ctrl Pts',(8.40469207476932,-2.94009041592513,149.031243128264));
#71136=CARTESIAN_POINT('Ctrl Pts',(7.02390482802235,5.48284888355675,149.349474586511));
#71137=CARTESIAN_POINT('Ctrl Pts',(-0.827338523409895,8.87270948965367,
149.667706044757));
#71138=CARTESIAN_POINT('Ctrl Pts',(-6.71460858458054,4.89494342072968,149.93289892663));
#71139=CARTESIAN_POINT('Ctrl Pts',(-7.8275546617825,-0.164671931225144,
150.145053232128));
#71140=CARTESIAN_POINT('Ctrl Pts',(-6.50280566616276,-5.17301435045905,
150.357207537626));
#71141=CARTESIAN_POINT('Ctrl Pts',(-0.453437149148608,-8.89964261191235,
150.622400419498));
#71142=CARTESIAN_POINT('Ctrl Pts',(7.2482615574515,-5.18261314600062,150.940631877745));
#71143=CARTESIAN_POINT('Ctrl Pts',(8.27364207620721,3.29099750241855,151.258863335992));
#71144=CARTESIAN_POINT('Ctrl Pts',(1.70819408117098,8.74514775907524,151.577094794239));
#71145=CARTESIAN_POINT('Ctrl Pts',(-6.44223380417698,6.15684971685954,151.895326252485));
#71146=CARTESIAN_POINT('Ctrl Pts',(-8.27954809599393,-0.707037044381812,
152.160519134358));
#71147=CARTESIAN_POINT('Ctrl Pts',(-5.8017705655009,-5.25645685740221,152.372673439856));
#71148=CARTESIAN_POINT('Ctrl Pts',(-1.51877066045986,-8.17030114169019,
152.584827745354));
#71149=CARTESIAN_POINT('Ctrl Pts',(5.49470260574753,-7.01535214655366,152.850020627226));
#71150=CARTESIAN_POINT('Ctrl Pts',(8.86799849696601,0.837016960770842,153.168252085473));
#71151=CARTESIAN_POINT('Ctrl Pts',(4.09424988831707,7.91433764660141,153.48648354372));
#71152=CARTESIAN_POINT('Ctrl Pts',(-4.45431737341237,7.71399471716865,153.804715001966));
#71153=CARTESIAN_POINT('Ctrl Pts',(-8.14272862359425,1.65554281259527,154.069907883839));
#71154=CARTESIAN_POINT('Ctrl Pts',(-7.04798108604295,-3.4286320911007,154.2820759771));
#71155=CARTESIAN_POINT('Ctrl Pts',(-5.39382471105643,-5.40373945539631,
154.388166917611));
#71156=CARTESIAN_POINT('Ctrl Pts',(-4.37174242490101,-6.13237120108859,
154.441219281748));
#71157=CARTESIAN_POINT('Ctrl Pts',(-3.42297540299426,7.13846790764723,0.00329555398570502));
#71158=CARTESIAN_POINT('Ctrl Pts',(-4.61248760772119,6.56808466220277,0.0563367808326817));
#71159=CARTESIAN_POINT('Ctrl Pts',(-6.68124558086778,4.82084484305895,0.162416584054128));
#71160=CARTESIAN_POINT('Ctrl Pts',(-8.73125343145438,-0.246903062024332,
0.374573540024513));
#71161=CARTESIAN_POINT('Ctrl Pts',(-6.00338321156667,-7.18601493687386,
0.63976642189686));
#71162=CARTESIAN_POINT('Ctrl Pts',(2.81366832431631,-8.93427211377407,0.957997880143678));
#71163=CARTESIAN_POINT('Ctrl Pts',(9.03311162062166,-2.46519013156289,1.2762293383905));
#71164=CARTESIAN_POINT('Ctrl Pts',(6.95491649732933,6.27496220779387,1.59446079663731));
#71165=CARTESIAN_POINT('Ctrl Pts',(-0.100287973879036,8.7351568589752,1.85965367850966));
#71166=CARTESIAN_POINT('Ctrl Pts',(-5.06108046326141,6.48944842488126,2.07180798400754));
#71167=CARTESIAN_POINT('Ctrl Pts',(-8.44712147412926,2.22451783963094,2.28396228950542));
#71168=CARTESIAN_POINT('Ctrl Pts',(-7.78147446499357,-5.2150894756392,2.54915517137776));
#71169=CARTESIAN_POINT('Ctrl Pts',(0.192851584205466,-9.36462709367549,
2.86738662962458));
#71170=CARTESIAN_POINT('Ctrl Pts',(7.97527740293589,-4.89948280242022,3.1856180878714));
#71171=CARTESIAN_POINT('Ctrl Pts',(8.44062740491563,4.06086316790547,3.50384954611821));
#71172=CARTESIAN_POINT('Ctrl Pts',(1.13445937096465,9.29847198840014,3.82208100436503));
#71173=CARTESIAN_POINT('Ctrl Pts',(-5.80213362046967,6.5293858776913,4.08727388623738));
#71174=CARTESIAN_POINT('Ctrl Pts',(-8.07677783027992,1.58136138774822,4.29942819173525));
#71175=CARTESIAN_POINT('Ctrl Pts',(-7.83611087594979,-3.85912798670673,
4.51158249723313));
#71176=CARTESIAN_POINT('Ctrl Pts',(-2.45601594162407,-9.03973489175808,
4.77677537910549));
#71177=CARTESIAN_POINT('Ctrl Pts',(6.28595611954916,-6.94418193300223,5.09500683735229));
#71178=CARTESIAN_POINT('Ctrl Pts',(9.23407505830372,1.53000458735974,5.41323829559912));
#71179=CARTESIAN_POINT('Ctrl Pts',(3.7103425378918,8.600481415577,5.73146975384593));
#71180=CARTESIAN_POINT('Ctrl Pts',(-5.24033302554986,7.76451626770152,6.04970121209275));
#71181=CARTESIAN_POINT('Ctrl Pts',(-8.66202435946179,1.12553451626218,6.3148940939651));
#71182=CARTESIAN_POINT('Ctrl Pts',(-7.13512265001104,-4.10184231184789,
6.52704839946297));
#71183=CARTESIAN_POINT('Ctrl Pts',(-3.38615597408042,-8.05179736388011,
6.73920270496085));
#71184=CARTESIAN_POINT('Ctrl Pts',(4.07284419904651,-8.43568288398085,7.0043955868332));
#71185=CARTESIAN_POINT('Ctrl Pts',(9.29931124422426,-1.12148598127022,7.32262704508001));
#71186=CARTESIAN_POINT('Ctrl Pts',(5.96884097496818,7.20985368569242,7.64085850332684));
#71187=CARTESIAN_POINT('Ctrl Pts',(-2.83777377981589,8.92647525582364,7.95908996157364));
#71188=CARTESIAN_POINT('Ctrl Pts',(-9.04771061934406,2.42646614163091,8.27732141982047));
#71189=CARTESIAN_POINT('Ctrl Pts',(-7.27812150961367,-4.82974538791432,
8.54251430169281));
#71190=CARTESIAN_POINT('Ctrl Pts',(-2.69774408852947,-7.77542683556561,
8.7546686071907));
#71191=CARTESIAN_POINT('Ctrl Pts',(2.72278186451387,-8.29963566286574,8.96682291268856));
#71192=CARTESIAN_POINT('Ctrl Pts',(8.60629055567863,-3.69872522279475,9.23201579456092));
#71193=CARTESIAN_POINT('Ctrl Pts',(7.75664043211721,5.25066183436719,9.55024725280773));
#71194=CARTESIAN_POINT('Ctrl Pts',(-0.220716078597512,9.3573680688768,9.86847871105456));
#71195=CARTESIAN_POINT('Ctrl Pts',(-7.9955754646328,4.87910785714359,10.1867101693014));
#71196=CARTESIAN_POINT('Ctrl Pts',(-8.42232971392672,-4.10038627340938,
10.5049416275482));
#71197=CARTESIAN_POINT('Ctrl Pts',(-2.3284377171429,-8.41878085102033,10.7701345094205));
#71198=CARTESIAN_POINT('Ctrl Pts',(3.06134429193571,-7.63958485568192,10.9822888149184));
#71199=CARTESIAN_POINT('Ctrl Pts',(7.4977430927122,-4.48122100948196,11.1944431204163));
#71200=CARTESIAN_POINT('Ctrl Pts',(8.92324408893685,2.85035442191671,11.4596360022886));
#71201=CARTESIAN_POINT('Ctrl Pts',(2.41374714549149,9.05034503263406,11.7778674605355));
#71202=CARTESIAN_POINT('Ctrl Pts',(-6.30213737131939,6.92041308861664,12.0960989187823));
#71203=CARTESIAN_POINT('Ctrl Pts',(-9.23609288047689,-1.55868816486623,
12.4143303770291));
#71204=CARTESIAN_POINT('Ctrl Pts',(-3.67058418915988,-8.61833029719639,
12.7325618352759));
#71205=CARTESIAN_POINT('Ctrl Pts',(3.76202105532412,-7.88319039472274,12.9977547171482));
#71206=CARTESIAN_POINT('Ctrl Pts',(7.32058367569969,-3.76086961858448,13.2099090226462));
#71207=CARTESIAN_POINT('Ctrl Pts',(8.59932381098584,1.53268496892321,13.422063328144));
#71208=CARTESIAN_POINT('Ctrl Pts',(4.86841927299924,8.00295565298049,13.6872562100164));
#71209=CARTESIAN_POINT('Ctrl Pts',(-4.11171689749063,8.41597912586406,14.0054876682632));
#71210=CARTESIAN_POINT('Ctrl Pts',(-9.29594305705086,1.09292975261354,14.32371912651));
#71211=CARTESIAN_POINT('Ctrl Pts',(-5.95155746979874,-7.23283375833925,
14.6419505847568));
#71212=CARTESIAN_POINT('Ctrl Pts',(2.87949614829766,-8.91388284269106,14.9601820430037));
#71213=CARTESIAN_POINT('Ctrl Pts',(8.00934721423155,-3.485376654256,15.225374924876));
#71214=CARTESIAN_POINT('Ctrl Pts',(7.99323852829464,1.9604141069423,15.4375292303739));
#71215=CARTESIAN_POINT('Ctrl Pts',(5.48782492723469,6.79568030355847,15.6496835358718));
#71216=CARTESIAN_POINT('Ctrl Pts',(-1.57159749337621,9.2346568274136,15.9148764177441));
#71217=CARTESIAN_POINT('Ctrl Pts',(-8.62272131889369,3.65835995341979,16.2331078759909));
#71218=CARTESIAN_POINT('Ctrl Pts',(-7.7353734295505,-5.27001429499806,16.5513393342377));
#71219=CARTESIAN_POINT('Ctrl Pts',(0.248833411311902,-9.36338626916054,
16.8695707924846));
#71220=CARTESIAN_POINT('Ctrl Pts',(8.01882062248585,-4.84224340834686,17.1878022507313));
#71221=CARTESIAN_POINT('Ctrl Pts',(8.33264188932629,2.62003289376223,17.4529951326037));
#71222=CARTESIAN_POINT('Ctrl Pts',(4.74975404971919,6.72122921109588,17.6651494381016));
#71223=CARTESIAN_POINT('Ctrl Pts',(-0.312332247401522,8.72925780277937,
17.8773037435995));
#71224=CARTESIAN_POINT('Ctrl Pts',(-7.24163914455982,5.94200874294728,18.1424966254718));
#71225=CARTESIAN_POINT('Ctrl Pts',(-8.90918296215872,-2.89160499357533,
18.4607280837186));
#71226=CARTESIAN_POINT('Ctrl Pts',(-2.3850007051549,-9.05101234119646,18.7789595419654));
#71227=CARTESIAN_POINT('Ctrl Pts',(6.32731296630629,-6.906520912768,19.0971910002123));
#71228=CARTESIAN_POINT('Ctrl Pts',(9.22947229175811,1.6017635958381,19.4154224584591));
#71229=CARTESIAN_POINT('Ctrl Pts',(4.57351283593627,7.4418057996482,19.6806153403314));
#71230=CARTESIAN_POINT('Ctrl Pts',(-0.820784548616145,8.18910241514082,
19.8927696458293));
#71231=CARTESIAN_POINT('Ctrl Pts',(-5.95946801599405,6.38609694465212,20.1049239513272));
#71232=CARTESIAN_POINT('Ctrl Pts',(-9.36377367702461,-0.26181658989513,
20.3701168331995));
#71233=CARTESIAN_POINT('Ctrl Pts',(-4.83075524509748,-8.02488157258739,
20.6883482914463));
#71234=CARTESIAN_POINT('Ctrl Pts',(4.13385898897949,-8.3976343468451,21.0065797496932));
#71235=CARTESIAN_POINT('Ctrl Pts',(9.30584259734126,-1.06593341518065,21.32481120794));
#71236=CARTESIAN_POINT('Ctrl Pts',(5.91831476945442,7.26101616104393,21.6430426661868));
#71237=CARTESIAN_POINT('Ctrl Pts',(-1.42632421522254,8.61760363750972,21.9082355480591));
#71238=CARTESIAN_POINT('Ctrl Pts',(-5.98919494298574,5.64487640040296,22.120389853557));
#71239=CARTESIAN_POINT('Ctrl Pts',(-8.68687268840156,0.914186039958304,
22.3325441590549));
#71240=CARTESIAN_POINT('Ctrl Pts',(-6.89830053896013,-6.33736972848087,
22.5977370409273));
#71241=CARTESIAN_POINT('Ctrl Pts',(1.61441162876708,-9.226515896317,22.915968499174));
#71242=CARTESIAN_POINT('Ctrl Pts',(8.62741095346841,-3.62999077189642,23.2341999574209));
#71243=CARTESIAN_POINT('Ctrl Pts',(7.72514681853416,5.29688843795875,23.5524314156677));
#71244=CARTESIAN_POINT('Ctrl Pts',(-0.292411577283184,9.36286819680556,
23.8706628739145));
#71245=CARTESIAN_POINT('Ctrl Pts',(-6.72736010606789,5.57136601054333,24.1358557557869));
#71246=CARTESIAN_POINT('Ctrl Pts',(-8.22331008327924,0.335047631166753,
24.3480100612847));
#71247=CARTESIAN_POINT('Ctrl Pts',(-7.15830480606812,-5.00561340132991,
24.5601643667826));
#71248=CARTESIAN_POINT('Ctrl Pts',(-1.05313267975989,-9.30804581854349,
24.825357248655));
#71249=CARTESIAN_POINT('Ctrl Pts',(7.26862739392478,-5.90778945971974,25.1435887069018));
#71250=CARTESIAN_POINT('Ctrl Pts',(8.89412254012404,2.91609962198425,25.4618201651486));
#71251=CARTESIAN_POINT('Ctrl Pts',(2.35965828169305,9.06459780054951,25.7800516233954));
#71252=CARTESIAN_POINT('Ctrl Pts',(-6.35987628174224,6.87755618531872,26.0982830816422));
#71253=CARTESIAN_POINT('Ctrl Pts',(-8.73245037824297,-0.20445931545182,
26.3634759635146));
#71254=CARTESIAN_POINT('Ctrl Pts',(-6.42856659067376,-5.13893152612344,
26.5756302690125));
#71255=CARTESIAN_POINT('Ctrl Pts',(-2.12265792236143,-8.47300516728202,
26.7877845745103));
#71256=CARTESIAN_POINT('Ctrl Pts',(5.30799805150393,-7.71841707129861,27.0529774563827));
#71257=CARTESIAN_POINT('Ctrl Pts',(9.36171364690645,0.30534912053947,27.3712089146295));
#71258=CARTESIAN_POINT('Ctrl Pts',(4.80332334159109,8.03350095787672,27.6894403728763));
#71259=CARTESIAN_POINT('Ctrl Pts',(-4.16190117338093,8.39127517812996,28.0076718311231));
#71260=CARTESIAN_POINT('Ctrl Pts',(-9.31143726830945,1.02271276496403,28.3259032893699));
#71261=CARTESIAN_POINT('Ctrl Pts',(-6.45923814978851,-5.88011358261622,
28.5910961712423));
#71262=CARTESIAN_POINT('Ctrl Pts',(-1.48426583417955,-8.09518625940132,
28.8032504767402));
#71263=CARTESIAN_POINT('Ctrl Pts',(3.95294593835214,-7.78920481362613,29.0154047822381));
#71264=CARTESIAN_POINT('Ctrl Pts',(9.06857334260554,-2.34729268116836,29.2805976641104));
#71265=CARTESIAN_POINT('Ctrl Pts',(6.86820150300202,6.36888754856376,29.5988291223572));
#71266=CARTESIAN_POINT('Ctrl Pts',(-1.64077526014977,9.21503713013466,29.917060580604));
#71267=CARTESIAN_POINT('Ctrl Pts',(-8.64441414938049,3.60680253217169,30.2352920388509));
#71268=CARTESIAN_POINT('Ctrl Pts',(-7.70103183950281,-5.33318985300987,
30.5535234970977));
#71269=CARTESIAN_POINT('Ctrl Pts',(-1.02144169452243,-8.67491499006428,
30.81871637897));
#71270=CARTESIAN_POINT('Ctrl Pts',(4.18722350683741,-7.08535425682446,31.0308706844679));
#71271=CARTESIAN_POINT('Ctrl Pts',(8.09187707143799,-3.28922767240087,31.2430249899657));
#71272=CARTESIAN_POINT('Ctrl Pts',(8.38616890541952,4.17384432999819,31.5082178718381));
#71273=CARTESIAN_POINT('Ctrl Pts',(1.00974110375637,9.31210735523779,31.8264493300849));
#71274=CARTESIAN_POINT('Ctrl Pts',(-7.28100637975073,5.88183635118395,32.1446807883317));
#71275=CARTESIAN_POINT('Ctrl Pts',(-8.89175634629185,-2.94475628367924,
32.4629122465786));
#71276=CARTESIAN_POINT('Ctrl Pts',(-2.31764834047869,-9.07619477375616,
32.7811437048254));
#71277=CARTESIAN_POINT('Ctrl Pts',(4.91679122091634,-7.21960229583813,33.0463365866977));
#71278=CARTESIAN_POINT('Ctrl Pts',(7.80726016000046,-2.60418402479207,33.2584908921956));
#71279=CARTESIAN_POINT('Ctrl Pts',(8.26634274408729,2.82224571173855,33.4706451976935));
#71280=CARTESIAN_POINT('Ctrl Pts',(3.59511616853625,8.65008353347016,33.7358380795658));
#71281=CARTESIAN_POINT('Ctrl Pts',(-5.34342326769297,7.69303244984494,34.0540695378126));
#71282=CARTESIAN_POINT('Ctrl Pts',(-9.35404313209839,-0.333061326069361,
34.3723009960595));
#71283=CARTESIAN_POINT('Ctrl Pts',(-4.78274703090486,-8.05358624033165,
34.6905324543063));
#71284=CARTESIAN_POINT('Ctrl Pts',(4.20122408332126,-8.37248598702948,35.008763912553));
#71285=CARTESIAN_POINT('Ctrl Pts',(8.4461332449818,-2.22717902921267,35.2739567944255));
#71286=CARTESIAN_POINT('Ctrl Pts',(7.60227414268639,3.15285798924627,35.4861110999233));
#71287=CARTESIAN_POINT('Ctrl Pts',(4.39086672783747,7.55101202478985,35.6982654054212));
#71288=CARTESIAN_POINT('Ctrl Pts',(-2.95729722059006,8.88837434801064,35.9634582872935));
#71289=CARTESIAN_POINT('Ctrl Pts',(-9.07867626972295,2.30489862719791,36.2816897455404));
#71290=CARTESIAN_POINT('Ctrl Pts',(-6.84423951437506,-6.38478176870181,
36.5999212037871));
#71291=CARTESIAN_POINT('Ctrl Pts',(1.66948070495901,-9.21671062081584,36.9181526620341));
#71292=CARTESIAN_POINT('Ctrl Pts',(8.66178449584876,-3.56683259331808,37.2363841202807));
#71293=CARTESIAN_POINT('Ctrl Pts',(7.83744855060318,3.85640939693899,37.5015770021533));
#71294=CARTESIAN_POINT('Ctrl Pts',(3.6726945615586,7.36521556360778,37.713731307651));
#71295=CARTESIAN_POINT('Ctrl Pts',(-1.6358332047192,8.5802997002721,37.925885613149));
#71296=CARTESIAN_POINT('Ctrl Pts',(-8.06083755050287,4.77197059773897,38.1910784950212));
#71297=CARTESIAN_POINT('Ctrl Pts',(-8.36599980124193,-4.21247763409013,
38.5093099532681));
#71298=CARTESIAN_POINT('Ctrl Pts',(-0.981227374309102,-9.30839651089201,
38.8275414115149));
#71299=CARTESIAN_POINT('Ctrl Pts',(7.30377725708829,-5.86427815429389,39.1457728697617));
#71300=CARTESIAN_POINT('Ctrl Pts',(8.87866384941099,2.98632443824268,39.4640043280085));
#71301=CARTESIAN_POINT('Ctrl Pts',(3.38895094229788,8.05062138787126,39.7291972098809));
#71302=CARTESIAN_POINT('Ctrl Pts',(-2.05625377016801,7.96912203906943,39.9413515153788));
#71303=CARTESIAN_POINT('Ctrl Pts',(-6.86108692375931,5.4058282848024,40.1535058208766));
#71304=CARTESIAN_POINT('Ctrl Pts',(-9.21511965898805,-1.68237185895847,
40.418698702749));
#71305=CARTESIAN_POINT('Ctrl Pts',(-3.5545565124997,-8.66602841511239,40.7369301609958));
#71306=CARTESIAN_POINT('Ctrl Pts',(5.36251896376071,-7.67153460054681,41.0551616192426));
#71307=CARTESIAN_POINT('Ctrl Pts',(9.35972327190498,0.361248896814873,41.3733930774894));
#71308=CARTESIAN_POINT('Ctrl Pts',(4.74560611729256,8.07638706234402,41.6916245357363));
#71309=CARTESIAN_POINT('Ctrl Pts',(-2.71990047999163,8.30058037724426,41.9568174176086));
#71310=CARTESIAN_POINT('Ctrl Pts',(-6.77777861068786,4.66870461106876,42.1689717231065));
#71311=CARTESIAN_POINT('Ctrl Pts',(-8.724878043929,-0.417128683641938,42.3811260286043));
#71312=CARTESIAN_POINT('Ctrl Pts',(-5.85462438277968,-7.31246734952329,
42.6463189104767));
#71313=CARTESIAN_POINT('Ctrl Pts',(2.99837597541927,-8.87381890744443,42.9645503687235));
#71314=CARTESIAN_POINT('Ctrl Pts',(9.07899834941898,-2.27614624647169,43.2827818269704));
#71315=CARTESIAN_POINT('Ctrl Pts',(6.83004603724268,6.40978873452435,43.6010132852171));
#71316=CARTESIAN_POINT('Ctrl Pts',(-1.71247353183573,9.2095732693782,43.919244743464));
#71317=CARTESIAN_POINT('Ctrl Pts',(-7.49618698396174,4.48382358279551,44.1844376253363));
#71318=CARTESIAN_POINT('Ctrl Pts',(-8.17865621900968,-0.919058263749683,
44.3965919308342));
#71319=CARTESIAN_POINT('Ctrl Pts',(-6.31407658856778,-6.03572117098297,
44.6087462363321));
#71320=CARTESIAN_POINT('Ctrl Pts',(0.374235791270018,-9.35995475276541,
44.8739391182044));
#71321=CARTESIAN_POINT('Ctrl Pts',(8.08230962820882,-4.73404600377431,45.1921705764512));
#71322=CARTESIAN_POINT('Ctrl Pts',(8.34739046757811,4.23439784926572,45.510402034698));
#71323=CARTESIAN_POINT('Ctrl Pts',(0.954114111760157,9.31797117154962,45.8286334929449));
#71324=CARTESIAN_POINT('Ctrl Pts',(-7.33155845712685,5.83069944269244,46.1468649511917));
#71325=CARTESIAN_POINT('Ctrl Pts',(-8.59985536477875,-1.52969961921854,
46.412057833064));
#71326=CARTESIAN_POINT('Ctrl Pts',(-5.5725525290743,-6.05654554606999,46.624212138562));
#71327=CARTESIAN_POINT('Ctrl Pts',(-0.809810127629026,-8.69722373963903,
46.8363664440597));
#71328=CARTESIAN_POINT('Ctrl Pts',(6.41974606325721,-6.8217054967637,47.1015593259322));
#71329=CARTESIAN_POINT('Ctrl Pts',(9.20646521236131,1.72508515316507,47.4197907841789));
#71330=CARTESIAN_POINT('Ctrl Pts',(3.52613306420666,8.67037706086584,47.7380222424258));
#71331=CARTESIAN_POINT('Ctrl Pts',(-5.38926837037244,7.66098602819454,48.0562537006726));
#71332=CARTESIAN_POINT('Ctrl Pts',(-9.35868196013644,-0.404817700082644,
48.3744851589195));
#71333=CARTESIAN_POINT('Ctrl Pts',(-5.49018371862514,-6.79377479431687,
48.6396780407917));
#71334=CARTESIAN_POINT('Ctrl Pts',(-0.236279827308163,-8.22674039241056,
48.8518323462897));
#71335=CARTESIAN_POINT('Ctrl Pts',(5.09120782275439,-7.09768244750886,49.0639866517874));
#71336=CARTESIAN_POINT('Ctrl Pts',(9.32002052557175,-0.941287843438186,
49.3291795336599));
#71337=CARTESIAN_POINT('Ctrl Pts',(5.82008349782607,7.33904275572924,49.6474109919066));
#71338=CARTESIAN_POINT('Ctrl Pts',(-3.02268799572273,8.85846544524466,49.9656424501536));
#71339=CARTESIAN_POINT('Ctrl Pts',(-9.09227852322461,2.25064251897061,50.2838739084002));
#71340=CARTESIAN_POINT('Ctrl Pts',(-6.80069238510234,-6.44200190037953,
50.6021053666473));
#71341=CARTESIAN_POINT('Ctrl Pts',(0.309301864614412,-8.72936570299912,
50.8672982485194));
#71342=CARTESIAN_POINT('Ctrl Pts',(5.21575380434986,-6.36639598935869,51.0794525540174));
#71343=CARTESIAN_POINT('Ctrl Pts',(8.49788269463788,-2.02076295698556,51.2916068595152));
#71344=CARTESIAN_POINT('Ctrl Pts',(7.65412336441857,5.40029637367655,51.5567997413876));
#71345=CARTESIAN_POINT('Ctrl Pts',(-0.417740447020749,9.35737214238125,
51.8750311996344));
#71346=CARTESIAN_POINT('Ctrl Pts',(-8.09059899598044,4.7065125783663,52.1932626578812));
#71347=CARTESIAN_POINT('Ctrl Pts',(-8.34069503312267,-4.26236165247995,
52.511494116128));
#71348=CARTESIAN_POINT('Ctrl Pts',(-0.910829398031864,-9.32304645536878,
52.8297255743748));
#71349=CARTESIAN_POINT('Ctrl Pts',(5.95725072179067,-6.38816539061693,53.0949184562473));
#71350=CARTESIAN_POINT('Ctrl Pts',(8.11242535809501,-1.38695365829185,53.307072761745));
#71351=CARTESIAN_POINT('Ctrl Pts',(7.74117716265346,4.0461919574538,53.5192270672431));
#71352=CARTESIAN_POINT('Ctrl Pts',(2.23823007254506,9.09610529532493,53.7844199491152));
#71353=CARTESIAN_POINT('Ctrl Pts',(-6.45090018861527,6.79123017196538,54.1026514073622));
#71354=CARTESIAN_POINT('Ctrl Pts',(-9.1946707052259,-1.75130904940847,54.4208828656089));
#71355=CARTESIAN_POINT('Ctrl Pts',(-3.50274232572709,-8.68710059177684,
54.7391143238558));
#71356=CARTESIAN_POINT('Ctrl Pts',(5.42527760102361,-7.63643688857014,55.0573457821025));
#71357=CARTESIAN_POINT('Ctrl Pts',(8.68655480505386,-0.917201634836717,
55.322538663975));
#71358=CARTESIAN_POINT('Ctrl Pts',(7.03456419852726,4.27200095712899,55.5346929694727));
#71359=CARTESIAN_POINT('Ctrl Pts',(3.19182510211682,8.13078998238474,55.7468472749707));
#71360=CARTESIAN_POINT('Ctrl Pts',(-4.27424263307616,8.33544571782919,56.0120401568429));
#71361=CARTESIAN_POINT('Ctrl Pts',(-9.32356073321153,0.897850625775644,
56.3302716150898));
#71362=CARTESIAN_POINT('Ctrl Pts',(-5.79398361634028,-7.35110921002132,
56.6485030733367));
#71363=CARTESIAN_POINT('Ctrl Pts',(3.05131417866885,-8.85575531929058,56.9667345315834));
#71364=CARTESIAN_POINT('Ctrl Pts',(9.1033702144607,-2.20849635266917,57.2849659898303));
#71365=CARTESIAN_POINT('Ctrl Pts',(7.16004207464101,5.00312809245597,57.5501588717026));
#71366=CARTESIAN_POINT('Ctrl Pts',(2.51024845888154,7.83796774142348,57.7623131772005));
#71367=CARTESIAN_POINT('Ctrl Pts',(-2.92130261410299,8.23185788610236,57.9744674826984));
#71368=CARTESIAN_POINT('Ctrl Pts',(-8.69262923991475,3.49098872794833,58.2396603645707));
#71369=CARTESIAN_POINT('Ctrl Pts',(-7.62831519510564,-5.43541422305696,
58.5578918228176));
#71370=CARTESIAN_POINT('Ctrl Pts',(0.44535854880617,-9.34936941868726,58.8761232810643));
#71371=CARTESIAN_POINT('Ctrl Pts',(8.11043575468189,-4.68569657161741,59.1943547393112));
#71372=CARTESIAN_POINT('Ctrl Pts',(8.321435016034,4.30145611104038,59.5125861975579));
#71373=CARTESIAN_POINT('Ctrl Pts',(2.12559920025952,8.47226777551363,59.7777790794304));
#71374=CARTESIAN_POINT('Ctrl Pts',(-3.24391707018758,7.56386724385468,59.9899333849281));
#71375=CARTESIAN_POINT('Ctrl Pts',(-7.60319216260854,4.29987931907398,60.2020876904262));
#71376=CARTESIAN_POINT('Ctrl Pts',(-8.85222297610258,-3.06381360115863,
60.4672805722983));
#71377=CARTESIAN_POINT('Ctrl Pts',(-2.19571776134802,-9.10569843584722,
60.7855120305454));
#71378=CARTESIAN_POINT('Ctrl Pts',(6.46650553270306,-6.76707905669801,61.103743488792));
#71379=CARTESIAN_POINT('Ctrl Pts',(9.19599938676387,1.78003251957012,61.421974947039));
#71380=CARTESIAN_POINT('Ctrl Pts',(3.46256668934964,8.7039897359251,61.7402064052856));
#71381=CARTESIAN_POINT('Ctrl Pts',(-3.95024167581746,7.79057661041764,62.0053992871582));
#71382=CARTESIAN_POINT('Ctrl Pts',(-7.40878544758956,3.58398993197489,62.2175535926559));
#71383=CARTESIAN_POINT('Ctrl Pts',(-8.56003838042413,-1.73874556672825,
62.4297078981539));
#71384=CARTESIAN_POINT('Ctrl Pts',(-4.67483384329524,-8.11755714109021,
62.6949007800261));
#71385=CARTESIAN_POINT('Ctrl Pts',(4.3126309658217,-8.31481416778063,63.0131322382731));
#71386=CARTESIAN_POINT('Ctrl Pts',(9.31950776998579,-0.869383511031748,
63.3313636965197));
#71387=CARTESIAN_POINT('Ctrl Pts',(5.7761532577777,7.37366761081306,63.6495951547667));
#71388=CARTESIAN_POINT('Ctrl Pts',(-3.09272212459566,8.84216462532336,63.9678266130134));
#71389=CARTESIAN_POINT('Ctrl Pts',(-8.09073472766302,3.29203657129424,64.2330194948858));
#71390=CARTESIAN_POINT('Ctrl Pts',(-7.94385646753675,-2.15179693839514,
64.4451738003837));
#71391=CARTESIAN_POINT('Ctrl Pts',(-5.32305216608538,-6.92550423126613,
64.6573281058815));
#71392=CARTESIAN_POINT('Ctrl Pts',(1.79290364026012,-9.19425374557529,64.9225209877539));
#71393=CARTESIAN_POINT('Ctrl Pts',(8.70808594081639,-3.45024053356348,65.2407524460007));
#71394=CARTESIAN_POINT('Ctrl Pts',(7.60658959891365,5.4542504010889,65.5589839042475));
#71395=CARTESIAN_POINT('Ctrl Pts',(-0.473612293177449,9.35471067900242,
65.8772153624943));
#71396=CARTESIAN_POINT('Ctrl Pts',(-8.13278895315451,4.64828454859746,66.1954468207411));
#71397=CARTESIAN_POINT('Ctrl Pts',(-8.2673219892696,-2.81937587878726,66.4606397026135));
#71398=CARTESIAN_POINT('Ctrl Pts',(-4.58698198334685,-6.83335070996431,
66.6727940081113));
#71399=CARTESIAN_POINT('Ctrl Pts',(0.521864973333528,-8.71924022892736,
66.8849483136093));
#71400=CARTESIAN_POINT('Ctrl Pts',(7.38224115642129,-5.76639583359743,67.1501411954815));
#71401=CARTESIAN_POINT('Ctrl Pts',(8.83717532052503,3.10471461594072,67.4683726537285));
#71402=CARTESIAN_POINT('Ctrl Pts',(2.16696358608828,9.10567524023015,67.7866041119752));
#71403=CARTESIAN_POINT('Ctrl Pts',(-6.49134026355597,6.75258632487546,68.1048355702222));
#71404=CARTESIAN_POINT('Ctrl Pts',(-9.18834630176509,-1.82293654315669,
68.4230670284687));
#71405=CARTESIAN_POINT('Ctrl Pts',(-4.39348779890017,-7.54948727930569,
68.6882599103413));
#71406=CARTESIAN_POINT('Ctrl Pts',(1.01719945816525,-8.16703072749937,68.9004142158391));
#71407=CARTESIAN_POINT('Ctrl Pts',(6.11110402433387,-6.24114579410071,69.112568521337));
#71408=CARTESIAN_POINT('Ctrl Pts',(9.35478619936243,0.486601030664479,69.3777614032093));
#71409=CARTESIAN_POINT('Ctrl Pts',(4.63665415188428,8.13857228119282,69.6959928614562));
#71410=CARTESIAN_POINT('Ctrl Pts',(-4.33432614433332,8.29594296206201,70.0142243197029));
#71411=CARTESIAN_POINT('Ctrl Pts',(-9.32875616973107,0.842157234248181,
70.3324557779499));
#71412=CARTESIAN_POINT('Ctrl Pts',(-5.74224337806769,-7.40104360508217,
70.6506872361965));
#71413=CARTESIAN_POINT('Ctrl Pts',(1.63285445542184,-8.58086705839598,70.915880118069));
#71414=CARTESIAN_POINT('Ctrl Pts',(6.12302284155387,-5.49942514752871,71.1280344235668));
#71415=CARTESIAN_POINT('Ctrl Pts',(8.70632073004518,-0.70531743185354,71.3401887290648));
#71416=CARTESIAN_POINT('Ctrl Pts',(6.7441268038012,6.50119669029752,71.605381610937));
#71417=CARTESIAN_POINT('Ctrl Pts',(-1.83550990659903,9.18508708634037,71.9236130691839));
#71418=CARTESIAN_POINT('Ctrl Pts',(-8.71209302149546,3.42176681632458,72.2418445274307));
#71419=CARTESIAN_POINT('Ctrl Pts',(-7.59572049010687,-5.48087102386278,
72.5600759856775));
#71420=CARTESIAN_POINT('Ctrl Pts',(0.517165260720624,-9.35314665584888,
72.8783074439244));
#71421=CARTESIAN_POINT('Ctrl Pts',(6.85921020902198,-5.40820912682017,73.1435003257966));
#71422=CARTESIAN_POINT('Ctrl Pts',(8.22898402782439,-0.137478835253676,
73.3556546312946));
#71423=CARTESIAN_POINT('Ctrl Pts',(7.03603774439987,5.17607027954607,73.5678089367924));
#71424=CARTESIAN_POINT('Ctrl Pts',(0.829304980625463,9.3306468046128,73.8330018186647));
#71425=CARTESIAN_POINT('Ctrl Pts',(-7.4083960272372,5.73154597449478,74.1512332769116));
#71426=CARTESIAN_POINT('Ctrl Pts',(-8.82153809043052,-3.1288545050304,74.4694647351584));
#71427=CARTESIAN_POINT('Ctrl Pts',(-2.14128887058924,-9.11862174517115,
74.7876961934052));
#71428=CARTESIAN_POINT('Ctrl Pts',(6.52317212309447,-6.72290049963323,75.105927651652));
#71429=CARTESIAN_POINT('Ctrl Pts',(8.72506864642096,0.41419157696923,75.3711205335244));
#71430=CARTESIAN_POINT('Ctrl Pts',(6.30324556561973,5.29170151049384,75.5832748390223));
#71431=CARTESIAN_POINT('Ctrl Pts',(1.91872716925317,8.52183314014436,75.7954291445202));
#71432=CARTESIAN_POINT('Ctrl Pts',(-5.49213569966153,7.58809272686213,76.0606220263924));
#71433=CARTESIAN_POINT('Ctrl Pts',(-9.351145146202,-0.529009343018155,76.3788534846394));
#71434=CARTESIAN_POINT('Ctrl Pts',(-4.61000204878283,-8.1484690439886,76.6970849428861));
#71435=CARTESIAN_POINT('Ctrl Pts',(4.36404740560219,-8.28527156301856,77.0153164011329));
#71436=CARTESIAN_POINT('Ctrl Pts',(9.32976675590779,-0.805805192827627,
77.3335478593798));
#71437=CARTESIAN_POINT('Ctrl Pts',(5.72000965224047,7.41431886349542,77.6517793176265));
#71438=CARTESIAN_POINT('Ctrl Pts',(-3.14460068207903,8.81822846159531,77.9700107758735));
#71439=CARTESIAN_POINT('Ctrl Pts',(-9.12196189467311,2.12451820949349,78.2882422341201));
#71440=CARTESIAN_POINT('Ctrl Pts',(-6.71185432316634,-6.53404295360445,
78.6064736923671));
#71441=CARTESIAN_POINT('Ctrl Pts',(0.429163617750448,-8.72461876575088,
78.8716665742392));
#71442=CARTESIAN_POINT('Ctrl Pts',(5.30258923183553,-6.29408905045752,79.0838208797373));
#71443=CARTESIAN_POINT('Ctrl Pts',(8.52484345756404,-1.90405398327316,79.2959751852351));
#71444=CARTESIAN_POINT('Ctrl Pts',(7.57927685282243,5.50488220253219,79.5611680671074));
#71445=CARTESIAN_POINT('Ctrl Pts',(-0.546104350604037,9.35072994995942,
79.8793995253544));
#71446=CARTESIAN_POINT('Ctrl Pts',(-8.15442949307008,4.59505652164535,80.197630983601));
#71447=CARTESIAN_POINT('Ctrl Pts',(-8.28141444936442,-4.37642841504223,
80.515862441848));
#71448=CARTESIAN_POINT('Ctrl Pts',(-0.782804302232367,-9.33466303450356,
80.8340939000947));
#71449=CARTESIAN_POINT('Ctrl Pts',(6.04435568800383,-6.30581438010313,81.0992867819672));
#71450=CARTESIAN_POINT('Ctrl Pts',(8.13069441932884,-1.27549473531918,81.3114410874649));
#71451=CARTESIAN_POINT('Ctrl Pts',(7.68492225173183,4.15204294725026,81.5235953929629));
#71452=CARTESIAN_POINT('Ctrl Pts',(2.11319270213992,9.12596454498564,81.7887882748351));
#71453=CARTESIAN_POINT('Ctrl Pts',(-6.54348919449422,6.70206431672992,82.1070197330821));
#71454=CARTESIAN_POINT('Ctrl Pts',(-9.16977157964343,-1.877323130858,82.4252511913288));
#71455=CARTESIAN_POINT('Ctrl Pts',(-3.38319878665011,-8.73435099883718,
82.7434826495756));
#71456=CARTESIAN_POINT('Ctrl Pts',(5.52956206707782,-7.56126630254611,83.0617141078225));
#71457=CARTESIAN_POINT('Ctrl Pts',(8.69832365568315,-0.797909089480057,
83.3269069896948));
#71458=CARTESIAN_POINT('Ctrl Pts',(6.9752768165914,4.36813449923239,83.5390612951928));
#71459=CARTESIAN_POINT('Ctrl Pts',(3.0799451492746,8.17382597220634,83.7512156006905));
#71460=CARTESIAN_POINT('Ctrl Pts',(-4.38822804532377,8.27600507971838,84.0164084825631));
#71461=CARTESIAN_POINT('Ctrl Pts',(-9.33500403898603,0.769818208155055,
84.3346399408096));
#71462=CARTESIAN_POINT('Ctrl Pts',(-5.69255824119631,-7.42992822480975,
84.6528713990567));
#71463=CARTESIAN_POINT('Ctrl Pts',(3.17255499281213,-8.81304801518571,84.9711028573032));
#71464=CARTESIAN_POINT('Ctrl Pts',(9.1328203370509,-2.08336220806071,85.2893343155504));
#71465=CARTESIAN_POINT('Ctrl Pts',(7.09070957079878,5.10091472208982,85.5545271974224));
#71466=CARTESIAN_POINT('Ctrl Pts',(2.40245110553475,7.87167798675258,85.7666815029205));
#71467=CARTESIAN_POINT('Ctrl Pts',(-3.03399388307664,8.19099348900591,85.9788358084183));
#71468=CARTESIAN_POINT('Ctrl Pts',(-8.73971777196734,3.37137044358746,86.2440286902905));
#71469=CARTESIAN_POINT('Ctrl Pts',(-7.55300630343952,-5.53958629072243,
86.5622601485375));
#71470=CARTESIAN_POINT('Ctrl Pts',(0.573618655037129,-9.3423773421205,86.8804916067843));
#71471=CARTESIAN_POINT('Ctrl Pts',(8.17397416785781,-4.57395526818167,87.1987230650311));
#71472=CARTESIAN_POINT('Ctrl Pts',(8.26162224189486,4.41524668999585,87.5169545232779));
#71473=CARTESIAN_POINT('Ctrl Pts',(2.00913352443477,8.50063972305202,87.7821474051502));
#71474=CARTESIAN_POINT('Ctrl Pts',(-3.34741107811517,7.51863848811937,87.9943017106483));
#71475=CARTESIAN_POINT('Ctrl Pts',(-7.66148374389044,4.19513528533351,88.2064560161458));
#71476=CARTESIAN_POINT('Ctrl Pts',(-8.80934447375909,-3.18500476356538,
88.4716488980186));
#71477=CARTESIAN_POINT('Ctrl Pts',(-2.07055286995459,-9.1349729777823,88.789880356265));
#71478=CARTESIAN_POINT('Ctrl Pts',(6.55876170372602,-6.67770152655952,89.1081118145122));
#71479=CARTESIAN_POINT('Ctrl Pts',(9.17070592911142,1.90606223766466,89.4263432727587));
#71480=CARTESIAN_POINT('Ctrl Pts',(3.342795180477,8.75068716059845,89.7445747310057));
#71481=CARTESIAN_POINT('Ctrl Pts',(-4.05678032049151,7.73563356496568,90.0097676128779));
#71482=CARTESIAN_POINT('Ctrl Pts',(-7.45727113570789,3.48198116730271,90.2219219183759));
#71483=CARTESIAN_POINT('Ctrl Pts',(-8.53537139222743,-1.85605183572463,
90.4340762238736));
#71484=CARTESIAN_POINT('Ctrl Pts',(-4.56299583547458,-8.18094581370174,
90.6992691057461));
#71485=CARTESIAN_POINT('Ctrl Pts',(4.42632963412773,-8.25484866379338,91.0175005639929));
#71486=CARTESIAN_POINT('Ctrl Pts',(9.33056080167088,-0.741409394601718,
91.3357320222397));
#71487=CARTESIAN_POINT('Ctrl Pts',(5.67441999091111,7.45223981490379,91.6539634804866));
#71488=CARTESIAN_POINT('Ctrl Pts',(-3.21377253336565,8.79889035646353,91.9721949387333));
#71489=CARTESIAN_POINT('Ctrl Pts',(-8.13514970333771,3.18069686144963,92.2373878206056));
#71490=CARTESIAN_POINT('Ctrl Pts',(-7.91357917000356,-2.26060840505348,
92.4495421261036));
#71491=CARTESIAN_POINT('Ctrl Pts',(-5.22751174290429,-6.99790069934896,
92.6616964316014));
#71492=CARTESIAN_POINT('Ctrl Pts',(1.91890819078105,-9.16878382102207,92.9268893134739));
#71493=CARTESIAN_POINT('Ctrl Pts',(8.7546138270785,-3.33041397288932,93.2451207717205));
#71494=CARTESIAN_POINT('Ctrl Pts',(7.5310242628826,5.55812255316062,93.5633522299674));
#71495=CARTESIAN_POINT('Ctrl Pts',(-0.60194303736029,9.34733037138744,93.8815836882144));
#71496=CARTESIAN_POINT('Ctrl Pts',(-8.19581185364207,4.53624001359984,94.199815146461));
#71497=CARTESIAN_POINT('Ctrl Pts',(-8.2278530003507,-2.93256342212263,94.4650080283335));
#71498=CARTESIAN_POINT('Ctrl Pts',(-4.49277550191721,-6.89565471367907,
94.6771623338312));
#71499=CARTESIAN_POINT('Ctrl Pts',(0.641470568788609,-8.7112575859935,94.8893166393294));
#71500=CARTESIAN_POINT('Ctrl Pts',(7.46067865137102,-5.66454583018452,95.1545095212014));
#71501=CARTESIAN_POINT('Ctrl Pts',(8.79373694769651,3.22569542685074,95.4727409794484));
#71502=CARTESIAN_POINT('Ctrl Pts',(2.04180172067109,9.13455518881701,95.7909724376951));
#71503=CARTESIAN_POINT('Ctrl Pts',(-6.58339521124076,6.66286935071541,96.109203895942));
#71504=CARTESIAN_POINT('Ctrl Pts',(-9.1624647898756,-1.94885719732676,96.4274353541887));
#71505=CARTESIAN_POINT('Ctrl Pts',(-4.28947194629567,-7.60906851343142,
96.6926282360612));
#71506=CARTESIAN_POINT('Ctrl Pts',(1.12918040088547,-8.15230257431412,96.904782541559));
#71507=CARTESIAN_POINT('Ctrl Pts',(6.19617624338033,-6.15669498847559,97.1169368470568));
#71508=CARTESIAN_POINT('Ctrl Pts',(9.34722763940825,0.614931588361719,97.3821297289294));
#71509=CARTESIAN_POINT('Ctrl Pts',(4.52453134686614,8.20143503195108,97.700361187176));
#71510=CARTESIAN_POINT('Ctrl Pts',(-4.44776379847873,8.23568151138829,98.0185926454229));
#71511=CARTESIAN_POINT('Ctrl Pts',(-9.33943470312532,0.714058763791374,
98.3368241036697));
#71512=CARTESIAN_POINT('Ctrl Pts',(-5.64013762035087,-7.47914788092769,
98.6550555619165));
#71513=CARTESIAN_POINT('Ctrl Pts',(1.75045652679066,-8.55765126468515,98.9202484437888));
#71514=CARTESIAN_POINT('Ctrl Pts',(6.19791525764518,-5.41488061733235,99.1324027492867));
#71515=CARTESIAN_POINT('Ctrl Pts',(8.71518000520262,-0.585773588572133,
99.3445570547845));
#71516=CARTESIAN_POINT('Ctrl Pts',(6.65427538192215,6.59313465225967,99.6097499366571));
#71517=CARTESIAN_POINT('Ctrl Pts',(-1.96138467738728,9.1590332808326,99.9279813949035));
#71518=CARTESIAN_POINT('Ctrl Pts',(-8.75822973423427,3.30188804874659,100.24621285315));
#71519=CARTESIAN_POINT('Ctrl Pts',(-7.5197909544385,-5.58459170339549,100.564444311397));
#71520=CARTESIAN_POINT('Ctrl Pts',(0.645470626059692,-9.34516843466058,
100.882675769644));
#71521=CARTESIAN_POINT('Ctrl Pts',(6.93278121039915,-5.31357110697587,101.147868651516));
#71522=CARTESIAN_POINT('Ctrl Pts',(8.23009620377064,-0.0245380845330745,
101.360022957014));
#71523=CARTESIAN_POINT('Ctrl Pts',(6.96434256614091,5.27213674344548,101.572177262512));
#71524=CARTESIAN_POINT('Ctrl Pts',(0.70118401419441,9.34115337522732,101.837370144385));
#71525=CARTESIAN_POINT('Ctrl Pts',(-7.48635656723482,5.62933262832376,102.155601602631));
#71526=CARTESIAN_POINT('Ctrl Pts',(-8.77776305084519,-3.24960437396555,
102.473833060878));
#71527=CARTESIAN_POINT('Ctrl Pts',(-2.01596475396907,-9.14717478803391,
102.792064519125));
#71528=CARTESIAN_POINT('Ctrl Pts',(6.61484248131537,-6.63269661213821,103.110295977372));
#71529=CARTESIAN_POINT('Ctrl Pts',(8.71851800583927,0.533794906314948,103.375488859244));
#71530=CARTESIAN_POINT('Ctrl Pts',(6.23009378281474,5.37782642879489,103.587643164742));
#71531=CARTESIAN_POINT('Ctrl Pts',(1.80145433659379,8.54706121970112,103.79979747024));
#71532=CARTESIAN_POINT('Ctrl Pts',(-5.59543948843153,7.5126468260251,104.064990352112));
#71533=CARTESIAN_POINT('Ctrl Pts',(-9.34352656472846,-0.658355395134159,
104.383221810359));
#71534=CARTESIAN_POINT('Ctrl Pts',(-4.49679376123124,-8.20901325574707,
104.701453268606));
#71535=CARTESIAN_POINT('Ctrl Pts',(4.47554607962198,-8.22826882043062,105.019684726852));
#71536=CARTESIAN_POINT('Ctrl Pts',(9.34339464641931,-0.670657798393084,
105.3379161851));
#71537=CARTESIAN_POINT('Ctrl Pts',(6.23277820874136,6.11963798118718,105.603109066971));
#71538=CARTESIAN_POINT('Ctrl Pts',(1.17777217816441,8.14542438042699,105.81526337247));
#71539=CARTESIAN_POINT('Ctrl Pts',(-4.24402311581608,7.63451118360377,106.027417677967));
#71540=CARTESIAN_POINT('Ctrl Pts',(-9.15068093692945,2.0034579585802,106.29261055984));
#71541=CARTESIAN_POINT('Ctrl Pts',(-6.62300858976339,-6.62349437321487,
106.610842018087));
#71542=CARTESIAN_POINT('Ctrl Pts',(1.98729643490681,-9.14656797076846,106.929073476333));
#71543=CARTESIAN_POINT('Ctrl Pts',(8.77434591518241,-3.27807477840434,107.24730493458));
#71544=CARTESIAN_POINT('Ctrl Pts',(7.49432346999941,5.61995739559459,107.565536392827));
#71545=CARTESIAN_POINT('Ctrl Pts',(0.693404043131489,8.70727764879019,107.830729274699));
#71546=CARTESIAN_POINT('Ctrl Pts',(-4.45157711479331,6.92232235828129,108.042883580197));
#71547=CARTESIAN_POINT('Ctrl Pts',(-8.21021996282278,2.98157364192402,108.255037885695));
#71548=CARTESIAN_POINT('Ctrl Pts',(-8.22271556040278,-4.48728806897804,
108.520230767568));
#71549=CARTESIAN_POINT('Ctrl Pts',(-0.657670090896665,-9.34357482677965,
108.838462225814));
#71550=CARTESIAN_POINT('Ctrl Pts',(7.49774751044503,-5.60293093244015,109.156693684061));
#71551=CARTESIAN_POINT('Ctrl Pts',(8.77431730691419,3.278151352466,109.474925142308));
#71552=CARTESIAN_POINT('Ctrl Pts',(1.97354716461479,9.15717844045453,109.793156600555));
#71553=CARTESIAN_POINT('Ctrl Pts',(-5.1856906044942,7.02894772882912,110.058349482427));
#71554=CARTESIAN_POINT('Ctrl Pts',(-7.89995856057946,2.30775656905988,110.270503787925));
#71555=CARTESIAN_POINT('Ctrl Pts',(-8.1539714392633,-3.13213074245472,110.482658093423));
#71556=CARTESIAN_POINT('Ctrl Pts',(-3.26618282646103,-8.77957032806362,
110.747850975295));
#71557=CARTESIAN_POINT('Ctrl Pts',(5.62988170121529,-7.4859436627864,111.066082433542));
#71558=CARTESIAN_POINT('Ctrl Pts',(9.33481591175152,0.685758454406295,111.384313891789));
#71559=CARTESIAN_POINT('Ctrl Pts',(4.4754742709089,8.22830787844749,111.702545350036));
#71560=CARTESIAN_POINT('Ctrl Pts',(-4.51413206077047,8.20800932865017,112.020776808283));
#71561=CARTESIAN_POINT('Ctrl Pts',(-8.5241520827663,1.90691491420638,112.285969690155));
#71562=CARTESIAN_POINT('Ctrl Pts',(-7.47790146957128,-3.43745185454216,
112.498123995653));
#71563=CARTESIAN_POINT('Ctrl Pts',(-4.10283546858128,-7.71130561824021,
112.71027830115));
#71564=CARTESIAN_POINT('Ctrl Pts',(3.29055575448777,-8.77046453888797,112.975471183023));
#71565=CARTESIAN_POINT('Ctrl Pts',(9.15917711427336,-1.96071290133453,113.29370264127));
#71566=CARTESIAN_POINT('Ctrl Pts',(6.59846396386631,6.63847317397886,113.611934099517));
#71567=CARTESIAN_POINT('Ctrl Pts',(-2.0160445817765,9.1471571942533,113.930165557764));
#71568=CARTESIAN_POINT('Ctrl Pts',(-8.79019580055429,3.23747790559259,114.24839701601));
#71569=CARTESIAN_POINT('Ctrl Pts',(-7.68636295647619,-4.14937558211616,
114.513589897883));
#71570=CARTESIAN_POINT('Ctrl Pts',(-3.39218490487877,-7.49854433953852,
114.72574420338));
#71571=CARTESIAN_POINT('Ctrl Pts',(1.95840883190445,-8.51246897599455,114.937898508878));
#71572=CARTESIAN_POINT('Ctrl Pts',(8.23514742327505,-4.46443191438829,115.203091390751));
#71573=CARTESIAN_POINT('Ctrl Pts',(8.20110315740802,4.52513287027477,115.521322848998));
#71574=CARTESIAN_POINT('Ctrl Pts',(0.629316677428787,9.33879078272935,115.839554307244));
#71575=CARTESIAN_POINT('Ctrl Pts',(-7.51983969118302,5.58452607756445,116.157785765491));
#71576=CARTESIAN_POINT('Ctrl Pts',(-8.75966573841591,-3.31919591957222,
116.476017223738));
#71577=CARTESIAN_POINT('Ctrl Pts',(-3.08278250781349,-8.17275628106395,
116.74121010561));
#71578=CARTESIAN_POINT('Ctrl Pts',(2.35546989393181,-7.88586375863123,116.953364411108));
#71579=CARTESIAN_POINT('Ctrl Pts',(7.06016695842124,-5.14310565119636,117.165518716606));
#71580=CARTESIAN_POINT('Ctrl Pts',(9.1450809734394,2.02886652851272,117.430711598479));
#71581=CARTESIAN_POINT('Ctrl Pts',(3.2250504401161,8.79397351319627,117.748943056725));
#71582=CARTESIAN_POINT('Ctrl Pts',(-5.64815267190185,7.46374062779295,118.067174514972));
#71583=CARTESIAN_POINT('Ctrl Pts',(-9.3394284711406,-0.714140269510792,
118.385405973219));
#71584=CARTESIAN_POINT('Ctrl Pts',(-4.43749951345246,-8.2496911135747,118.703637431466));
#71585=CARTESIAN_POINT('Ctrl Pts',(3.03115019488987,-8.19204624719432,118.968830313338));
#71586=CARTESIAN_POINT('Ctrl Pts',(6.94910579760224,-4.40965012837104,119.180984618836));
#71587=CARTESIAN_POINT('Ctrl Pts',(8.70292690633611,0.746027132966607,119.393138924334));
#71588=CARTESIAN_POINT('Ctrl Pts',(5.57455129708413,7.52815935255504,119.658331806206));
#71589=CARTESIAN_POINT('Ctrl Pts',(-3.33105607249802,8.75436953377928,119.976563264453));
#71590=CARTESIAN_POINT('Ctrl Pts',(-9.15841411812871,1.93196884160687,120.2947947227));
#71591=CARTESIAN_POINT('Ctrl Pts',(-6.58333706377255,-6.66292680410411,
120.613026180947));
#71592=CARTESIAN_POINT('Ctrl Pts',(2.05873749836002,-9.13840277696978,120.931257639193));
#71593=CARTESIAN_POINT('Ctrl Pts',(7.66002694000164,-4.19779471849209,121.196450521066));
#71594=CARTESIAN_POINT('Ctrl Pts',(8.1381558836316,1.22698999776883,121.408604826563));
#71595=CARTESIAN_POINT('Ctrl Pts',(6.08184883245779,6.26965772584783,121.620759132062));
#71596=CARTESIAN_POINT('Ctrl Pts',(-0.727126650508542,9.33916978298414,
121.885952013934));
#71597=CARTESIAN_POINT('Ctrl Pts',(-8.25517329145266,4.42572416901183,122.204183472181));
#71598=CARTESIAN_POINT('Ctrl Pts',(-8.18168001027664,-4.54633533447753,
122.522414930428));
#71599=CARTESIAN_POINT('Ctrl Pts',(-0.601861462684696,-9.3473356242207,
122.840646388674));
#71600=CARTESIAN_POINT('Ctrl Pts',(7.54633416229053,-5.54992307264971,123.158877846921));
#71601=CARTESIAN_POINT('Ctrl Pts',(8.53601520676025,1.85308866763243,123.424070728793));
#71602=CARTESIAN_POINT('Ctrl Pts',(5.34006706141108,6.2624890754831,123.636225034291));
#71603=CARTESIAN_POINT('Ctrl Pts',(0.481081445579293,8.72158551313186,123.848379339789));
#71604=CARTESIAN_POINT('Ctrl Pts',(-6.67256234851482,6.57462676556356,124.113572221662));
#71605=CARTESIAN_POINT('Ctrl Pts',(-9.13482108817629,-2.07122287045563,
124.431803679908));
#71606=CARTESIAN_POINT('Ctrl Pts',(-3.19648315358039,-8.79724662681214,
124.750035138155));
#71607=CARTESIAN_POINT('Ctrl Pts',(5.674485026791,-7.45219029365284,125.068266596402));
#71608=CARTESIAN_POINT('Ctrl Pts',(9.33674402083647,0.757638760001384,125.386498054649));
#71609=CARTESIAN_POINT('Ctrl Pts',(5.22994075083988,6.99608554570746,125.651690936521));
#71610=CARTESIAN_POINT('Ctrl Pts',(-0.074288819055751,8.22979749521674,
125.863845242019));
#71611=CARTESIAN_POINT('Ctrl Pts',(-5.35538289490079,6.90053383943257,126.075999547517));
#71612=CARTESIAN_POINT('Ctrl Pts',(-9.34889957533105,0.588967003878703,
126.341192429389));
#71613=CARTESIAN_POINT('Ctrl Pts',(-5.53903229934317,-7.55341258497928,
126.659423887636));
#71614=CARTESIAN_POINT('Ctrl Pts',(3.35477148493349,-8.73810969534923,126.977655345883));
#71615=CARTESIAN_POINT('Ctrl Pts',(9.17072256306931,-1.90598220435038,127.29588680413));
#71616=CARTESIAN_POINT('Ctrl Pts',(6.55278888881734,6.69400949953583,127.614118262377));
#71617=CARTESIAN_POINT('Ctrl Pts',(-0.638446414948493,8.71147974774613,
127.879311144249));
#71618=CARTESIAN_POINT('Ctrl Pts',(-5.45224826706981,6.1650688945985,128.091465449747));
#71619=CARTESIAN_POINT('Ctrl Pts',(-8.56807646788026,1.69869328035053,128.303619755244));
#71620=CARTESIAN_POINT('Ctrl Pts',(-7.44491642255176,-5.68524624466725,
128.568812637117));
#71621=CARTESIAN_POINT('Ctrl Pts',(0.770502884933684,-9.33494755188252,
128.887044095364));
#71622=CARTESIAN_POINT('Ctrl Pts',(8.26241790223238,-4.39789758554576,129.205275553611));
#71623=CARTESIAN_POINT('Ctrl Pts',(8.17393425039314,4.57402660271456,129.523507011857));
#71624=CARTESIAN_POINT('Ctrl Pts',(0.558416076215122,9.35077413303877,129.841738470104));
#71625=CARTESIAN_POINT('Ctrl Pts',(-6.19403857185828,6.15884562158216,130.106931351977));
#71626=CARTESIAN_POINT('Ctrl Pts',(-8.1589795506303,1.07987885121863,130.319085657474));
#71627=CARTESIAN_POINT('Ctrl Pts',(-7.58299949647197,-4.33539062330698,
130.531239962973));
#71628=CARTESIAN_POINT('Ctrl Pts',(-1.89343420960715,-9.17407828041441,
130.796432844844));
#71629=CARTESIAN_POINT('Ctrl Pts',(6.70254443608692,-6.54299767494756,131.114664303092));
#71630=CARTESIAN_POINT('Ctrl Pts',(9.12204553428414,2.09698307921827,131.432895761338));
#71631=CARTESIAN_POINT('Ctrl Pts',(3.1724780806205,8.81307570148307,131.751127219585));
#71632=CARTESIAN_POINT('Ctrl Pts',(-5.70954236147284,7.42629998207919,132.069358677832));
#71633=CARTESIAN_POINT('Ctrl Pts',(-8.71497612861151,0.588799030131614,
132.334551559705));
#71634=CARTESIAN_POINT('Ctrl Pts',(-6.86836975556092,-4.53437785609103,
132.546705865202));
#71635=CARTESIAN_POINT('Ctrl Pts',(-2.88277221755536,-8.2454301016891,132.7588601707));
#71636=CARTESIAN_POINT('Ctrl Pts',(4.58570106323024,-8.16824039557919,133.024053052572));
#71637=CARTESIAN_POINT('Ctrl Pts',(9.3507983469536,-0.545427141514346,133.342284510819));
#71638=CARTESIAN_POINT('Ctrl Pts',(5.51249572704322,7.56448568135409,133.660515969066));
#71639=CARTESIAN_POINT('Ctrl Pts',(-3.38327502959951,8.7343214141785,133.978747427313));
#71640=CARTESIAN_POINT('Ctrl Pts',(-9.18021615344449,1.8634475515343,134.29697888556));
#71641=CARTESIAN_POINT('Ctrl Pts',(-6.96617237004453,-5.26971875255023,
134.562171767432));
#71642=CARTESIAN_POINT('Ctrl Pts',(-2.21272927292213,-7.92710002495654,
134.77432607293));
#71643=CARTESIAN_POINT('Ctrl Pts',(3.22981597415152,-8.11577365340277,134.986480378428));
#71644=CARTESIAN_POINT('Ctrl Pts',(8.8181569418351,-3.16052425246951,135.2516732603));
#71645=CARTESIAN_POINT('Ctrl Pts',(7.41780161019791,5.7193653287612,135.569904718547));
#71646=CARTESIAN_POINT('Ctrl Pts',(-0.797799373005577,9.32590847716784,
135.888136176794));
#71647=CARTESIAN_POINT('Ctrl Pts',(-8.28145513424959,4.3763479468045,136.206367635041));
#71648=CARTESIAN_POINT('Ctrl Pts',(-8.15321288750148,-4.61236653057451,
136.524599093288));
#71649=CARTESIAN_POINT('Ctrl Pts',(-1.80442134242299,-8.54643532937329,
136.78979197516));
#71650=CARTESIAN_POINT('Ctrl Pts',(3.52699697848842,-7.43608619871,137.001946280658));
#71651=CARTESIAN_POINT('Ctrl Pts',(7.76001558530448,-4.00994405646551,137.214100586155));
#71652=CARTESIAN_POINT('Ctrl Pts',(8.73031997466621,3.39563227414694,137.479293468028));
#71653=CARTESIAN_POINT('Ctrl Pts',(1.85059021392886,9.18206057223537,137.797524926275));
#71654=CARTESIAN_POINT('Ctrl Pts',(-6.71722743062202,6.51827495656469,138.115756384522));
#71655=CARTESIAN_POINT('Ctrl Pts',(-9.12228951404036,-2.12573622872636,
138.433987842768));
#71656=CARTESIAN_POINT('Ctrl Pts',(-3.1316938128374,-8.82843696607267,138.752219301015));
#71657=CARTESIAN_POINT('Ctrl Pts',(4.24137253767331,-7.63598403722936,139.017412182888));
#71658=CARTESIAN_POINT('Ctrl Pts',(7.53873631452235,-3.30189951709841,139.229566488385));
#71659=CARTESIAN_POINT('Ctrl Pts',(8.48833913126387,2.06048344152671,139.441720793883));
#71660=CARTESIAN_POINT('Ctrl Pts',(4.36522425868474,8.28816159185334,139.706913675756));
#71661=CARTESIAN_POINT('Ctrl Pts',(-4.62328361922247,8.14617511893268,140.025145134002));
#71662=CARTESIAN_POINT('Ctrl Pts',(-9.34567418643476,0.517133217931129,
140.343376592249));
#71663=CARTESIAN_POINT('Ctrl Pts',(-5.49382692117094,-7.58635526799968,
140.661608050496));
#71664=CARTESIAN_POINT('Ctrl Pts',(3.42414070483787,-8.71917804811639,140.979839508743));
#71665=CARTESIAN_POINT('Ctrl Pts',(8.20918441408827,-2.98442364211942,141.245032390615));
#71666=CARTESIAN_POINT('Ctrl Pts',(7.85701127011543,2.44999174329057,141.457186696113));
#71667=CARTESIAN_POINT('Ctrl Pts',(5.0579579656616,7.12141519908443,141.669341001611));
#71668=CARTESIAN_POINT('Ctrl Pts',(-2.13853232026243,9.12005947987599,141.934533883483));
#71669=CARTESIAN_POINT('Ctrl Pts',(-8.8320651801613,3.11922188141106,142.25276534173));
#71670=CARTESIAN_POINT('Ctrl Pts',(-7.39538078226736,-5.73736837316092,
142.570996799977));
#71671=CARTESIAN_POINT('Ctrl Pts',(0.82623452846722,-9.3301799015914,142.889228258224));
#71672=CARTESIAN_POINT('Ctrl Pts',(8.30238083543134,-4.3381191621197,143.20745971647));
#71673=CARTESIAN_POINT('Ctrl Pts',(8.15505826787976,3.12929990055637,143.472652598343));
#71674=CARTESIAN_POINT('Ctrl Pts',(4.32588891929462,7.00155487722944,143.684806903841));
#71675=CARTESIAN_POINT('Ctrl Pts',(-0.850476126127729,8.69334133570097,
143.896961209339));
#71676=CARTESIAN_POINT('Ctrl Pts',(-7.59455455464446,5.48375295922304,144.162154091211));
#71677=CARTESIAN_POINT('Ctrl Pts',(-8.71373981128762,-3.43593640707434,
144.480385549458));
#71678=CARTESIAN_POINT('Ctrl Pts',(-1.82185738840104,-9.18095247891603,
144.798617007704));
#71679=CARTESIAN_POINT('Ctrl Pts',(6.74149765731627,-6.5028555134215,145.116848465952));
#71680=CARTESIAN_POINT('Ctrl Pts',(9.11302308107979,2.16832094631068,145.435079924198));
#71681=CARTESIAN_POINT('Ctrl Pts',(4.10551220288046,7.70988085316744,145.700272806071));
#71682=CARTESIAN_POINT('Ctrl Pts',(-1.32462267258781,8.1228357374562,145.912427111569));
#71683=CARTESIAN_POINT('Ctrl Pts',(-6.34223517519423,6.00612572323542,146.124581417066));
#71684=CARTESIAN_POINT('Ctrl Pts',(-9.32976529389266,-0.839216866339801,
146.389774298939));
#71685=CARTESIAN_POINT('Ctrl Pts',(-4.32627883899791,-8.30772122338493,
146.708005757186));
#71686=CARTESIAN_POINT('Ctrl Pts',(4.64425132809667,-8.12649877591966,147.026237215432));
#71687=CARTESIAN_POINT('Ctrl Pts',(9.35388873200124,-0.489577381506351,
147.344468673679));
#71688=CARTESIAN_POINT('Ctrl Pts',(5.45890827904218,7.6124323307205,147.662700131926));
#71689=CARTESIAN_POINT('Ctrl Pts',(-1.95545362162443,8.51314831325412,147.927893013798));
#71690=CARTESIAN_POINT('Ctrl Pts',(-6.32615987565755,5.26448352733551,148.140047319296));
#71691=CARTESIAN_POINT('Ctrl Pts',(-8.72673348322189,0.376319895862742,
148.352201624794));
#71692=CARTESIAN_POINT('Ctrl Pts',(-6.49403004923184,-6.75102783357787,
148.617394506666));
#71693=CARTESIAN_POINT('Ctrl Pts',(2.18076225489512,-9.10929186686864,148.935625964913));
#71694=CARTESIAN_POINT('Ctrl Pts',(8.83499531207604,-3.09061709943564,149.25385742316));
#71695=CARTESIAN_POINT('Ctrl Pts',(7.3835145506797,5.76355965835638,149.572088881407));
#71696=CARTESIAN_POINT('Ctrl Pts',(-0.869696582671238,9.32697427212434,
149.890320339654));
#71697=CARTESIAN_POINT('Ctrl Pts',(-7.05838296506824,5.14555462476081,150.155513221526));
#71698=CARTESIAN_POINT('Ctrl Pts',(-8.22830963069686,-0.173102801086107,
150.367667527024));
#71699=CARTESIAN_POINT('Ctrl Pts',(-6.83573616555874,-5.43786222374656,
150.579821832522));
#71700=CARTESIAN_POINT('Ctrl Pts',(-0.476652214192424,-9.35528631577552,
150.845014714394));
#71701=CARTESIAN_POINT('Ctrl Pts',(7.61935789093666,-5.44795245820723,151.163246172641));
#71702=CARTESIAN_POINT('Ctrl Pts',(8.69723581861135,3.45948991911445,151.481477630888));
#71703=CARTESIAN_POINT('Ctrl Pts',(1.79565016362255,9.19288163891025,151.799709089134));
#71704=CARTESIAN_POINT('Ctrl Pts',(-6.77206314673528,6.47206797128248,152.117940547382));
#71705=CARTESIAN_POINT('Ctrl Pts',(-8.70344421466748,-0.743235911204164,
152.383133429254));
#71706=CARTESIAN_POINT('Ctrl Pts',(-6.09880948545569,-5.52557681829827,
152.595287734752));
#71707=CARTESIAN_POINT('Ctrl Pts',(-1.5965286468446,-8.58860403723511,152.807442040249));
#71708=CARTESIAN_POINT('Ctrl Pts',(5.77602026715138,-7.37452398921601,153.072634922122));
#71709=CARTESIAN_POINT('Ctrl Pts',(9.32202208613815,0.879870536452235,153.390866380369));
#71710=CARTESIAN_POINT('Ctrl Pts',(4.30386720274188,8.31953572883633,153.709097838616));
#71711=CARTESIAN_POINT('Ctrl Pts',(-4.68236941490573,8.10893564657233,154.027329296862));
#71712=CARTESIAN_POINT('Ctrl Pts',(-8.55961986197294,1.74030325657316,154.292522178735));
#71713=CARTESIAN_POINT('Ctrl Pts',(-7.40882346442135,-3.60417112039676,
154.504690271996));
#71714=CARTESIAN_POINT('Ctrl Pts',(-5.66997762825804,-5.68039998745807,
154.610781212507));
#71715=CARTESIAN_POINT('Ctrl Pts',(-4.59556679602214,-6.44633620500796,
154.663833576644));
#71716=CARTESIAN_POINT('Ctrl Pts',(-3.93864885562957,-5.51416611762882,
-4.5102810375397E-17));
#71717=CARTESIAN_POINT('Ctrl Pts',(-4.08585763522341,-5.42754158645561,
-9.48998345292704E-15));
#71718=CARTESIAN_POINT('Ctrl Pts',(-4.22926307194498,-5.33519815285744,
-8.48289216403754E-15));
#71719=CARTESIAN_POINT('Ctrl Pts',(-4.36847541855169,-5.23720844074822,
-7.17481629664007E-15));
#71720=CARTESIAN_POINT('Ctrl Pts',(-4.5153143814705,-5.13385045524223,-6.2635930340045E-15));
#71721=CARTESIAN_POINT('Ctrl Pts',(-4.65748939328674,-5.02421136591519,
-8.76666634847064E-15));
#71722=CARTESIAN_POINT('Ctrl Pts',(-4.79490097280245,-4.90875376760295,
-7.57727214306669E-15));
#71723=CARTESIAN_POINT('Ctrl Pts',(-4.9348947149667,-4.79112655375393,-6.36552749745673E-15));
#71724=CARTESIAN_POINT('Ctrl Pts',(-5.06994473026214,-4.66745971743739,
-3.71552428771349E-15));
#71725=CARTESIAN_POINT('Ctrl Pts',(-5.19991919475653,-4.53819530501257,
-3.6498581934552E-15));
#71726=CARTESIAN_POINT('Ctrl Pts',(-5.23498113790099,-4.50332490568703,
-3.6321440919018E-15));
#71727=CARTESIAN_POINT('Ctrl Pts',(-5.26967356318341,-4.46804692542487,
-2.38309310078048E-15));
#71728=CARTESIAN_POINT('Ctrl Pts',(-5.30399349825367,-4.43236952795225,
-3.17801340798951E-15));
#71729=CARTESIAN_POINT('Ctrl Pts',(-5.33072700462355,-4.40457862652305,
-3.79721641792535E-15));
#71730=CARTESIAN_POINT('Ctrl Pts',(-5.35723606352971,-4.37654348380284,
-3.20335373337224E-15));
#71731=CARTESIAN_POINT('Ctrl Pts',(-5.38349836887505,-4.34829087335799,
-2.5951463200613E-15));
#71732=CARTESIAN_POINT('Ctrl Pts',(-5.51182776783945,-4.21023595129815,
3.76827799100414E-16));
#71733=CARTESIAN_POINT('Ctrl Pts',(-5.63438296049573,-4.06687452090324,
1.5979460223273E-16));
#71734=CARTESIAN_POINT('Ctrl Pts',(-5.75105261248448,-3.91872155205454,
7.7715611723761E-16));
#71735=CARTESIAN_POINT('Ctrl Pts',(-5.86802410885443,-3.77018528608921,
1.39611485226759E-15));
#71736=CARTESIAN_POINT('Ctrl Pts',(-5.97907994344739,-3.61683206879924,
2.92190851021412E-15));
#71737=CARTESIAN_POINT('Ctrl Pts',(-6.08407689566617,-3.45913508104809,
2.33146835171283E-15));
#71738=CARTESIAN_POINT('Ctrl Pts',(-6.16258753371837,-3.3412184095103,1.889971407316E-15));
#71739=CARTESIAN_POINT('Ctrl Pts',(-6.23770993659032,-3.22087206005872,
2.51853654700645E-15));
#71740=CARTESIAN_POINT('Ctrl Pts',(-6.3093710339331,-3.09828019800675,2.4980018054066E-15));
#71741=CARTESIAN_POINT('Ctrl Pts',(-6.3341774208916,-3.05584348853973,2.49089344724426E-15));
#71742=CARTESIAN_POINT('Ctrl Pts',(-6.35856893839169,-3.01313761181226,
1.25464931670994E-15));
#71743=CARTESIAN_POINT('Ctrl Pts',(-6.38254220714328,-2.9701699351918,2.13717932240343E-15));
#71744=CARTESIAN_POINT('Ctrl Pts',(-6.4036413320246,-2.9323536330317,2.9139032224517E-15));
#71745=CARTESIAN_POINT('Ctrl Pts',(-6.42441971552428,-2.89432817575107,
3.01420564380196E-15));
#71746=CARTESIAN_POINT('Ctrl Pts',(-6.44485308977601,-2.85614028785739,
2.44249065417534E-15));
#71747=CARTESIAN_POINT('Ctrl Pts',(-6.47726144497496,-2.79557238458748,
1.53572203984232E-15));
#71748=CARTESIAN_POINT('Ctrl Pts',(-6.50881123945918,-2.73458002559567,
4.5774480660375E-15));
#71749=CARTESIAN_POINT('Ctrl Pts',(-6.53949852066889,-2.67318520039554,
4.35762537165374E-15));
#71750=CARTESIAN_POINT('Ctrl Pts',(-6.62571770655248,-2.50068989818723,
3.74001009257501E-15));
#71751=CARTESIAN_POINT('Ctrl Pts',(-6.70512878428164,-2.32502421973284,
2.90696192907388E-15));
#71752=CARTESIAN_POINT('Ctrl Pts',(-6.77760467320117,-2.1466793262714,4.57966997657877E-15));
#71753=CARTESIAN_POINT('Ctrl Pts',(-6.85107121035924,-1.96589669720997,
6.2752417006187E-15));
#71754=CARTESIAN_POINT('Ctrl Pts',(-6.91741213237192,-1.78236052985066,
6.40827725235636E-15));
#71755=CARTESIAN_POINT('Ctrl Pts',(-6.97645624116144,-1.59654609617019,
6.41153796721028E-15));
#71756=CARTESIAN_POINT('Ctrl Pts',(-7.03541281540019,-1.41100713761017,
6.41479384796279E-15));
#71757=CARTESIAN_POINT('Ctrl Pts',(-7.08709457358015,-1.22319598087583,
8.11353623083457E-15));
#71758=CARTESIAN_POINT('Ctrl Pts',(-7.13128646726196,-1.03355947757627,
5.93969318174459E-15));
#71759=CARTESIAN_POINT('Ctrl Pts',(-7.1748356573002,-0.84668094777523,3.79746536186948E-15));
#71760=CARTESIAN_POINT('Ctrl Pts',(-7.21111152210714,-0.658029091154123,
4.52783243078309E-15));
#71761=CARTESIAN_POINT('Ctrl Pts',(-7.23986029137286,-0.468016202745084,
4.27435864480685E-15));
#71762=CARTESIAN_POINT('Ctrl Pts',(-7.24843435095544,-0.411346582852196,
4.19876238802472E-15));
#71763=CARTESIAN_POINT('Ctrl Pts',(-7.25633855027266,-0.354555835328044,
3.81851370664238E-15));
#71764=CARTESIAN_POINT('Ctrl Pts',(-7.26356525899322,-0.297654766670134,
2.33146835171283E-15));
#71765=CARTESIAN_POINT('Ctrl Pts',(-7.26643816125284,-0.275034343591875,
2.05066034735898E-15));
#71766=CARTESIAN_POINT('Ctrl Pts',(-7.26920381458604,-0.25239753682228,
6.88911783367723E-15));
#71767=CARTESIAN_POINT('Ctrl Pts',(-7.27186036178065,-0.229757926941342,
6.82787160144471E-15));
#71768=CARTESIAN_POINT('Ctrl Pts',(-7.29508985368643,-0.0317916963596518,
2.89494710093888E-15));
#71769=CARTESIAN_POINT('Ctrl Pts',(-7.31001436370851,0.166647965845849,
3.28825056680269E-15));
#71770=CARTESIAN_POINT('Ctrl Pts',(-7.31647360189607,0.365072157842635,
3.10862446895044E-15));
#71771=CARTESIAN_POINT('Ctrl Pts',(-7.32239953343523,0.547113467257426,
2.84891488009813E-15));
#71772=CARTESIAN_POINT('Ctrl Pts',(-7.32120010776079,0.729142519857608,
3.27746221103623E-15));
#71773=CARTESIAN_POINT('Ctrl Pts',(-7.31271643791274,0.910797816932271,
3.88578058618805E-15));
#71774=CARTESIAN_POINT('Ctrl Pts',(-7.30374392664761,1.10292035689018,4.19327191292733E-15));
#71775=CARTESIAN_POINT('Ctrl Pts',(-7.28662463969137,1.29462530195052,4.84441888438171E-15));
#71776=CARTESIAN_POINT('Ctrl Pts',(-7.26166737560021,1.48549791199764,3.33066907387547E-15));
#71777=CARTESIAN_POINT('Ctrl Pts',(-7.23635360931169,1.67909704305478,1.8476684640108E-15));
#71778=CARTESIAN_POINT('Ctrl Pts',(-7.20297622264173,1.87184053501143,2.85422380346747E-15));
#71779=CARTESIAN_POINT('Ctrl Pts',(-7.16180345191425,2.06329674672944,3.1641356201817E-15));
#71780=CARTESIAN_POINT('Ctrl Pts',(-7.13907515744559,2.16898487703731,4.63215597939171E-15));
#71781=CARTESIAN_POINT('Ctrl Pts',(-7.11397044673297,2.2742806998604,2.85116288317276E-15));
#71782=CARTESIAN_POINT('Ctrl Pts',(-7.08652776855258,2.3791106285664,1.49880108324396E-15));
#71783=CARTESIAN_POINT('Ctrl Pts',(-7.07123960516252,2.43751079883005,-4.23777917910264E-16));
#71784=CARTESIAN_POINT('Ctrl Pts',(-7.05522576098077,2.49576635929609,6.98375336362743E-16));
#71785=CARTESIAN_POINT('Ctrl Pts',(-7.03849227337608,2.55386441534103,9.43689570931383E-16));
#71786=CARTESIAN_POINT('Ctrl Pts',(-7.02101618737152,2.6145407458302,1.00858386228158E-15));
#71787=CARTESIAN_POINT('Ctrl Pts',(-7.00277560991787,2.67497411182156,3.28000556455198E-16));
#71788=CARTESIAN_POINT('Ctrl Pts',(-6.98378477400738,2.73514402802049,5.55111512312578E-16));
#71789=CARTESIAN_POINT('Ctrl Pts',(-6.92410274331356,2.92423853667474,1.26884750067373E-15));
#71790=CARTESIAN_POINT('Ctrl Pts',(-6.85700877086983,3.11075193737884,2.68086629815529E-15));
#71791=CARTESIAN_POINT('Ctrl Pts',(-6.78285079805515,3.29425396444948,1.66533453693773E-15));
#71792=CARTESIAN_POINT('Ctrl Pts',(-6.70769973559542,3.48021336671545,6.36203238974364E-16));
#71793=CARTESIAN_POINT('Ctrl Pts',(-6.62529404332015,3.6630808733105,-9.33836692105665E-17));
#71794=CARTESIAN_POINT('Ctrl Pts',(-6.53594209786488,3.84240790796595,-2.77555756156289E-16));
#71795=CARTESIAN_POINT('Ctrl Pts',(-6.44578821461818,4.0233444109478,-4.63380795994014E-16));
#71796=CARTESIAN_POINT('Ctrl Pts',(-6.34856261409735,4.20067733546166,1.67798683334567E-15));
#71797=CARTESIAN_POINT('Ctrl Pts',(-6.24453069856692,4.37393447487679,-7.7715611723761E-16));
#71798=CARTESIAN_POINT('Ctrl Pts',(-6.22727537286666,4.40267189026762,-1.18438010265586E-15));
#71799=CARTESIAN_POINT('Ctrl Pts',(-6.2098326865377,4.43129713518358,-1.42691211972322E-15));
#71800=CARTESIAN_POINT('Ctrl Pts',(-6.19220372232323,4.45980800258806,-1.22124532708767E-15));
#71801=CARTESIAN_POINT('Ctrl Pts',(-6.08596170519876,4.63163046624324,-1.41530437407216E-15));
#71802=CARTESIAN_POINT('Ctrl Pts',(-5.97295776163549,4.79930104647229,-1.50003702229236E-15));
#71803=CARTESIAN_POINT('Ctrl Pts',(-5.85345634600849,4.96251156798406,1.88737914186277E-15));
#71804=CARTESIAN_POINT('Ctrl Pts',(-5.81488241610479,5.01519438503113,2.98080513171597E-15));
#71805=CARTESIAN_POINT('Ctrl Pts',(-5.77563115178433,5.06741226883694,-1.31746641749658E-15));
#71806=CARTESIAN_POINT('Ctrl Pts',(-5.73571051010428,5.11915416998263,-2.66453525910038E-15));
#71807=CARTESIAN_POINT('Ctrl Pts',(-5.72137816578353,5.13773059340222,-2.96003365710495E-15));
#71808=CARTESIAN_POINT('Ctrl Pts',(-5.70695815007714,5.15624742332188,1.25829997975076E-15));
#71809=CARTESIAN_POINT('Ctrl Pts',(-5.69245532260261,5.17469841337795,9.99200722162641E-16));
#71810=CARTESIAN_POINT('Ctrl Pts',(-5.56612038982047,5.33542600891682,-5.38442201744225E-16));
#71811=CARTESIAN_POINT('Ctrl Pts',(-5.43376647828372,5.4908295940974,6.83770205204893E-17));
#71812=CARTESIAN_POINT('Ctrl Pts',(-5.2957647648533,5.64065053822135,-7.7715611723761E-16));
#71813=CARTESIAN_POINT('Ctrl Pts',(-5.15609478068988,5.79228263301915,3.30164136699358E-16));
#71814=CARTESIAN_POINT('Ctrl Pts',(-5.01063933152216,5.93819685285966,-2.71421503180125E-15));
#71815=CARTESIAN_POINT('Ctrl Pts',(-4.85973389667245,6.07810484637022,-1.22124532708767E-15));
#71816=CARTESIAN_POINT('Ctrl Pts',(-4.7089054661251,6.21794144737296,5.73169886049089E-16));
#71817=CARTESIAN_POINT('Ctrl Pts',(-4.55263221916868,6.35177848028246,-5.16154924826819E-16));
#71818=CARTESIAN_POINT('Ctrl Pts',(-4.39120541678212,6.47929982942619,1.55431223447522E-15));
#71819=CARTESIAN_POINT('Ctrl Pts',(-4.23176612557716,6.60525111645157,2.78351566838913E-15));
#71820=CARTESIAN_POINT('Ctrl Pts',(-4.06729895549648,6.72504173207748,-1.21935944349465E-15));
#71821=CARTESIAN_POINT('Ctrl Pts',(-3.89804823092294,6.83833238416448,-5.55111512312578E-16));
#71822=CARTESIAN_POINT('Ctrl Pts',(-3.74289087714262,6.94218941538343,-1.70801214086168E-15));
#71823=CARTESIAN_POINT('Ctrl Pts',(-3.58371283294784,7.04058382880945,1.8720578375122E-15));
#71824=CARTESIAN_POINT('Ctrl Pts',(-3.42067962509758,7.13322310757502,-1.77635683940025E-15));
#71825=CARTESIAN_POINT('Origin',(-2.30940107675851,-4.,-10.));
#71826=CARTESIAN_POINT('',(-2.30940107675851,-4.,-10.));
#71827=CARTESIAN_POINT('',(2.3094010767585,-4.,-10.));
#71828=CARTESIAN_POINT('',(-1.15470053837925,-4.,-10.));
#71829=CARTESIAN_POINT('',(-2.30940107675851,-4.,-6.));
#71830=CARTESIAN_POINT('',(-2.30940107675851,-4.,-10.));
#71831=CARTESIAN_POINT('',(2.3094010767585,-4.,-6.));
#71832=CARTESIAN_POINT('',(-2.30940107675851,-4.,-6.));
#71833=CARTESIAN_POINT('',(2.3094010767585,-4.,-10.));
#71834=CARTESIAN_POINT('Origin',(-4.61880215351701,5.6564012731995E-16,
-10.));
#71835=CARTESIAN_POINT('',(-4.61880215351701,5.6564012731995E-16,-10.));
#71836=CARTESIAN_POINT('',(-4.04145188432738,-0.999999999999999,-10.));
#71837=CARTESIAN_POINT('',(-4.61880215351701,5.55111512312578E-16,-6.));
#71838=CARTESIAN_POINT('',(-4.61880215351701,5.6564012731995E-16,-10.));
#71839=CARTESIAN_POINT('',(-4.61880215351701,5.6564012731995E-16,-6.));
#71840=CARTESIAN_POINT('Origin',(-2.3094010767585,4.,-10.));
#71841=CARTESIAN_POINT('',(-2.3094010767585,4.,-10.));
#71842=CARTESIAN_POINT('',(-2.88675134594813,3.,-10.));
#71843=CARTESIAN_POINT('',(-2.3094010767585,4.,-6.));
#71844=CARTESIAN_POINT('',(-2.3094010767585,4.,-10.));
#71845=CARTESIAN_POINT('',(-2.3094010767585,4.,-6.));
#71846=CARTESIAN_POINT('Origin',(2.3094010767585,4.,-10.));
#71847=CARTESIAN_POINT('',(2.3094010767585,4.,-10.));
#71848=CARTESIAN_POINT('',(1.15470053837925,4.,-10.));
#71849=CARTESIAN_POINT('',(2.3094010767585,4.,-6.));
#71850=CARTESIAN_POINT('',(2.3094010767585,4.,-10.));
#71851=CARTESIAN_POINT('',(2.3094010767585,4.,-6.));
#71852=CARTESIAN_POINT('Origin',(4.61880215351701,0.,-10.));
#71853=CARTESIAN_POINT('',(4.61880215351701,0.,-10.));
#71854=CARTESIAN_POINT('',(4.04145188432738,1.,-10.));
#71855=CARTESIAN_POINT('',(4.61880215351701,0.,-6.));
#71856=CARTESIAN_POINT('',(4.61880215351701,0.,-10.));
#71857=CARTESIAN_POINT('',(4.61880215351701,0.,-6.));
#71858=CARTESIAN_POINT('Origin',(2.3094010767585,-4.,-10.));
#71859=CARTESIAN_POINT('',(2.88675134594813,-3.,-10.));
#71860=CARTESIAN_POINT('',(2.3094010767585,-4.,-6.));
#71861=CARTESIAN_POINT('Origin',(0.,0.,-6.));
#71862=CARTESIAN_POINT('Origin',(0.,0.,0.));
#71863=CARTESIAN_POINT('',(-45.,5.51091059616309E-15,0.));
#71864=CARTESIAN_POINT('Origin',(0.,0.,0.));
#71865=CARTESIAN_POINT('Origin',(0.,0.,-10.));
#71866=CARTESIAN_POINT('',(-45.,5.51091059616309E-15,-10.));
#71867=CARTESIAN_POINT('',(-45.,-5.51091059616309E-15,-10.));
#71868=CARTESIAN_POINT('Origin',(0.,0.,-10.));
#71869=CARTESIAN_POINT('Origin',(0.,0.,-10.));
#71870=CARTESIAN_POINT('',(0.,0.,0.));
#71871=CARTESIAN_POINT('Origin',(-1.,0.,1.));
#71872=CARTESIAN_POINT('',(-1.,3.87298334620742,0.));
#71873=CARTESIAN_POINT('',(-1.,3.87298334620742,1.));
#71874=CARTESIAN_POINT('',(-1.,3.87298334620742,0.));
#71875=CARTESIAN_POINT('',(-1.,7.93725393319377,0.));
#71876=CARTESIAN_POINT('',(-1.,0.,0.));
#71877=CARTESIAN_POINT('',(-1.,7.93725393319377,1.));
#71878=CARTESIAN_POINT('',(-1.,7.93725393319377,0.));
#71879=CARTESIAN_POINT('',(-1.,0.,1.));
#71880=CARTESIAN_POINT('Origin',(1.,16.,1.));
#71881=CARTESIAN_POINT('',(1.,3.87298334620742,1.));
#71882=CARTESIAN_POINT('',(1.,3.87298334620742,0.));
#71883=CARTESIAN_POINT('',(1.,3.87298334620742,0.));
#71884=CARTESIAN_POINT('',(1.,7.93725393319377,1.));
#71885=CARTESIAN_POINT('',(1.,8.,1.));
#71886=CARTESIAN_POINT('',(1.,7.93725393319377,0.));
#71887=CARTESIAN_POINT('',(1.,7.93725393319377,0.));
#71888=CARTESIAN_POINT('',(1.,8.,0.));
#71889=CARTESIAN_POINT('Origin',(0.,0.,0.));
#71890=CARTESIAN_POINT('Origin',(0.,0.,0.));
#71891=CARTESIAN_POINT('Origin',(0.,0.,0.));
#71892=CARTESIAN_POINT('Origin',(0.,0.,0.));
#71893=CARTESIAN_POINT('Origin',(0.,0.,1.));
#71894=CARTESIAN_POINT('Origin',(0.,0.,0.));
#71895=CARTESIAN_POINT('Origin',(0.,0.,1.));
#71896=CARTESIAN_POINT('Origin',(0.,0.,1.));
#71897=CARTESIAN_POINT('',(0.,0.,0.));
#71898=CARTESIAN_POINT('Origin',(0.,0.,24.4167025567876));
#71899=CARTESIAN_POINT('',(4.94636091871675,6.44535235552233,0.874940417221147));
#71900=CARTESIAN_POINT('',(4.94635496516529,6.4453438615057,0.708350185246763));
#71901=CARTESIAN_POINT('',(4.9467595481762,6.44587135576158,24.4167025567876));
#71902=CARTESIAN_POINT('',(2.10208451021607,-7.84862588447237,0.));
#71903=CARTESIAN_POINT('Ctrl Pts',(4.94635496517363,6.44534386149931,0.708350185246352));
#71904=CARTESIAN_POINT('Ctrl Pts',(5.44049095014118,6.06630505566983,0.683958258880921));
#71905=CARTESIAN_POINT('Ctrl Pts',(6.87015483931645,4.68667886721249,0.606635132002986));
#71906=CARTESIAN_POINT('Ctrl Pts',(8.32157346971745,1.57860155059824,0.476380804612548));
#71907=CARTESIAN_POINT('Ctrl Pts',(8.06280828226814,-2.59475929044894,0.317587203075035));
#71908=CARTESIAN_POINT('Ctrl Pts',(5.8384210982867,-6.13665782895719,0.158793601537515));
#71909=CARTESIAN_POINT('Ctrl Pts',(3.40721893572613,-7.4990738864542,0.0529312005125064));
#71910=CARTESIAN_POINT('Ctrl Pts',(2.10208451021607,-7.84862588447237,0.));
#71911=CARTESIAN_POINT('',(-2.10231583414457,-7.84925104679543,-1.60949812505473E-15));
#71912=CARTESIAN_POINT('Origin',(0.,0.,0.));
#71913=CARTESIAN_POINT('Ctrl Pts',(4.94636091871776,6.44535235552155,0.874940417221097));
#71914=CARTESIAN_POINT('Ctrl Pts',(5.54686650886728,5.98419136571353,0.845285016134203));
#71915=CARTESIAN_POINT('Ctrl Pts',(7.04180178671693,4.46845944575802,0.762698414534804));
#71916=CARTESIAN_POINT('Ctrl Pts',(8.38967733351479,1.16400612135573,0.6271806124229));
#71917=CARTESIAN_POINT('Ctrl Pts',(7.92408883944575,-2.99170878695321,0.46838701088538));
#71918=CARTESIAN_POINT('Ctrl Pts',(5.52703242316562,-6.41823535228475,0.309593409347865));
#71919=CARTESIAN_POINT('Ctrl Pts',(1.8455873829112,-8.24902208290505,0.153464405719403));
#71920=CARTESIAN_POINT('Ctrl Pts',(-0.863038767841767,-8.18056566201579,
0.0502666026034473));
#71921=CARTESIAN_POINT('Ctrl Pts',(-2.10231583414457,-7.84925104679543,
-1.60949812505473E-15));
#71922=CARTESIAN_POINT('Origin',(0.,0.,24.4167025567876));
#71923=CARTESIAN_POINT('',(4.9467595481762,6.44587135576158,2.87494842260025));
#71924=CARTESIAN_POINT('',(4.94675954817618,6.44587135576159,2.70835108074798));
#71925=CARTESIAN_POINT('',(4.9467595481762,6.44587135576158,24.4167025567876));
#71926=CARTESIAN_POINT('',(-8.12526511089558,-0.000106822124032805,1.4167025564899));
#71927=CARTESIAN_POINT('Ctrl Pts',(4.94675954817618,6.44587135576159,2.70835108074799));
#71928=CARTESIAN_POINT('Ctrl Pts',(5.00654996272257,6.39998635624443,2.70539779587792));
#71929=CARTESIAN_POINT('Ctrl Pts',(5.0656987513671,6.35327181669309,2.70244451100785));
#71930=CARTESIAN_POINT('Ctrl Pts',(5.12418284497226,6.30574640576292,2.69949122613778));
#71931=CARTESIAN_POINT('Ctrl Pts',(5.28700683250325,6.17343219108189,2.69126906538914));
#71932=CARTESIAN_POINT('Ctrl Pts',(5.44473011680673,6.03478622619136,2.68304690464051));
#71933=CARTESIAN_POINT('Ctrl Pts',(5.5968671918238,5.89022624349748,2.67482474389187));
#71934=CARTESIAN_POINT('Ctrl Pts',(5.74897622359167,5.74569290737622,2.66660409872451));
#71935=CARTESIAN_POINT('Ctrl Pts',(5.89550088736123,5.59524793238774,2.65838345355716));
#71936=CARTESIAN_POINT('Ctrl Pts',(6.03599120669964,5.43934717729477,2.6501628083898));
#71937=CARTESIAN_POINT('Ctrl Pts',(6.17646574291822,5.28346393657796,2.64194308675531));
#71938=CARTESIAN_POINT('Ctrl Pts',(6.31090709061718,5.12212635857307,2.63372336512082));
#71939=CARTESIAN_POINT('Ctrl Pts',(6.43890381653687,4.95582538068956,2.62550364348633));
#71940=CARTESIAN_POINT('Ctrl Pts',(6.56691079828585,4.78951107782118,2.61728326324077));
#71941=CARTESIAN_POINT('Ctrl Pts',(6.68847194429077,4.61823281266861,2.60906288299519));
#71942=CARTESIAN_POINT('Ctrl Pts',(6.80321698323602,4.44251350493264,2.60084250274963));
#71943=CARTESIAN_POINT('Ctrl Pts',(6.91796159749113,4.26679484756256,2.59262215292903));
#71944=CARTESIAN_POINT('Ctrl Pts',(7.02588999601499,4.0866354290706,2.58440180310845));
#71945=CARTESIAN_POINT('Ctrl Pts',(7.12667572325493,3.90258641135193,2.57618145328786));
#71946=CARTESIAN_POINT('Ctrl Pts',(7.22748299970096,3.71849804172979,2.56795934585716));
#71947=CARTESIAN_POINT('Ctrl Pts',(7.32114441204801,3.53051867034308,2.55973723842646));
#71948=CARTESIAN_POINT('Ctrl Pts',(7.4073793590196,3.33922425034175,2.55151513099576));
#71949=CARTESIAN_POINT('Ctrl Pts',(7.44519801229645,3.25533137862455,2.5479092955306));
#71950=CARTESIAN_POINT('Ctrl Pts',(7.48158894702567,3.17080121861856,2.54430346006544));
#71951=CARTESIAN_POINT('Ctrl Pts',(7.5165313868341,3.08568363142396,2.54069762460027));
#71952=CARTESIAN_POINT('Ctrl Pts',(7.59620841783576,2.89159539171117,2.53247546651058));
#71953=CARTESIAN_POINT('Ctrl Pts',(7.66837709955814,2.69438740193867,2.52425330842089));
#71954=CARTESIAN_POINT('Ctrl Pts',(7.73281095174109,2.49465876366551,2.51603115033119));
#71955=CARTESIAN_POINT('Ctrl Pts',(7.79723292682117,2.29496694140597,2.50781050783329));
#71956=CARTESIAN_POINT('Ctrl Pts',(7.8539228274159,2.09275567873303,2.49958986533539));
#71957=CARTESIAN_POINT('Ctrl Pts',(7.90270361351394,1.88864055856421,2.49136922283748));
#71958=CARTESIAN_POINT('Ctrl Pts',(7.9514789194125,1.68454836938245,2.48314950387452));
#71959=CARTESIAN_POINT('Ctrl Pts',(7.99234681613915,1.47855303665947,2.47492978491157));
#71960=CARTESIAN_POINT('Ctrl Pts',(8.02518089209509,1.27128250662546,2.46671006594861));
#71961=CARTESIAN_POINT('Ctrl Pts',(8.05801759897362,1.06399536845787,2.45848968835758));
#71962=CARTESIAN_POINT('Ctrl Pts',(8.08281914996309,0.855433119907242,2.45026931076654));
#71963=CARTESIAN_POINT('Ctrl Pts',(8.09951058010313,0.646232098628225,2.44204893317551));
#71964=CARTESIAN_POINT('Ctrl Pts',(8.11620194849499,0.437031851266314,2.4338285859949));
#71965=CARTESIAN_POINT('Ctrl Pts',(8.12478323524068,0.227193130324511,2.42560823881427));
#71966=CARTESIAN_POINT('Ctrl Pts',(8.12523146303619,0.0173561109345648,
2.41738789163366));
#71967=CARTESIAN_POINT('Ctrl Pts',(8.12567978667038,-0.192525775157294,
2.40916578680386));
#71968=CARTESIAN_POINT('Ctrl Pts',(8.11799157656876,-0.402405663767066,
2.40094368197406));
#71969=CARTESIAN_POINT('Ctrl Pts',(8.10219598212575,-0.611643547930737,
2.39272157714425));
#71970=CARTESIAN_POINT('Ctrl Pts',(8.09526873333835,-0.703406025410291,
2.38911572578376));
#71971=CARTESIAN_POINT('Ctrl Pts',(8.08678285649728,-0.795045059485583,
2.38550987442326));
#71972=CARTESIAN_POINT('Ctrl Pts',(8.0767439624085,-0.886506925070441,2.38190402306276));
#71973=CARTESIAN_POINT('Ctrl Pts',(8.05385299354372,-1.09506084534311,2.37368185929709));
#71974=CARTESIAN_POINT('Ctrl Pts',(8.0228761563586,-1.30276208569347,2.36545969553142));
#71975=CARTESIAN_POINT('Ctrl Pts',(7.98390120047228,-1.50897620378761,2.35723753176575));
#71976=CARTESIAN_POINT('Ctrl Pts',(7.94493342875514,-1.71515231088016,2.34901688357372));
#71977=CARTESIAN_POINT('Ctrl Pts',(7.89797053557262,-1.91984155295615,2.34079623538168));
#71978=CARTESIAN_POINT('Ctrl Pts',(7.84315157048059,-2.12241866863442,2.33257558718965));
#71979=CARTESIAN_POINT('Ctrl Pts',(7.78833876393394,-2.32497302612382,2.32435586253265));
#71980=CARTESIAN_POINT('Ctrl Pts',(7.72567172454593,-2.52541544615141,2.31613613787566));
#71981=CARTESIAN_POINT('Ctrl Pts',(7.65533987497481,-2.72313403289677,2.30791641321866));
#71982=CARTESIAN_POINT('Ctrl Pts',(7.58500239023559,-2.9208684613622,2.29969602997624));
#71983=CARTESIAN_POINT('Ctrl Pts',(7.50699896457821,-3.11587834148089,2.29147564673383));
#71984=CARTESIAN_POINT('Ctrl Pts',(7.4215682120023,-3.30756902227254,2.28325526349142));
#71985=CARTESIAN_POINT('Ctrl Pts',(7.33613777583018,-3.49925899311308,2.27503491069425));
#71986=CARTESIAN_POINT('Ctrl Pts',(7.24328019034877,-3.68762952072127,2.26681455789709));
#71987=CARTESIAN_POINT('Ctrl Pts',(7.14328155724583,-3.87210745672321,2.25859420509993));
#71988=CARTESIAN_POINT('Ctrl Pts',(7.04326154383628,-4.05662483521265,2.25037209474211));
#71989=CARTESIAN_POINT('Ctrl Pts',(6.93609757323777,-4.23724769987652,2.24214998438428));
#71990=CARTESIAN_POINT('Ctrl Pts',(6.82212144050659,-4.41342798893108,2.23392787402646));
#71991=CARTESIAN_POINT('Ctrl Pts',(6.77213705497226,-4.49069209046385,2.23032205652605));
#71992=CARTESIAN_POINT('Ctrl Pts',(6.72084308082629,-4.56710211611093,2.22671623902564));
#71993=CARTESIAN_POINT('Ctrl Pts',(6.66827014779923,-4.64261357410561,2.22311042152523));
#71994=CARTESIAN_POINT('Ctrl Pts',(6.54839087633042,-4.81479834772838,2.21488826707978));
#71995=CARTESIAN_POINT('Ctrl Pts',(6.42181915258924,-4.98236585834492,2.20666611263434));
#71996=CARTESIAN_POINT('Ctrl Pts',(6.28893556637754,-5.14480096840019,2.19844395818889));
#71997=CARTESIAN_POINT('Ctrl Pts',(6.15607647469026,-5.30720613667798,2.19022331933892));
#71998=CARTESIAN_POINT('Ctrl Pts',(6.01690802944503,-5.46448056427156,2.18200268048895));
#71999=CARTESIAN_POINT('Ctrl Pts',(5.87185147584527,-5.61614171901971,2.17378204163899));
#72000=CARTESIAN_POINT('Ctrl Pts',(5.72681121825511,-5.76778583578114,2.16556232631578));
#72001=CARTESIAN_POINT('Ctrl Pts',(5.57588437683982,-5.91381772545637,2.15734261099258));
#72002=CARTESIAN_POINT('Ctrl Pts',(5.41953003628161,-6.05379069247868,2.14912289566938));
#72003=CARTESIAN_POINT('Ctrl Pts',(5.26316316664825,-6.19377487589456,2.14090252167926));
#72004=CARTESIAN_POINT('Ctrl Pts',(5.10136814694562,-6.32769896764435,2.13268214768914));
#72005=CARTESIAN_POINT('Ctrl Pts',(4.9346390076379,-6.45515494986746,2.12446177369903));
#72006=CARTESIAN_POINT('Ctrl Pts',(4.76791048454023,-6.58261046102921,2.11624143009039));
#72007=CARTESIAN_POINT('Ctrl Pts',(4.59624811441685,-6.70359773335699,2.10802108648175));
#72008=CARTESIAN_POINT('Ctrl Pts',(4.42017734043375,-6.8177503504907,2.09980074287311));
#72009=CARTESIAN_POINT('Ctrl Pts',(4.24406891810606,-6.93192737631511,2.09157864154896));
#72010=CARTESIAN_POINT('Ctrl Pts',(4.06355045643346,-7.03926666671835,2.08335654022482));
#72011=CARTESIAN_POINT('Ctrl Pts',(3.87917552096256,-7.13944569557503,2.07513443890068));
#72012=CARTESIAN_POINT('Ctrl Pts',(3.79831631354934,-7.1833800668717,2.07152856592969));
#72013=CARTESIAN_POINT('Ctrl Pts',(3.71671571368778,-7.2259378643607,2.06792269295871));
#72014=CARTESIAN_POINT('Ctrl Pts',(3.63442190659676,-7.26709467169305,2.06431681998772));
#72015=CARTESIAN_POINT('Ctrl Pts',(3.44677435505551,-7.36094103022438,2.05609465530618));
#72016=CARTESIAN_POINT('Ctrl Pts',(3.2554590105286,-7.44753096748448,2.04787249062462));
#72017=CARTESIAN_POINT('Ctrl Pts',(3.06105653712331,-7.52659421245989,2.03965032594308));
#72018=CARTESIAN_POINT('Ctrl Pts',(2.86668989789977,-7.60564288371799,2.03142967685204));
#72019=CARTESIAN_POINT('Ctrl Pts',(2.66923753880226,-7.67716752060457,2.02320902776101));
#72020=CARTESIAN_POINT('Ctrl Pts',(2.46930022512807,-7.74094593448905,2.01498837866997));
#72021=CARTESIAN_POINT('Ctrl Pts',(2.26938537354817,-7.80471718314398,2.00676865313337));
#72022=CARTESIAN_POINT('Ctrl Pts',(2.06698640581499,-7.86074385653922,1.99854892759678));
#72023=CARTESIAN_POINT('Ctrl Pts',(1.8627201697933,-7.90885333860385,1.99032920206018));
#72024=CARTESIAN_POINT('Ctrl Pts',(1.65843756831291,-7.95696667511725,1.98210881797335));
#72025=CARTESIAN_POINT('Ctrl Pts',(1.4522876862897,-7.99716148256033,1.97388843388651));
#72026=CARTESIAN_POINT('Ctrl Pts',(1.24489955385584,-8.0293158278467,1.96566804979968));
#72027=CARTESIAN_POINT('Ctrl Pts',(1.03751219006002,-8.06147005396013,1.95744769617988));
#72028=CARTESIAN_POINT('Ctrl Pts',(0.828886877101282,-8.08558383494591,
1.94922734256007));
#72029=CARTESIAN_POINT('Ctrl Pts',(0.619660326089502,-8.10158679782983,
1.94100698894027));
#72030=CARTESIAN_POINT('Ctrl Pts',(0.410389042151422,-8.11759318216938,
1.93278487779747));
#72031=CARTESIAN_POINT('Ctrl Pts',(0.200516557694702,-8.12548526149068,
1.92456276665469));
#72032=CARTESIAN_POINT('Ctrl Pts',(-0.00931671950940989,-8.12524465854645,
1.9163406555119));
#72033=CARTESIAN_POINT('Ctrl Pts',(-0.101339243902614,-8.12513914196395,
1.912734843158));
#72034=CARTESIAN_POINT('Ctrl Pts',(-0.193354211646623,-8.12347016864793,
1.90912903080411));
#72035=CARTESIAN_POINT('Ctrl Pts',(-0.285307631331966,-8.12023935102924,
1.90552321845021));
#72036=CARTESIAN_POINT('Ctrl Pts',(-0.494984716518033,-8.11287226861541,
1.89730105306821));
#72037=CARTESIAN_POINT('Ctrl Pts',(-0.70441090320622,-8.09737835170293,
1.88907888768622));
#72038=CARTESIAN_POINT('Ctrl Pts',(-0.91294698938132,-8.07379807507468,
1.88085672230422));
#72039=CARTESIAN_POINT('Ctrl Pts',(-1.12144463783091,-8.05022214480305,
1.87263607244571));
#72040=CARTESIAN_POINT('Ctrl Pts',(-1.32905222009258,-8.01856286277639,
1.8644154225872));
#72041=CARTESIAN_POINT('Ctrl Pts',(-1.53513588680306,-7.97891254316961,
1.8561947727287));
#72042=CARTESIAN_POINT('Ctrl Pts',(-1.74119640250264,-7.93926667779735,
1.84797504636091));
#72043=CARTESIAN_POINT('Ctrl Pts',(-1.94573305471411,-7.89163162277346,
1.83975531999312));
#72044=CARTESIAN_POINT('Ctrl Pts',(-2.14812158852616,-7.83615091760029,
1.83153559362534));
#72045=CARTESIAN_POINT('Ctrl Pts',(-2.35052633952146,-7.78066576681577,
1.8233152086194));
#72046=CARTESIAN_POINT('Ctrl Pts',(-2.5507823428187,-7.71733378514711,1.81509482361347));
#72047=CARTESIAN_POINT('Ctrl Pts',(-2.74827889416591,-7.64634884650067,
1.80687443860754));
#72048=CARTESIAN_POINT('Ctrl Pts',(-2.94577471470873,-7.57536417052265,
1.79865408401983));
#72049=CARTESIAN_POINT('Ctrl Pts',(-3.14051082688264,-7.49672669655549,
1.79043372943212));
#72050=CARTESIAN_POINT('Ctrl Pts',(-3.33189444944503,-7.41067924958687,
1.78221337484441));
#72051=CARTESIAN_POINT('Ctrl Pts',(-3.52331899161975,-7.32461340486757,
1.77399126266783));
#72052=CARTESIAN_POINT('Ctrl Pts',(-3.71138934292691,-7.23113454303285,
1.76576915049127));
#72053=CARTESIAN_POINT('Ctrl Pts',(-3.89553435227035,-7.13053291646435,
1.75754703831469));
#72054=CARTESIAN_POINT('Ctrl Pts',(-3.97629114251125,-7.08641407510312,
1.7539412311807));
#72055=CARTESIAN_POINT('Ctrl Pts',(-4.05629329600876,-7.04092594081101,
1.7503354240467));
#72056=CARTESIAN_POINT('Ctrl Pts',(-4.13549417314262,-6.9940957604542,1.7467296169127));
#72057=CARTESIAN_POINT('Ctrl Pts',(-4.31609156993985,-6.88731148015273,
1.73850749355601));
#72058=CARTESIAN_POINT('Ctrl Pts',(-4.49258058326739,-6.77351091743634,
1.73028537019933));
#72059=CARTESIAN_POINT('Ctrl Pts',(-4.66441928172336,-6.65303542203011,
1.72206324684263));
#72060=CARTESIAN_POINT('Ctrl Pts',(-4.83622630117851,-6.53258213665777,
1.71384263926006));
#72061=CARTESIAN_POINT('Ctrl Pts',(-5.00338447526566,-6.40545654394141,
1.70562203167748));
#72062=CARTESIAN_POINT('Ctrl Pts',(-5.16538137421267,-6.27204295436796,
1.69740142409492));
#72063=CARTESIAN_POINT('Ctrl Pts',(-5.32736007243909,-6.13864435411519,
1.68918174011634));
#72064=CARTESIAN_POINT('Ctrl Pts',(-5.48417842547541,-5.99895935498211,
1.68096205613776));
#72065=CARTESIAN_POINT('Ctrl Pts',(-5.63535693628535,-5.85341265956541,
1.67274237215917));
#72066=CARTESIAN_POINT('Ctrl Pts',(-5.78654756365206,-5.70785429896699,
1.66452202939472));
#72067=CARTESIAN_POINT('Ctrl Pts',(-5.93209723108903,-5.5564335061223,1.65630168663026));
#72068=CARTESIAN_POINT('Ctrl Pts',(-6.07156242213258,-5.39961270061543,
1.6480813438658));
#72069=CARTESIAN_POINT('Ctrl Pts',(-6.21102709986354,-5.24279247229988,
1.63986103135696));
#72070=CARTESIAN_POINT('Ctrl Pts',(-6.34440715185304,-5.08057249340363,
1.63164071884812));
#72071=CARTESIAN_POINT('Ctrl Pts',(-6.47129821992731,-4.91344959384602,
1.62342040633928));
#72072=CARTESIAN_POINT('Ctrl Pts',(-6.59821642662373,-4.74629095114831,
1.61519833572439));
#72073=CARTESIAN_POINT('Ctrl Pts',(-6.71864269829153,-4.57422752799915,
1.60697626510949));
#72074=CARTESIAN_POINT('Ctrl Pts',(-6.83221436141168,-4.39778745305181,
1.59875419449459));
#72075=CARTESIAN_POINT('Ctrl Pts',(-6.88202495260671,-4.32040385046845,
1.59514813478812));
#72076=CARTESIAN_POINT('Ctrl Pts',(-6.93051758438691,-4.24217875673097,
1.59154207508164));
#72077=CARTESIAN_POINT('Ctrl Pts',(-6.97766433109251,-4.16315842181141,
1.58793601537516));
#72078=CARTESIAN_POINT('Ctrl Pts',(-7.0851647931161,-3.98298220379674,1.57971374954309));
#72079=CARTESIAN_POINT('Ctrl Pts',(-7.18570052831571,-3.79861025402686,
1.57149148371102));
#72080=CARTESIAN_POINT('Ctrl Pts',(-7.27895895856883,-3.61060161773223,
1.56326921787894));
#72081=CARTESIAN_POINT('Ctrl Pts',(-7.37220020351639,-3.42262762694744,
1.55504846721446));
#72082=CARTESIAN_POINT('Ctrl Pts',(-7.45816668895786,-3.23101855143005,
1.54682771654997));
#72083=CARTESIAN_POINT('Ctrl Pts',(-7.53659229682653,-3.03635704651397,
1.53860696588548));
#72084=CARTESIAN_POINT('Ctrl Pts',(-7.61500909493637,-2.84171740844671,
1.53038713867996));
#72085=CARTESIAN_POINT('Ctrl Pts',(-7.68588659637947,-2.64402629917056,
1.52216731147444));
#72086=CARTESIAN_POINT('Ctrl Pts',(-7.74900692705355,-2.4438860871522,1.51394748426891));
#72087=CARTESIAN_POINT('Ctrl Pts',(-7.81213231003214,-2.24372985542539,
1.50572699912847));
#72088=CARTESIAN_POINT('Ctrl Pts',(-7.86749919024205,-2.04112440991499,
1.49750651398802));
#72089=CARTESIAN_POINT('Ctrl Pts',(-7.91493933402158,-1.8366880250217,1.48928602884758));
#72090=CARTESIAN_POINT('Ctrl Pts',(-7.9623792988666,-1.63225241122055,1.48106557471312));
#72091=CARTESIAN_POINT('Ctrl Pts',(-8.00189252297233,-1.42598615994298,
1.47284512057865));
#72092=CARTESIAN_POINT('Ctrl Pts',(-8.03336162146412,-1.21851902787254,
1.46462466644419));
#72093=CARTESIAN_POINT('Ctrl Pts',(-8.06483744242478,-1.01100757640927,
1.45640245624585));
#72094=CARTESIAN_POINT('Ctrl Pts',(-8.08826566048024,-0.802295023498583,
1.44818024604752));
#72095=CARTESIAN_POINT('Ctrl Pts',(-8.10358046933688,-0.593018667060264,
1.43995803584918));
#72096=CARTESIAN_POINT('Ctrl Pts',(-8.11029558120164,-0.501256885552666,
1.436352828512));
#72097=CARTESIAN_POINT('Ctrl Pts',(-8.11545150101203,-0.409386774614503,
1.43274762117482));
#72098=CARTESIAN_POINT('Ctrl Pts',(-8.11904583497314,-0.317462268789904,
1.42914241383765));
#72099=CARTESIAN_POINT('Ctrl Pts',(-8.12317994770551,-0.211733008777547,
1.42499579482097));
#72100=CARTESIAN_POINT('Ctrl Pts',(-8.12524860804669,-0.105922731453665,
1.42084917580429));
#72101=CARTESIAN_POINT('Ctrl Pts',(-8.12524999929771,-0.000106829522945291,
1.41670255678761));
#72102=CARTESIAN_POINT('Ctrl Pts',(-8.12583419228576,-0.000106543491459244,
1.4167025452787));
#72103=CARTESIAN_POINT('Ctrl Pts',(-8.12502534027835,1.24489697938662,1.36791796761918));
#72104=CARTESIAN_POINT('Ctrl Pts',(-7.51929797608287,3.84148931606845,1.26620218944715));
#72105=CARTESIAN_POINT('Ctrl Pts',(-4.86711214124423,6.93200738973815,1.11155521076262));
#72106=CARTESIAN_POINT('Ctrl Pts',(-0.95745427596839,8.41576571390258,0.9527616092251));
#72107=CARTESIAN_POINT('Ctrl Pts',(2.54915990794148,7.93533015430886,0.818359934053017));
#72108=CARTESIAN_POINT('Ctrl Pts',(4.36820127080559,6.88883045742807,0.736889459393433));
#72109=CARTESIAN_POINT('Ctrl Pts',(4.94635496517363,6.44534386149931,0.708350185246352));
#72110=CARTESIAN_POINT('',(-8.12531588310525,3.02062580826617E-5,1.58329744321239));
#72111=CARTESIAN_POINT('Ctrl Pts',(-8.12593926228046,3.02085755239396E-5,
1.58329744321239));
#72112=CARTESIAN_POINT('Ctrl Pts',(-8.12594527009992,0.0285713546895934,
1.58217903602426));
#72113=CARTESIAN_POINT('Ctrl Pts',(-8.11883025624699,1.40788508355762,1.52812942832363));
#72114=CARTESIAN_POINT('Ctrl Pts',(-7.39463807035817,4.13048620871564,1.42114862011048));
#72115=CARTESIAN_POINT('Ctrl Pts',(-4.51728121963489,7.16489725681085,1.26235501857297));
#72116=CARTESIAN_POINT('Ctrl Pts',(-0.538848536700319,8.45288342237417,
1.10356141703545));
#72117=CARTESIAN_POINT('Ctrl Pts',(2.8034090240862,7.82474427555336,0.974423216584827));
#72118=CARTESIAN_POINT('Ctrl Pts',(4.47503875958309,6.80730634394467,0.898216216646709));
#72119=CARTESIAN_POINT('Ctrl Pts',(4.94636091871776,6.44535235552155,0.874940417221097));
#72120=CARTESIAN_POINT('Ctrl Pts',(4.94675954817621,6.44587135576157,2.87494842260024));
#72121=CARTESIAN_POINT('Ctrl Pts',(5.11318684010766,6.3181499430928,2.86672929304954));
#72122=CARTESIAN_POINT('Ctrl Pts',(5.2746458763742,6.18399423460548,2.85851016349884));
#72123=CARTESIAN_POINT('Ctrl Pts',(5.43064894709995,6.04381829441142,2.85029103394814));
#72124=CARTESIAN_POINT('Ctrl Pts',(5.58670953802513,5.9035906696704,2.842068873906));
#72125=CARTESIAN_POINT('Ctrl Pts',(5.73736164193147,5.75729209116024,2.83384671386386));
#72126=CARTESIAN_POINT('Ctrl Pts',(5.88214107051609,5.60536385875599,2.82562455382172));
#72127=CARTESIAN_POINT('Ctrl Pts',(6.02689381201688,5.45346363116923,2.81740390936419));
#72128=CARTESIAN_POINT('Ctrl Pts',(6.1657758352205,5.29593603437041,2.80918326490666));
#72129=CARTESIAN_POINT('Ctrl Pts',(6.29836032883316,5.13325868534605,2.80096262044913));
#72130=CARTESIAN_POINT('Ctrl Pts',(6.43092992747311,4.97059961202352,2.79274289952551));
#72131=CARTESIAN_POINT('Ctrl Pts',(6.55720322257782,4.80279217018242,2.78452317860188));
#72132=CARTESIAN_POINT('Ctrl Pts',(6.67679363853073,4.63034710048561,2.77630345767825));
#72133=CARTESIAN_POINT('Ctrl Pts',(6.79639363680517,4.45788821342652,2.7680830781399));
#72134=CARTESIAN_POINT('Ctrl Pts',(6.90930951555532,4.28079119700873,2.75986269860155));
#72135=CARTESIAN_POINT('Ctrl Pts',(7.01519739680621,4.09959669313255,2.7516423190632));
#72136=CARTESIAN_POINT('Ctrl Pts',(7.12108488619231,3.9184028598123,2.74342196994644));
#72137=CARTESIAN_POINT('Ctrl Pts',(7.21994428349637,3.73311182553568,2.73520162082968));
#72138=CARTESIAN_POINT('Ctrl Pts',(7.31147687342435,3.54429026631298,2.72698127171291));
#72139=CARTESIAN_POINT('Ctrl Pts',(7.40302903423637,3.35542833453178,2.71875916497627));
#72140=CARTESIAN_POINT('Ctrl Pts',(7.4872511292024,3.16303463535269,2.71053705823964));
#72141=CARTESIAN_POINT('Ctrl Pts',(7.56389147054215,2.96769833109091,2.70231495150299));
#72142=CARTESIAN_POINT('Ctrl Pts',(7.59750241650546,2.88203276838012,2.69870911180553));
#72143=CARTESIAN_POINT('Ctrl Pts',(7.62965578754156,2.79580151722597,2.69510327210807));
#72144=CARTESIAN_POINT('Ctrl Pts',(7.66033330596529,2.70905540807473,2.69149743241061));
#72145=CARTESIAN_POINT('Ctrl Pts',(7.73028524070325,2.51125394048837,2.68327527246571));
#72146=CARTESIAN_POINT('Ctrl Pts',(7.79258332089186,2.31070898626016,2.67505311252082));
#72147=CARTESIAN_POINT('Ctrl Pts',(7.84703106126773,2.10803014352249,2.66683095257592));
#72148=CARTESIAN_POINT('Ctrl Pts',(7.90146876533037,1.90538866043161,2.65861030821591));
#72149=CARTESIAN_POINT('Ctrl Pts',(7.94805894115351,1.70061435877334,2.65038966385591));
#72150=CARTESIAN_POINT('Ctrl Pts',(7.98665530036555,1.49433084544318,2.6421690194959));
#72151=CARTESIAN_POINT('Ctrl Pts',(8.02524732353679,1.28807050667525,2.63394929866988));
#72152=CARTESIAN_POINT('Ctrl Pts',(8.05584726873433,1.08030158472424,2.62572957784385));
#72153=CARTESIAN_POINT('Ctrl Pts',(8.0783600269179,0.871657523339884,2.61750985701782));
#72154=CARTESIAN_POINT('Ctrl Pts',(8.10087458896488,0.662996744084499,2.6092894775762));
#72155=CARTESIAN_POINT('Ctrl Pts',(8.11530063485901,0.453460978442835,2.60106909813458));
#72156=CARTESIAN_POINT('Ctrl Pts',(8.12159485509865,0.243689499435362,2.59284871869296));
#72157=CARTESIAN_POINT('Ctrl Pts',(8.1278890520454,0.0339187967250488,2.58462836967234));
#72158=CARTESIAN_POINT('Ctrl Pts',(8.12605147735175,-0.176087322514969,
2.57640802065172));
#72159=CARTESIAN_POINT('Ctrl Pts',(8.11609093552446,-0.38568833116607,2.56818767163109));
#72160=CARTESIAN_POINT('Ctrl Pts',(8.10612826399912,-0.595334155337057,
2.55996556498908));
#72161=CARTESIAN_POINT('Ctrl Pts',(8.08803916956429,-0.804574401001969,
2.55174345834707));
#72162=CARTESIAN_POINT('Ctrl Pts',(8.06188451092087,-1.0127712945548,2.54352135170506));
#72163=CARTESIAN_POINT('Ctrl Pts',(8.05041427273469,-1.10407693884677,2.53991551142774));
#72164=CARTESIAN_POINT('Ctrl Pts',(8.03739345750648,-1.19518198281216,2.53630967115042));
#72165=CARTESIAN_POINT('Ctrl Pts',(8.02283033388594,-1.28603304630154,2.5327038308731));
#72166=CARTESIAN_POINT('Ctrl Pts',(7.98962300227551,-1.49319474258745,2.52448167078277));
#72167=CARTESIAN_POINT('Ctrl Pts',(7.94838205632125,-1.69910374035563,2.51625951069245));
#72168=CARTESIAN_POINT('Ctrl Pts',(7.89922660659719,-1.90313073122343,2.50803735060213));
#72169=CARTESIAN_POINT('Ctrl Pts',(7.85008021766045,-2.10712011394843,2.49981670609643));
#72170=CARTESIAN_POINT('Ctrl Pts',(7.793022305761,-2.30922789536695,2.49159606159073));
#72171=CARTESIAN_POINT('Ctrl Pts',(7.72822276287901,-2.50883648128345,2.48337541708503));
#72172=CARTESIAN_POINT('Ctrl Pts',(7.66343049978985,-2.70842264251782,2.47515569611346));
#72173=CARTESIAN_POINT('Ctrl Pts',(7.59089843314881,-2.90550988817235,2.46693597514187));
#72174=CARTESIAN_POINT('Ctrl Pts',(7.51084610308596,-3.09949647172866,2.4587162541703));
#72175=CARTESIAN_POINT('Ctrl Pts',(7.43078735874187,-3.29349859867395,2.45049587458451));
#72176=CARTESIAN_POINT('Ctrl Pts',(7.3432072570489,-3.48439929322881,2.44227549499874));
#72177=CARTESIAN_POINT('Ctrl Pts',(7.24837361356307,-3.67161647244134,2.43405511541295));
#72178=CARTESIAN_POINT('Ctrl Pts',(7.15354032103805,-3.85883295879963,2.42583476624919));
#72179=CARTESIAN_POINT('Ctrl Pts',(7.05145367616815,-4.04236569499885,2.41761441708542));
#72180=CARTESIAN_POINT('Ctrl Pts',(6.94242785718441,-4.22165642968372,2.40939406792166));
#72181=CARTESIAN_POINT('Ctrl Pts',(6.83337872704452,-4.40098549908922,2.40117196113897));
#72182=CARTESIAN_POINT('Ctrl Pts',(6.71738761205256,-4.57607050274914,2.39294985435627));
#72183=CARTESIAN_POINT('Ctrl Pts',(6.59481308323288,-4.74638051147613,2.38472774757358));
#72184=CARTESIAN_POINT('Ctrl Pts',(6.54105750954748,-4.82107068007513,2.38112190816092));
#72185=CARTESIAN_POINT('Ctrl Pts',(6.48603630710692,-4.89484285566418,2.37751606874826));
#72186=CARTESIAN_POINT('Ctrl Pts',(6.42978227541665,-4.96765411972672,2.3739102293356));
#72187=CARTESIAN_POINT('Ctrl Pts',(6.30150988326345,-5.13368088681117,2.36568806937151));
#72188=CARTESIAN_POINT('Ctrl Pts',(6.16678229109025,-5.29476411247359,2.35746590940743));
#72189=CARTESIAN_POINT('Ctrl Pts',(6.02600517238921,-5.45040817048031,2.34924374944334));
#72190=CARTESIAN_POINT('Ctrl Pts',(5.88525400302796,-5.60602353873556,2.34102310506378));
#72191=CARTESIAN_POINT('Ctrl Pts',(5.7384557306157,-5.75620152160216,2.33280246068421));
#72192=CARTESIAN_POINT('Ctrl Pts',(5.58605501672273,-5.90048107467915,2.32458181630465));
#72193=CARTESIAN_POINT('Ctrl Pts',(5.4336714240135,-6.04474441892959,2.31636209545858));
#72194=CARTESIAN_POINT('Ctrl Pts',(5.27568686061463,-6.18311045349229,2.30814237461251));
#72195=CARTESIAN_POINT('Ctrl Pts',(5.11258200345081,-6.31515580334253,2.29992265376643));
#72196=CARTESIAN_POINT('Ctrl Pts',(4.94946407729784,-6.44721173349845,2.29170227430452));
#72197=CARTESIAN_POINT('Ctrl Pts',(4.78122526530201,-6.57294577915914,2.28348189484261));
#72198=CARTESIAN_POINT('Ctrl Pts',(4.60837922868544,-6.69197492875762,2.2752615153807));
#72199=CARTESIAN_POINT('Ctrl Pts',(4.43553383171244,-6.81100363787027,2.26704116633957));
#72200=CARTESIAN_POINT('Ctrl Pts',(4.25808148881973,-6.92332733535738,2.25882081729844));
#72201=CARTESIAN_POINT('Ctrl Pts',(4.07656517178318,-7.02860611805103,2.25060046825732));
#72202=CARTESIAN_POINT('Ctrl Pts',(3.89501004410986,-7.13390741076836,2.2423783615947));
#72203=CARTESIAN_POINT('Ctrl Pts',(3.70938946169537,-7.23216063129356,2.23415625493207));
#72204=CARTESIAN_POINT('Ctrl Pts',(3.52027230707397,-7.32307110757147,2.22593414826945));
#72205=CARTESIAN_POINT('Ctrl Pts',(3.43733416743192,-7.36294028703093,2.22232830811232));
#72206=CARTESIAN_POINT('Ctrl Pts',(3.35372384018368,-7.40139783865352,2.21872246795519));
#72207=CARTESIAN_POINT('Ctrl Pts',(3.2694906609304,-7.43842176678554,2.21511662779806));
#72208=CARTESIAN_POINT('Ctrl Pts',(3.07741928968188,-7.52284499179453,2.20689446796006));
#72209=CARTESIAN_POINT('Ctrl Pts',(2.88204457163584,-7.59983880869683,2.19867230812206));
#72210=CARTESIAN_POINT('Ctrl Pts',(2.6839598612744,-7.66916208105996,2.19045014828406));
#72211=CARTESIAN_POINT('Ctrl Pts',(2.48591166375443,-7.7384725751039,2.18222950403209));
#72212=CARTESIAN_POINT('Ctrl Pts',(2.28515474935039,-7.80011524912847,2.17400885978011));
#72213=CARTESIAN_POINT('Ctrl Pts',(2.0823001640475,-7.85389798694303,2.16578821552814));
#72214=CARTESIAN_POINT('Ctrl Pts',(1.8794683681093,-7.90767468262437,2.15756849481092));
#72215=CARTESIAN_POINT('Ctrl Pts',(1.67453965692389,-7.95359312935804,2.1493487740937));
#72216=CARTESIAN_POINT('Ctrl Pts',(1.46813868038228,-7.99151152021102,2.14112905337648));
#72217=CARTESIAN_POINT('Ctrl Pts',(1.26172116570797,-8.0294329493218,2.13290867404401));
#72218=CARTESIAN_POINT('Ctrl Pts',(1.05383143976939,-8.05935298572509,2.12468829471154));
#72219=CARTESIAN_POINT('Ctrl Pts',(0.845103805785858,-8.08118104734365,
2.11646791537907));
#72220=CARTESIAN_POINT('Ctrl Pts',(0.636376944235713,-8.10300902818362,
2.10824756646755));
#72221=CARTESIAN_POINT('Ctrl Pts',(0.426812474664166,-8.11674506609866,
2.10002721755604));
#72222=CARTESIAN_POINT('Ctrl Pts',(0.217049814348368,-8.12235045664685,
2.09180686864453));
#72223=CARTESIAN_POINT('Ctrl Pts',(0.00724230392923697,-8.12795704570361,
2.08358476211087));
#72224=CARTESIAN_POINT('Ctrl Pts',(-0.202763186794446,-8.12542950643695,
2.0753626555772));
#72225=CARTESIAN_POINT('Ctrl Pts',(-0.412326127505104,-8.11478124949013,
2.06714054904354));
#72226=CARTESIAN_POINT('Ctrl Pts',(-0.504230875448006,-8.11011140964436,
2.06353470811588));
#72227=CARTESIAN_POINT('Ctrl Pts',(-0.596050525226838,-8.10388038764368,
2.05992886718822));
#72228=CARTESIAN_POINT('Ctrl Pts',(-0.687731230561746,-8.09609247211332,
2.05632302626055));
#72229=CARTESIAN_POINT('Ctrl Pts',(-0.896784683851678,-8.07833420302493,
2.04810086549959));
#72230=CARTESIAN_POINT('Ctrl Pts',(-1.1051844479233,-8.05247155703697,2.03987870473862));
#72231=CARTESIAN_POINT('Ctrl Pts',(-1.31229411584146,-8.01857666397397,
2.03165654397766));
#72232=CARTESIAN_POINT('Ctrl Pts',(-1.51936560747801,-7.98468801871676,
2.02343589879792));
#72233=CARTESIAN_POINT('Ctrl Pts',(-1.72514718645945,-7.94277012905113,
2.01521525361819));
#72234=CARTESIAN_POINT('Ctrl Pts',(-1.92901036318679,-7.89294663488978,
2.00699460843845));
#72235=CARTESIAN_POINT('Ctrl Pts',(-2.13285063729275,-7.84312873805426,
1.99877488679148));
#72236=CARTESIAN_POINT('Ctrl Pts',(-2.33477265282164,-7.78540707987436,
1.99055516514452));
#72237=CARTESIAN_POINT('Ctrl Pts',(-2.53416004363824,-7.71995598664445,
1.98233544349755));
#72238=CARTESIAN_POINT('Ctrl Pts',(-2.7335634105079,-7.65449964910027,1.97411506323968));
#72239=CARTESIAN_POINT('Ctrl Pts',(-2.93043146559177,-7.58131272849055,
1.96589468298181));
#72240=CARTESIAN_POINT('Ctrl Pts',(-3.12416387337227,-7.50061915143114,
1.95767430272394));
#72241=CARTESIAN_POINT('Ctrl Pts',(-3.3178955641178,-7.41992587303171,1.94945395289103));
#72242=CARTESIAN_POINT('Ctrl Pts',(-3.5084913593472,-7.33172610970674,1.94123360305811));
#72243=CARTESIAN_POINT('Ctrl Pts',(-3.69537125251977,-7.23629178989836,
1.9330132532252));
#72244=CARTESIAN_POINT('Ctrl Pts',(-3.88229110286499,-7.14083706508264,
1.92479114578246));
#72245=CARTESIAN_POINT('Ctrl Pts',(-4.06549320098115,-7.038144827766,1.91656903833971));
#72246=CARTESIAN_POINT('Ctrl Pts',(-4.2444214963054,-6.92853330252519,1.90834693089697));
#72247=CARTESIAN_POINT('Ctrl Pts',(-4.32289115682492,-6.88046276589438,
1.90474109550566));
#72248=CARTESIAN_POINT('Ctrl Pts',(-4.40053917807562,-6.83106203178722,
1.90113526011435));
#72249=CARTESIAN_POINT('Ctrl Pts',(-4.47732032824069,-6.78036062763793,
1.89752942472304));
#72250=CARTESIAN_POINT('Ctrl Pts',(-4.65239952191805,-6.66474942700232,
1.88930726666098));
#72251=CARTESIAN_POINT('Ctrl Pts',(-4.82302732827707,-6.54233430842207,
1.88108510859891));
#72252=CARTESIAN_POINT('Ctrl Pts',(-4.98867941096454,-6.4134830862113,1.87286295053685));
#72253=CARTESIAN_POINT('Ctrl Pts',(-5.15430095897274,-6.28465561517034,
1.86464230806672));
#72254=CARTESIAN_POINT('Ctrl Pts',(-5.31494838101878,-6.14939458944456,
1.85642166559659));
#72255=CARTESIAN_POINT('Ctrl Pts',(-5.47012893708334,-6.00810926782989,
1.84820102312646));
#72256=CARTESIAN_POINT('Ctrl Pts',(-5.62529205963782,-5.86683981868753,
1.83998130419119));
#72257=CARTESIAN_POINT('Ctrl Pts',(-5.77498932419644,-5.71954762343952,
1.83176158525592));
#72258=CARTESIAN_POINT('Ctrl Pts',(-5.918762886503,-5.56668064970991,1.82354186632065));
#72259=CARTESIAN_POINT('Ctrl Pts',(-6.06254796907189,-5.4138014270827,1.8153214887572));
#72260=CARTESIAN_POINT('Ctrl Pts',(-6.20040819678272,-5.25534674656431,
1.80710111119376));
#72261=CARTESIAN_POINT('Ctrl Pts',(-6.33192353251545,-5.09180046161249,
1.79888073363031));
#72262=CARTESIAN_POINT('Ctrl Pts',(-6.46343838172507,-4.92825478167791,
1.79066038647704));
#72263=CARTESIAN_POINT('Ctrl Pts',(-6.58860820303355,-4.75961776666391,
1.78244003932377));
#72264=CARTESIAN_POINT('Ctrl Pts',(-6.70705377619678,-4.5864056957169,1.77421969217049));
#72265=CARTESIAN_POINT('Ctrl Pts',(-6.82552467503089,-4.41315658909366,
1.76599758736769));
#72266=CARTESIAN_POINT('Ctrl Pts',(-6.93726828672637,-4.23533071591357,
1.75777548256488));
#72267=CARTESIAN_POINT('Ctrl Pts',(-7.04194857682741,-4.05347354793618,
1.74955337776207));
#72268=CARTESIAN_POINT('Ctrl Pts',(-7.08785672234551,-3.97371903710175,
1.74594752623656));
#72269=CARTESIAN_POINT('Ctrl Pts',(-7.13240694770843,-3.89318953402025,
1.74234167471104));
#72270=CARTESIAN_POINT('Ctrl Pts',(-7.17557366011081,-3.8119326083791,1.73873582318552));
#72271=CARTESIAN_POINT('Ctrl Pts',(-7.27390924468367,-3.62682591762555,
1.73052154190463));
#72272=CARTESIAN_POINT('Ctrl Pts',(-7.36509510738364,-3.43788036080296,
1.72230726062374));
#72273=CARTESIAN_POINT('Ctrl Pts',(-7.44884708413954,-3.24566860286225,
1.71409297934284));
#72274=CARTESIAN_POINT('Ctrl Pts',(-7.53258335119622,-3.05349289886344,
1.70588023884813));
#72275=CARTESIAN_POINT('Ctrl Pts',(-7.60888839697619,-2.8580524879719,1.69766749835342));
#72276=CARTESIAN_POINT('Ctrl Pts',(-7.67752562207033,-2.65994133111119,
1.68945475785871));
#72277=CARTESIAN_POINT('Ctrl Pts',(-7.74615513048944,-2.46185244728693,
1.6812429406975));
#72278=CARTESIAN_POINT('Ctrl Pts',(-7.80711844230906,-2.26109369679558,
1.67303112353629));
#72279=CARTESIAN_POINT('Ctrl Pts',(-7.86022811674692,-2.05827634568374,
1.66481930637508));
#72280=CARTESIAN_POINT('Ctrl Pts',(-7.91334192051017,-1.85544322533877,
1.65660685073763));
#72281=CARTESIAN_POINT('Ctrl Pts',(-7.95860078932263,-1.65055147055819,
1.64839439510018));
#72282=CARTESIAN_POINT('Ctrl Pts',(-7.99586765266581,-1.44422575920546,
1.64018193946274));
#72283=CARTESIAN_POINT('Ctrl Pts',(-8.03313464924543,-1.23789931019728,
1.63196945446413));
#72284=CARTESIAN_POINT('Ctrl Pts',(-8.0624095334704,-1.03013918645309,1.62375696946551));
#72285=CARTESIAN_POINT('Ctrl Pts',(-8.08360659039843,-0.82157900056356,
1.6155444844669));
#72286=CARTESIAN_POINT('Ctrl Pts',(-8.10480806444663,-0.612975354140554,
1.60733028812067));
#72287=CARTESIAN_POINT('Ctrl Pts',(-8.11792831905951,-0.403571607369352,
1.59911609177443));
#72288=CARTESIAN_POINT('Ctrl Pts',(-8.12293352926269,-0.194006292887625,
1.59090189542819));
#72289=CARTESIAN_POINT('Ctrl Pts',(-8.12447808619866,-0.129336569362995,
1.58836707802292));
#72290=CARTESIAN_POINT('Ctrl Pts',(-8.12525024040116,-0.064651475246315,
1.58583226061766));
#72291=CARTESIAN_POINT('Ctrl Pts',(-8.12524999994385,3.02060131589238E-5,
1.58329744321239));
#72292=CARTESIAN_POINT('Origin',(0.,0.,24.4167025567876));
#72293=CARTESIAN_POINT('',(4.94671019697112,6.44580737750965,4.87493507917627));
#72294=CARTESIAN_POINT('',(4.94648442104396,6.445513583535,4.7083419611594));
#72295=CARTESIAN_POINT('',(4.9467595481762,6.44587135576158,24.4167025567876));
#72296=CARTESIAN_POINT('',(-8.12518278065587,-2.09407945338198E-5,3.41670255698467));
#72297=CARTESIAN_POINT('Ctrl Pts',(4.94648442104396,6.445513583535,4.7083419611594));
#72298=CARTESIAN_POINT('Ctrl Pts',(5.64364652292867,5.90964851341047,4.6738994556356));
#72299=CARTESIAN_POINT('Ctrl Pts',(7.19392102387665,4.26498724618048,4.5865257495993));
#72300=CARTESIAN_POINT('Ctrl Pts',(8.43364688506178,0.784339091177833,4.44622084305048));
#72301=CARTESIAN_POINT('Ctrl Pts',(7.78105715559112,-3.34615258666749,4.28742724151297));
#72302=CARTESIAN_POINT('Ctrl Pts',(5.23185395479474,-6.66102783264922,4.12863363997545));
#72303=CARTESIAN_POINT('Ctrl Pts',(1.40739926919892,-8.35229398964753,3.96984003843793));
#72304=CARTESIAN_POINT('Ctrl Pts',(-2.76010551353616,-8.00770910714061,
3.81104643690042));
#72305=CARTESIAN_POINT('Ctrl Pts',(-6.25484139177157,-5.71126490000266,
3.6522528353629));
#72306=CARTESIAN_POINT('Ctrl Pts',(-7.88570092334897,-2.65791459092136,
3.52080487600157));
#72307=CARTESIAN_POINT('Ctrl Pts',(-8.12461652328501,-0.653270324207159,
3.44228811715276));
#72308=CARTESIAN_POINT('Ctrl Pts',(-8.12455793610677,-2.09859534307796E-5,
3.41670255881645));
#72309=CARTESIAN_POINT('Ctrl Pts',(-8.12524999997303,-2.09359364451616E-5,
3.41670255678761));
#72310=CARTESIAN_POINT('Ctrl Pts',(-8.12525054662003,0.212133106632909,
3.40839391109587));
#72311=CARTESIAN_POINT('Ctrl Pts',(-8.11693759016218,0.424271844703091,
3.40008526540412));
#72312=CARTESIAN_POINT('Ctrl Pts',(-8.10034075105971,0.635741519189564,
3.39177661971238));
#72313=CARTESIAN_POINT('Ctrl Pts',(-8.08374270635953,0.847226554875311,
3.38346737047896));
#72314=CARTESIAN_POINT('Ctrl Pts',(-8.05885960296614,1.05804214951943,3.37515812124554));
#72315=CARTESIAN_POINT('Ctrl Pts',(-8.02577298472956,1.26753917497061,3.36684887201212));
#72316=CARTESIAN_POINT('Ctrl Pts',(-7.9926785791969,1.47708550782921,3.35853766710636));
#72317=CARTESIAN_POINT('Ctrl Pts',(-7.95137684593506,1.6853123734601,3.3502264622006));
#72318=CARTESIAN_POINT('Ctrl Pts',(-7.90200075295423,1.89157914526747,3.34191525729484));
#72319=CARTESIAN_POINT('Ctrl Pts',(-7.88764430434135,1.95155266952234,3.33949871562584));
#72320=CARTESIAN_POINT('Ctrl Pts',(-7.87260558032577,2.01136056062553,3.33708217395684));
#72321=CARTESIAN_POINT('Ctrl Pts',(-7.85688865322471,2.07098726537098,3.33466563228784));
#72322=CARTESIAN_POINT('Ctrl Pts',(-7.80341260928096,2.27386409127254,3.32644347234192));
#72323=CARTESIAN_POINT('Ctrl Pts',(-7.74206565800979,2.47470203848903,3.31822131239599));
#72324=CARTESIAN_POINT('Ctrl Pts',(-7.67302839265335,2.67288661338926,3.30999915245006));
#72325=CARTESIAN_POINT('Ctrl Pts',(-7.6040038528869,2.87103465706786,3.30177850808903));
#72326=CARTESIAN_POINT('Ctrl Pts',(-7.52729192531106,3.06653002601864,3.29355786372799));
#72327=CARTESIAN_POINT('Ctrl Pts',(-7.44312258174497,3.25877489182945,3.28533721936695));
#72328=CARTESIAN_POINT('Ctrl Pts',(-7.35896269403651,3.45099816022721,3.27711749853983));
#72329=CARTESIAN_POINT('Ctrl Pts',(-7.26734718125301,3.63997138426629,3.2688977777127));
#72330=CARTESIAN_POINT('Ctrl Pts',(-7.16855385840787,3.82511740232971,3.26067805688557));
#72331=CARTESIAN_POINT('Ctrl Pts',(-7.06975261962332,4.01027825545101,3.25245767744295));
#72332=CARTESIAN_POINT('Ctrl Pts',(-6.96377255814811,4.19161102817368,3.24423729800033));
#72333=CARTESIAN_POINT('Ctrl Pts',(-6.85093758982922,4.36856288758271,3.23601691855772));
#72334=CARTESIAN_POINT('Ctrl Pts',(-6.73810303907606,4.54551409215014,3.22779656953607));
#72335=CARTESIAN_POINT('Ctrl Pts',(-6.61841379315987,4.71808416841445,3.21957622051443));
#72336=CARTESIAN_POINT('Ctrl Pts',(-6.49223755427729,4.8857485712357,3.21135587149278));
#72337=CARTESIAN_POINT('Ctrl Pts',(-6.36603433721458,5.05344882296558,3.20313376484974));
#72338=CARTESIAN_POINT('Ctrl Pts',(-6.23334153372333,5.2162410698821,3.19491165820669));
#72339=CARTESIAN_POINT('Ctrl Pts',(-6.09456832782582,5.3736323339025,3.18668955156365));
#72340=CARTESIAN_POINT('Ctrl Pts',(-6.03370874084892,5.44265695043495,3.18308371129255));
#72341=CARTESIAN_POINT('Ctrl Pts',(-5.97168022833068,5.51064323045342,3.17947787102145));
#72342=CARTESIAN_POINT('Ctrl Pts',(-5.90851966259576,5.57755169937665,3.17587203075034));
#72343=CARTESIAN_POINT('Ctrl Pts',(-5.76449878431245,5.73011867446293,3.16764987066119));
#72344=CARTESIAN_POINT('Ctrl Pts',(-5.61454171433746,5.87712958608984,3.15942771057204));
#72345=CARTESIAN_POINT('Ctrl Pts',(-5.45910102793138,6.01813123231278,3.15120555048289));
#72346=CARTESIAN_POINT('Ctrl Pts',(-5.3036889937906,6.15910688780788,3.14298490597835));
#72347=CARTESIAN_POINT('Ctrl Pts',(-5.14279557911143,6.29407529048464,3.13476426147381));
#72348=CARTESIAN_POINT('Ctrl Pts',(-4.97690874665384,6.42262149670838,3.12654361696927));
#72349=CARTESIAN_POINT('Ctrl Pts',(-4.81104055046561,6.55115326163084,3.11832389599883));
#72350=CARTESIAN_POINT('Ctrl Pts',(-4.64018028965452,6.67326408979431,3.11010417502838));
#72351=CARTESIAN_POINT('Ctrl Pts',(-4.46484805175013,6.78858007519121,3.10188445405793));
#72352=CARTESIAN_POINT('Ctrl Pts',(-4.28950176515715,6.90390530040838,3.0936640744733));
#72353=CARTESIAN_POINT('Ctrl Pts',(-4.10968303060545,7.01243443053628,3.08544369488865));
#72354=CARTESIAN_POINT('Ctrl Pts',(-3.92594077841907,7.11383697921496,3.07722331530401));
#72355=CARTESIAN_POINT('Ctrl Pts',(-3.7421992062265,7.21523915262283,3.06900296614138));
#72356=CARTESIAN_POINT('Ctrl Pts',(-3.55453440513977,7.30951465706955,3.06078261697875));
#72357=CARTESIAN_POINT('Ctrl Pts',(-3.36352022173331,7.39637879509231,3.05256226781611));
#72358=CARTESIAN_POINT('Ctrl Pts',(-3.17246519697824,7.48326150581202,3.04434016103454));
#72359=CARTESIAN_POINT('Ctrl Pts',(-2.97805962791343,7.56272956208721,3.03611805425296));
#72360=CARTESIAN_POINT('Ctrl Pts',(-2.78089868479704,7.63454583242475,3.02789594747139));
#72361=CARTESIAN_POINT('Ctrl Pts',(-2.69443292613379,7.66604115903938,3.02429010805187));
#72362=CARTESIAN_POINT('Ctrl Pts',(-2.60743747384918,7.69606544792564,3.02068426863235));
#72363=CARTESIAN_POINT('Ctrl Pts',(-2.5199635922462,7.72460167621953,3.01707842921283));
#72364=CARTESIAN_POINT('Ctrl Pts',(-2.32050261699057,7.78967097257762,3.00885626924859));
#72365=CARTESIAN_POINT('Ctrl Pts',(-2.11848709807292,7.84702129777551,3.00063410928435));
#72366=CARTESIAN_POINT('Ctrl Pts',(-1.91453127864162,7.89647120843246,2.99241194932011));
#72367=CARTESIAN_POINT('Ctrl Pts',(-1.71061305423132,7.94591200402502,2.98419130494036));
#72368=CARTESIAN_POINT('Ctrl Pts',(-1.504755529824,7.98745522209652,2.97597066056061));
#72369=CARTESIAN_POINT('Ctrl Pts',(-1.2975857193745,8.02096994529809,2.96775001618086));
#72370=CARTESIAN_POINT('Ctrl Pts',(-1.09043918304662,8.05448090334806,2.95953029533469));
#72371=CARTESIAN_POINT('Ctrl Pts',(-0.881980946243665,8.07996512008632,
2.95131057448853));
#72372=CARTESIAN_POINT('Ctrl Pts',(-0.672846598932096,8.09734308380258,
2.94309085364236));
#72373=CARTESIAN_POINT('Ctrl Pts',(-0.463695494457813,8.11472243995089,
2.93487047418033));
#72374=CARTESIAN_POINT('Ctrl Pts',(-0.253868465142897,8.12399421810081,
2.92665009471829));
#72375=CARTESIAN_POINT('Ctrl Pts',(-0.0440056553494257,8.12513083370337,
2.91842971525625));
#72376=CARTESIAN_POINT('Ctrl Pts',(0.165856377813637,8.12626744509971,2.91020936621502));
#72377=CARTESIAN_POINT('Ctrl Pts',(0.375753896036386,8.11926895524163,2.9019890171738));
#72378=CARTESIAN_POINT('Ctrl Pts',(0.585046782080702,8.10415990866894,2.89376866813257));
#72379=CARTESIAN_POINT('Ctrl Pts',(0.794384417767329,8.08904763157828,2.88554656146983));
#72380=CARTESIAN_POINT('Ctrl Pts',(1.00311686856462,8.06582135454113,2.87732445480709));
#72381=CARTESIAN_POINT('Ctrl Pts',(1.21060804928841,8.03455759289198,2.86910234814435));
#72382=CARTESIAN_POINT('Ctrl Pts',(1.30160419689751,8.02084673607426,2.865496507988));
#72383=CARTESIAN_POINT('Ctrl Pts',(1.39236169515423,8.00559070101045,2.86189066783166));
#72384=CARTESIAN_POINT('Ctrl Pts',(1.48282738326404,7.98879906581348,2.85828482767532));
#72385=CARTESIAN_POINT('Ctrl Pts',(1.68910954411817,7.95051035254463,2.85006269932273));
#72386=CARTESIAN_POINT('Ctrl Pts',(1.89394194825558,7.90422130195749,2.84184057097013));
#72387=CARTESIAN_POINT('Ctrl Pts',(2.09669841206705,7.85006645394391,2.83361844261754));
#72388=CARTESIAN_POINT('Ctrl Pts',(2.29941724410512,7.79592165711652,2.82539784029901));
#72389=CARTESIAN_POINT('Ctrl Pts',(2.5000606198312,7.73391405278821,2.81717723798048));
#72390=CARTESIAN_POINT('Ctrl Pts',(2.69801531649065,7.66422865750245,2.80895663566195));
#72391=CARTESIAN_POINT('Ctrl Pts',(2.89989977431968,7.59315988023536,2.80057283941912));
#72392=CARTESIAN_POINT('Ctrl Pts',(3.09898738478772,7.51410537956481,2.79218904317629));
#72393=CARTESIAN_POINT('Ctrl Pts',(3.29464576591258,7.42731424134285,2.78380524693346));
#72394=CARTESIAN_POINT('Ctrl Pts',(3.4864840455747,7.34221764312561,2.77558513880921));
#72395=CARTESIAN_POINT('Ctrl Pts',(3.67502548782356,7.24968384603085,2.76736503068495));
#72396=CARTESIAN_POINT('Ctrl Pts',(3.85969528407515,7.14999579556436,2.7591449225607));
#72397=CARTESIAN_POINT('Ctrl Pts',(4.04988111205948,7.04733009276431,2.75067928225858));
#72398=CARTESIAN_POINT('Ctrl Pts',(4.23596012924437,6.93707627618972,2.74221364195646));
#72399=CARTESIAN_POINT('Ctrl Pts',(4.41733225402655,6.81959407296627,2.73374800165434));
#72400=CARTESIAN_POINT('Ctrl Pts',(4.59870437880873,6.70211186974282,2.72528236135222));
#72401=CARTESIAN_POINT('Ctrl Pts',(4.77536932835898,6.57740147163754,2.71681672105011));
#72402=CARTESIAN_POINT('Ctrl Pts',(4.94675954817618,6.44587135576159,2.70835108074799));
#72403=CARTESIAN_POINT('',(-8.12524999887371,-0.000135288016022189,3.58329744321239));
#72404=CARTESIAN_POINT('Ctrl Pts',(-8.12524999887371,-0.000135288016022189,
3.58329744321239));
#72405=CARTESIAN_POINT('Ctrl Pts',(-8.12525350335822,0.210340211731544,
3.5750539685695));
#72406=CARTESIAN_POINT('Ctrl Pts',(-8.11707446516784,0.420817569687947,
3.56681049392662));
#72407=CARTESIAN_POINT('Ctrl Pts',(-8.1007385130676,0.630652919919719,3.55856701928373));
#72408=CARTESIAN_POINT('Ctrl Pts',(-8.08440281262829,0.840485037566233,
3.55032367163439));
#72409=CARTESIAN_POINT('Ctrl Pts',(-8.05991047461304,1.04967487660205,3.54208032398506));
#72410=CARTESIAN_POINT('Ctrl Pts',(-8.02733908616164,1.25758290314462,3.53383697633572));
#72411=CARTESIAN_POINT('Ctrl Pts',(-7.99475885361346,1.46554738287492,3.52559139037331));
#72412=CARTESIAN_POINT('Ctrl Pts',(-7.95409523049929,1.67222906598806,3.5173458044109));
#72413=CARTESIAN_POINT('Ctrl Pts',(-7.90547731210573,1.87699654509046,3.50910021844849));
#72414=CARTESIAN_POINT('Ctrl Pts',(-7.85902523741095,2.07264198916994,3.5012219589984));
#72415=CARTESIAN_POINT('Ctrl Pts',(-7.80531218040087,2.26653982392757,3.4933436995483));
#72416=CARTESIAN_POINT('Ctrl Pts',(-7.74449383032738,2.45815029534834,3.48546544009821));
#72417=CARTESIAN_POINT('Ctrl Pts',(-7.68102064709461,2.65812491726941,3.47724328009178));
#72418=CARTESIAN_POINT('Ctrl Pts',(-7.60978737587496,2.85567276256273,3.46902112008536));
#72419=CARTESIAN_POINT('Ctrl Pts',(-7.53100486733088,3.05018905163904,3.46079896007893));
#72420=CARTESIAN_POINT('Ctrl Pts',(-7.45223688070886,3.24466948567034,3.45257831565722));
#72421=CARTESIAN_POINT('Ctrl Pts',(-7.3659225448347,3.43611920536153,3.44435767123552));
#72422=CARTESIAN_POINT('Ctrl Pts',(-7.27232120155027,3.62395252507292,3.43613702681382));
#72423=CARTESIAN_POINT('Ctrl Pts',(-7.17873037374545,3.81176474297771,3.42791730592607));
#72424=CARTESIAN_POINT('Ctrl Pts',(-7.07785430448506,3.99596110795115,3.41969758503833));
#72425=CARTESIAN_POINT('Ctrl Pts',(-6.969999094814,4.17597894879656,3.41147786415058));
#72426=CARTESIAN_POINT('Ctrl Pts',(-6.86213524311471,4.35601121378771,3.40325748464782));
#72427=CARTESIAN_POINT('Ctrl Pts',(-6.74729128299553,4.53186403107694,3.39503710514507));
#72428=CARTESIAN_POINT('Ctrl Pts',(-6.62581815285298,4.70300131488647,3.38681672564231));
#72429=CARTESIAN_POINT('Ctrl Pts',(-6.50434547224924,4.87413796536377,3.37859637656093));
#72430=CARTESIAN_POINT('Ctrl Pts',(-6.37624384370664,5.04055887813666,3.37037602747954));
#72431=CARTESIAN_POINT('Ctrl Pts',(-6.24190653496301,5.2017583922445,3.36215567839816));
#72432=CARTESIAN_POINT('Ctrl Pts',(-6.10754050310864,5.36299237296134,3.35393357169636));
#72433=CARTESIAN_POINT('Ctrl Pts',(-5.96693631642396,5.51900249787455,3.34571146499456));
#72434=CARTESIAN_POINT('Ctrl Pts',(-5.82052710764396,5.66931669177881,3.33748935829275));
#72435=CARTESIAN_POINT('Ctrl Pts',(-5.75631872560042,5.73523762167929,3.33388351838206));
#72436=CARTESIAN_POINT('Ctrl Pts',(-5.69099435995881,5.80006351310103,3.33027767847137));
#72437=CARTESIAN_POINT('Ctrl Pts',(-5.62459279563755,5.86375676898029,3.32667183856068));
#72438=CARTESIAN_POINT('Ctrl Pts',(-5.47318166809742,6.00899231859359,3.31844967855303));
#72439=CARTESIAN_POINT('Ctrl Pts',(-5.31611724404946,6.14838420077997,3.31022751854539));
#72440=CARTESIAN_POINT('Ctrl Pts',(-5.15387402109143,6.28150221978938,3.30200535853774));
#72441=CARTESIAN_POINT('Ctrl Pts',(-4.99166070430765,6.414595701252,3.29378471411482));
#72442=CARTESIAN_POINT('Ctrl Pts',(-4.82427072192752,6.5414174405494,3.2855640696919));
#72443=CARTESIAN_POINT('Ctrl Pts',(-4.65221201782622,6.66157720841644,3.27734342526898));
#72444=CARTESIAN_POINT('Ctrl Pts',(-4.48017264336145,6.78172347714287,3.26912370438009));
#72445=CARTESIAN_POINT('Ctrl Pts',(-4.3034658361829,6.89520909970062,3.26090398349119));
#72446=CARTESIAN_POINT('Ctrl Pts',(-4.1226295898715,7.00168642736991,3.2526842626023));
#72447=CARTESIAN_POINT('Ctrl Pts',(-3.94177885383763,7.10817228666357,3.24446388309836));
#72448=CARTESIAN_POINT('Ctrl Pts',(-3.75679827050111,7.20764857693053,3.23624350359442));
#72449=CARTESIAN_POINT('Ctrl Pts',(-3.56825248706198,7.29981244629449,3.22802312409047));
#72450=CARTESIAN_POINT('Ctrl Pts',(-3.37970740137907,7.39197597458526,3.2198027750079));
#72451=CARTESIAN_POINT('Ctrl Pts',(-3.18759740831881,7.47682700888961,3.21158242592532));
#72452=CARTESIAN_POINT('Ctrl Pts',(-2.99250976947125,7.55410966574613,3.20336207684274));
#72453=CARTESIAN_POINT('Ctrl Pts',(-2.79738041828228,7.63140884666633,3.1951399701398));
#72454=CARTESIAN_POINT('Ctrl Pts',(-2.59927242383551,7.70113630852653,3.18691786343685));
#72455=CARTESIAN_POINT('Ctrl Pts',(-2.39879198582123,7.76308473296922,3.17869575673391));
#72456=CARTESIAN_POINT('Ctrl Pts',(-2.31087043610211,7.79025247827947,3.17508991683033));
#72457=CARTESIAN_POINT('Ctrl Pts',(-2.22249281008404,7.81592472265312,3.17148407692676));
#72458=CARTESIAN_POINT('Ctrl Pts',(-2.13371115334702,7.84008700695231,3.16787823702318));
#72459=CARTESIAN_POINT('Ctrl Pts',(-1.93126816993193,7.89518267760579,3.15965607701146));
#72460=CARTESIAN_POINT('Ctrl Pts',(-1.72665665855564,7.94244216953387,3.15143391699972));
#72461=CARTESIAN_POINT('Ctrl Pts',(-1.52049910613384,7.9817147299779,3.143211756988));
#72462=CARTESIAN_POINT('Ctrl Pts',(-1.31437955458275,8.02098005133962,3.13499111256102));
#72463=CARTESIAN_POINT('Ctrl Pts',(-1.10671482055134,8.05226132437254,3.12677046813403));
#72464=CARTESIAN_POINT('Ctrl Pts',(-0.898137639883169,8.0754588936063,3.11854982370704));
#72465=CARTESIAN_POINT('Ctrl Pts',(-0.689583891453495,8.09865385674972,
3.11033010281397));
#72466=CARTESIAN_POINT('Ctrl Pts',(-0.480118194254602,8.11376689653932,
3.10211038192091));
#72467=CARTESIAN_POINT('Ctrl Pts',(-0.270379299796881,8.1207501252496,3.09389066102784));
#72468=CARTESIAN_POINT('Ctrl Pts',(-0.0606235997583052,8.12773391349947,
3.08567028151976));
#72469=CARTESIAN_POINT('Ctrl Pts',(0.149405046379006,8.12658657653562,3.07744990201167));
#72470=CARTESIAN_POINT('Ctrl Pts',(0.359065913971908,8.11731231578061,3.06922952250359));
#72471=CARTESIAN_POINT('Ctrl Pts',(0.568726005667304,8.1080380893471,3.06100917341689));
#72472=CARTESIAN_POINT('Ctrl Pts',(0.778018026803319,8.09063701499423,3.05278882433019));
#72473=CARTESIAN_POINT('Ctrl Pts',(0.986303865499881,8.06516535772206,3.04456847524349));
#72474=CARTESIAN_POINT('Ctrl Pts',(1.19463423848764,8.03968825426973,3.03634636853648));
#72475=CARTESIAN_POINT('Ctrl Pts',(1.40195770621676,8.00613715632205,3.02812426182946));
#72476=CARTESIAN_POINT('Ctrl Pts',(1.607642761719,7.96462003570745,3.01990215512245));
#72477=CARTESIAN_POINT('Ctrl Pts',(1.69784681793703,7.94641252581916,3.01629631524352));
#72478=CARTESIAN_POINT('Ctrl Pts',(1.78773587569151,7.92667357721418,3.01269047536459));
#72479=CARTESIAN_POINT('Ctrl Pts',(1.87725731472338,7.90541539305921,3.00908463548566));
#72480=CARTESIAN_POINT('Ctrl Pts',(2.08138547454277,7.85694215514455,3.00086254402858));
#72481=CARTESIAN_POINT('Ctrl Pts',(2.28366885122072,7.80055040854686,2.9926404525715));
#72482=CARTESIAN_POINT('Ctrl Pts',(2.48348871359225,7.7364055847635,2.98441836111442));
#72483=CARTESIAN_POINT('Ctrl Pts',(2.68327103617755,7.67227281174899,2.97619781432639));
#72484=CARTESIAN_POINT('Ctrl Pts',(2.88059048735292,7.6003899589272,2.96797726753835));
#72485=CARTESIAN_POINT('Ctrl Pts',(3.07484378835328,7.52097222702792,2.95975672075032));
#72486=CARTESIAN_POINT('Ctrl Pts',(3.26909078469402,7.44155707270011,2.95153644076727));
#72487=CARTESIAN_POINT('Ctrl Pts',(3.46027155529169,7.35460763648865,2.94331616078422));
#72488=CARTESIAN_POINT('Ctrl Pts',(3.647802165979,7.26038751860939,2.93509588080117));
#72489=CARTESIAN_POINT('Ctrl Pts',(3.83531994853028,7.16617384590983,2.92687616313096));
#72490=CARTESIAN_POINT('Ctrl Pts',(4.0191878067775,7.06469061856965,2.91865644546074));
#72491=CARTESIAN_POINT('Ctrl Pts',(4.19884524925915,6.95624799265192,2.91043672779053));
#72492=CARTESIAN_POINT('Ctrl Pts',(4.37852390560449,6.8477925618815,2.90221603954004));
#72493=CARTESIAN_POINT('Ctrl Pts',(4.55399089994502,6.73237624282856,2.89399535128957));
#72494=CARTESIAN_POINT('Ctrl Pts',(4.72471274193336,6.6103537778785,2.88577466303908));
#72495=CARTESIAN_POINT('Ctrl Pts',(4.79965682014225,6.55678792449998,2.88216591622614));
#72496=CARTESIAN_POINT('Ctrl Pts',(4.87368685165283,6.50194958619583,2.87855716941319));
#72497=CARTESIAN_POINT('Ctrl Pts',(4.94675954817621,6.44587135576157,2.87494842260024));
#72498=CARTESIAN_POINT('Ctrl Pts',(4.94671019697112,6.44580737750965,4.87493507917627));
#72499=CARTESIAN_POINT('Ctrl Pts',(5.75015646111357,5.82789648496184,4.83522813691696));
#72500=CARTESIAN_POINT('Ctrl Pts',(7.356633927154,4.0356546125411,4.74258999414515));
#72501=CARTESIAN_POINT('Ctrl Pts',(8.46217010059878,0.365053444517306,4.59702065086083));
#72502=CARTESIAN_POINT('Ctrl Pts',(7.60550572314025,-3.72798464644211,4.43822704932331));
#72503=CARTESIAN_POINT('Ctrl Pts',(4.89501810258881,-6.91233568369901,4.27943344778579));
#72504=CARTESIAN_POINT('Ctrl Pts',(0.991381904642859,-8.41182196364104,
4.12063984624828));
#72505=CARTESIAN_POINT('Ctrl Pts',(-3.15390118497908,-7.86094740754393,
3.96184624471076));
#72506=CARTESIAN_POINT('Ctrl Pts',(-6.53042864729724,-5.39398632844221,
3.80305264317324));
#72507=CARTESIAN_POINT('Ctrl Pts',(-7.9486544727063,-2.38889033598931,3.67686971310851));
#72508=CARTESIAN_POINT('Ctrl Pts',(-8.12500981392525,-0.518932006235639,
3.6036179835563));
#72509=CARTESIAN_POINT('Ctrl Pts',(-8.12470237155434,-0.000135567501295938,
3.58329745451658));
#72510=CARTESIAN_POINT('Origin',(0.,0.,24.4167025567876));
#72511=CARTESIAN_POINT('',(4.94675954817622,6.44587135576156,6.87494727151379));
#72512=CARTESIAN_POINT('',(4.9467595481762,6.44587135576158,6.70835375129049));
#72513=CARTESIAN_POINT('',(4.9467595481762,6.44587135576158,24.4167025567876));
#72514=CARTESIAN_POINT('',(-8.1252499987303,0.000143642949229983,5.41670255678761));
#72515=CARTESIAN_POINT('Ctrl Pts',(4.9467595481762,6.44587135576158,6.70835375129049));
#72516=CARTESIAN_POINT('Ctrl Pts',(5.11326717757315,6.31808828965565,6.70013160170819));
#72517=CARTESIAN_POINT('Ctrl Pts',(5.27480674507703,6.18386087726778,6.69190945212589));
#72518=CARTESIAN_POINT('Ctrl Pts',(5.43088886988298,6.04360270413941,6.68368730254359));
#72519=CARTESIAN_POINT('Ctrl Pts',(5.52172970930857,5.96197151031037,6.6789019565543));
#72520=CARTESIAN_POINT('Ctrl Pts',(5.61072256014284,5.87829825786018,6.67411661056502));
#72521=CARTESIAN_POINT('Ctrl Pts',(5.69777643160371,5.79267048069897,6.66933126457574));
#72522=CARTESIAN_POINT('Ctrl Pts',(5.84735200294864,5.64554521818103,6.66110910456816));
#72523=CARTESIAN_POINT('Ctrl Pts',(5.99125071310778,5.49259917758122,6.65288694456059));
#72524=CARTESIAN_POINT('Ctrl Pts',(6.12902875487278,5.334294150536,6.64466478455301));
#72525=CARTESIAN_POINT('Ctrl Pts',(6.26678140011208,5.17601830374068,6.63644414013018));
#72526=CARTESIAN_POINT('Ctrl Pts',(6.39841543505899,5.01238566456822,6.62822349570735));
#72527=CARTESIAN_POINT('Ctrl Pts',(6.52352602984438,4.84389261859125,6.62000285128451));
#72528=CARTESIAN_POINT('Ctrl Pts',(6.64862256929821,4.67541850167165,6.61178313039564));
#72529=CARTESIAN_POINT('Ctrl Pts',(6.76719695582161,4.50208530493441,6.60356340950677));
#72530=CARTESIAN_POINT('Ctrl Pts',(6.87888604857588,4.32442068874065,6.59534368861789));
#72531=CARTESIAN_POINT('Ctrl Pts',(6.99058409055312,4.1467418369557,6.58712330911399));
#72532=CARTESIAN_POINT('Ctrl Pts',(7.09539557702665,3.96473112067881,6.57890292961008));
#72533=CARTESIAN_POINT('Ctrl Pts',(7.19300137027119,3.77894414483421,6.57068255010618));
#72534=CARTESIAN_POINT('Ctrl Pts',(7.29060680230357,3.59315785653605,6.56246220102364));
#72535=CARTESIAN_POINT('Ctrl Pts',(7.38100645954513,3.40359559914725,6.55424185194111));
#72536=CARTESIAN_POINT('Ctrl Pts',(7.46392749545489,3.21083694775872,6.54602150285857));
#72537=CARTESIAN_POINT('Ctrl Pts',(7.54686626098896,3.01803708199755,6.53779939615566));
#72538=CARTESIAN_POINT('Ctrl Pts',(7.62232309398686,2.82203972804977,6.52957728945276));
#72539=CARTESIAN_POINT('Ctrl Pts',(7.69007314197288,2.62344480285128,6.52135518274985));
#72540=CARTESIAN_POINT('Ctrl Pts',(7.71978521399354,2.53635015279798,6.51774934284597));
#72541=CARTESIAN_POINT('Ctrl Pts',(7.74801567483915,2.44875614619009,6.51414350294209));
#72542=CARTESIAN_POINT('Ctrl Pts',(7.7747485585597,2.3607143862979,6.5105376630382));
#72543=CARTESIAN_POINT('Ctrl Pts',(7.83570579827994,2.15995854120309,6.50231550303063));
#72544=CARTESIAN_POINT('Ctrl Pts',(7.88889320817592,1.9568072932397,6.49409334302306));
#72545=CARTESIAN_POINT('Ctrl Pts',(7.93414200400985,1.75187848400128,6.4858711830155));
#72546=CARTESIAN_POINT('Ctrl Pts',(7.97938245916653,1.54698744913946,6.47765053859263));
#72547=CARTESIAN_POINT('Ctrl Pts',(8.01668715724014,1.34031979501592,6.46942989416977));
#72548=CARTESIAN_POINT('Ctrl Pts',(8.04593809175954,1.13250509317743,6.4612092497469));
#72549=CARTESIAN_POINT('Ctrl Pts',(8.07518574013385,0.924713737918286,6.45298952885797));
#72550=CARTESIAN_POINT('Ctrl Pts',(8.09638139017429,0.715775884357431,6.44476980796903));
#72551=CARTESIAN_POINT('Ctrl Pts',(8.10945860640715,0.506328622012376,6.43655008708009));
#72552=CARTESIAN_POINT('Ctrl Pts',(8.12253687046756,0.296864577455713,6.42832970757622));
#72553=CARTESIAN_POINT('Ctrl Pts',(8.12749537984046,0.0868913369679979,
6.42010932807234));
#72554=CARTESIAN_POINT('Ctrl Pts',(8.12431970883006,-0.122950523445302,
6.41188894856847));
#72555=CARTESIAN_POINT('Ctrl Pts',(8.12114404957194,-0.332791607291501,
6.40366859948596));
#72556=CARTESIAN_POINT('Ctrl Pts',(8.10983427728161,-0.542501016966194,
6.39544825040345));
#72557=CARTESIAN_POINT('Ctrl Pts',(8.09042808378968,-0.751439274677085,
6.38722790132095));
#72558=CARTESIAN_POINT('Ctrl Pts',(8.07101774099448,-0.960422206177113,
6.37900579461805));
#72559=CARTESIAN_POINT('Ctrl Pts',(8.04350754585145,-1.16863336237135,6.37078368791515));
#72560=CARTESIAN_POINT('Ctrl Pts',(8.00798706716778,-1.37543836451278,6.36256158121226));
#72561=CARTESIAN_POINT('Ctrl Pts',(7.99240940999671,-1.46613357876682,6.3589557413084));
#72562=CARTESIAN_POINT('Ctrl Pts',(7.9752918045222,-1.55655844534596,6.35534990140455));
#72563=CARTESIAN_POINT('Ctrl Pts',(7.95664491912615,-1.64666001149114,6.35174406150069));
#72564=CARTESIAN_POINT('Ctrl Pts',(7.91412565053497,-1.85211269755876,6.34352190149313));
#72565=CARTESIAN_POINT('Ctrl Pts',(7.86363746031812,-2.05595153774641,6.33529974148558));
#72566=CARTESIAN_POINT('Ctrl Pts',(7.80532772794959,-2.25755323786646,6.32707758147802));
#72567=CARTESIAN_POINT('Ctrl Pts',(7.74702874377128,-2.45911777689289,6.31885693705519));
#72568=CARTESIAN_POINT('Ctrl Pts',(7.68091117691605,-2.65844571550676,6.31063629263237));
#72569=CARTESIAN_POINT('Ctrl Pts',(7.60717260809678,-2.85492775269743,6.30241564820954));
#72570=CARTESIAN_POINT('Ctrl Pts',(7.53344232330819,-3.05138771645695,6.29419592732064));
#72571=CARTESIAN_POINT('Ctrl Pts',(7.45209284949711,-3.2450021408717,6.28597620643174));
#72572=CARTESIAN_POINT('Ctrl Pts',(7.36337065003751,-3.43517979626484,6.27775648554285));
#72573=CARTESIAN_POINT('Ctrl Pts',(7.27464134160532,-3.62537268987063,6.26953610603896));
#72574=CARTESIAN_POINT('Ctrl Pts',(7.17853824946032,-3.81212799559555,6.26131572653507));
#72575=CARTESIAN_POINT('Ctrl Pts',(7.07535517616391,-3.99487630517273,6.25309534703119));
#72576=CARTESIAN_POINT('Ctrl Pts',(6.9721724847201,-4.17762393844794,6.2448749979487));
#72577=CARTESIAN_POINT('Ctrl Pts',(6.86191001197225,-4.35636434954377,6.2366546488662));
#72578=CARTESIAN_POINT('Ctrl Pts',(6.74490680083194,-4.53055402909964,6.22843429978371));
#72579=CARTESIAN_POINT('Ctrl Pts',(6.62787857284226,-4.70478095273569,6.22021219308079));
#72580=CARTESIAN_POINT('Ctrl Pts',(6.50410689170542,-4.87445495589887,6.21199008637787));
#72581=CARTESIAN_POINT('Ctrl Pts',(6.37397391533588,-5.03906182628451,6.20376797967495));
#72582=CARTESIAN_POINT('Ctrl Pts',(6.31690354444877,-5.11125087018064,6.20016213977103));
#72583=CARTESIAN_POINT('Ctrl Pts',(6.25861024672682,-5.18246575875067,6.1965562998671));
#72584=CARTESIAN_POINT('Ctrl Pts',(6.19912872449208,-5.25266509685104,6.19295045996318));
#72585=CARTESIAN_POINT('Ctrl Pts',(6.06349691433436,-5.41273603889675,6.18472829995561));
#72586=CARTESIAN_POINT('Ctrl Pts',(5.92163949572164,-5.56757725726279,6.17650613994804));
#72587=CARTESIAN_POINT('Ctrl Pts',(5.77398408845677,-5.71671193158691,6.16828397994048));
#72588=CARTESIAN_POINT('Ctrl Pts',(5.62635589840466,-5.86581911602604,6.16006333551762));
#72589=CARTESIAN_POINT('Ctrl Pts',(5.47293206030617,-6.00922164620704,6.15184269109476));
#72590=CARTESIAN_POINT('Ctrl Pts',(5.31417758224729,-6.1464790072724,6.14362204667191));
#72591=CARTESIAN_POINT('Ctrl Pts',(5.1554409391846,-6.28372094839786,6.13540232578308));
#72592=CARTESIAN_POINT('Ctrl Pts',(4.99137507492434,-6.41481890572221,6.12718260489425));
#72593=CARTESIAN_POINT('Ctrl Pts',(4.82247927684922,-6.53937162018338,6.11896288400542));
#72594=CARTESIAN_POINT('Ctrl Pts',(4.65356994579412,-6.66393431458135,6.11074250450152));
#72595=CARTESIAN_POINT('Ctrl Pts',(4.47983014357609,-6.78195054084556,6.10252212499762));
#72596=CARTESIAN_POINT('Ctrl Pts',(4.30179028736472,-6.89306085030696,6.09430174549372));
#72597=CARTESIAN_POINT('Ctrl Pts',(4.12375109003059,-7.00417074857923,6.08608139641121));
#72598=CARTESIAN_POINT('Ctrl Pts',(3.94141212233445,-7.10837462717717,6.07786104732871));
#72599=CARTESIAN_POINT('Ctrl Pts',(3.75533113739616,-7.2053574242367,6.0696406982462));
#72600=CARTESIAN_POINT('Ctrl Pts',(3.56921036585876,-7.30236095751314,6.06141859154331));
#72601=CARTESIAN_POINT('Ctrl Pts',(3.37934624043094,-7.39214018827443,6.05319648484041));
#72602=CARTESIAN_POINT('Ctrl Pts',(3.18632035808629,-7.47442640863798,6.04497437813751));
#72603=CARTESIAN_POINT('Ctrl Pts',(3.10166803548755,-7.51051338094985,6.04136853823356));
#72604=CARTESIAN_POINT('Ctrl Pts',(3.01640789291937,-7.54515983824007,6.0377626983296));
#72605=CARTESIAN_POINT('Ctrl Pts',(2.93059020803865,-7.57834603294466,6.03415685842564));
#72606=CARTESIAN_POINT('Ctrl Pts',(2.73490577518451,-7.65401833403713,6.02593469841807));
#72607=CARTESIAN_POINT('Ctrl Pts',(2.53625652373678,-7.72211976588572,6.0177125384105));
#72608=CARTESIAN_POINT('Ctrl Pts',(2.33524608255602,-7.78243620573961,6.00949037840293));
#72609=CARTESIAN_POINT('Ctrl Pts',(2.13427269348219,-7.84274152750846,6.00126973398007));
#72610=CARTESIAN_POINT('Ctrl Pts',(1.93093926589526,-7.89526463656503,5.99304908955722));
#72611=CARTESIAN_POINT('Ctrl Pts',(1.72586489068135,-7.93984117861393,5.98482844513436));
#72612=CARTESIAN_POINT('Ctrl Pts',(1.52081355419142,-7.98441271278875,5.9766087242455));
#72613=CARTESIAN_POINT('Ctrl Pts',(1.31402194883852,-8.02103939958893,5.96838900335665));
#72614=CARTESIAN_POINT('Ctrl Pts',(1.10612048594723,-8.04960775647285,5.96016928246779));
#72615=CARTESIAN_POINT('Ctrl Pts',(0.898202364700916,-8.07817840243076,
5.9519489029639));
#72616=CARTESIAN_POINT('Ctrl Pts',(0.68917450026178,-8.09868938544733,5.94372852346));
#72617=CARTESIAN_POINT('Ctrl Pts',(0.479674636532062,-8.11107883117701,
5.93550814395611));
#72618=CARTESIAN_POINT('Ctrl Pts',(0.270175548104904,-8.1234682310567,5.92728779487363));
#72619=CARTESIAN_POINT('Ctrl Pts',(0.0602047586679581,-8.12773613901279,
5.91906744579115));
#72620=CARTESIAN_POINT('Ctrl Pts',(-0.149597219396503,-8.12387273622924,
5.91084709670866));
#72621=CARTESIAN_POINT('Ctrl Pts',(-0.359444055926759,-8.12000850739857,
5.90262499000573));
#72622=CARTESIAN_POINT('Ctrl Pts',(-0.569121713821754,-8.10800949991264,
5.89440288330279));
#72623=CARTESIAN_POINT('Ctrl Pts',(-0.777990919875223,-8.08791800719392,
5.88618077659986));
#72624=CARTESIAN_POINT('Ctrl Pts',(-0.869591399545033,-8.07910679751351,
5.88257493669595));
#72625=CARTESIAN_POINT('Ctrl Pts',(-0.961036437701934,-8.06873983509607,
5.87896909679204));
#72626=CARTESIAN_POINT('Ctrl Pts',(-1.05227243640895,-8.05682383337714,
5.87536325688813));
#72627=CARTESIAN_POINT('Ctrl Pts',(-1.26031189456843,-8.02965255694936,
5.86714109688057));
#72628=CARTESIAN_POINT('Ctrl Pts',(-1.46733271424759,-7.99441464640026,
5.85891893687301));
#72629=CARTESIAN_POINT('Ctrl Pts',(-1.67270239057271,-7.95121086848238,
5.85069677686544));
#72630=CARTESIAN_POINT('Ctrl Pts',(-1.87803421125648,-7.9080150542851,5.84247613244259));
#72631=CARTESIAN_POINT('Ctrl Pts',(-2.0817152073591,-7.85685636405683,5.83425548801973));
#72632=CARTESIAN_POINT('Ctrl Pts',(-2.28312310706937,-7.79788666501802,
5.82603484359687));
#72633=CARTESIAN_POINT('Ctrl Pts',(-2.4845083799611,-7.73892359082701,5.81781512270794));
#72634=CARTESIAN_POINT('Ctrl Pts',(-2.68362078314228,-7.67215134262059,
5.80959540181902));
#72635=CARTESIAN_POINT('Ctrl Pts',(-2.87985244255038,-7.59777187546695,
5.80137568093009));
#72636=CARTESIAN_POINT('Ctrl Pts',(-3.07609982525436,-7.52338644856975,
5.79315530142622));
#72637=CARTESIAN_POINT('Ctrl Pts',(-3.26946572601762,-7.44139268686743,
5.78493492192234));
#72638=CARTESIAN_POINT('Ctrl Pts',(-3.45936052270696,-7.35204137205692,
5.77671454241847));
#72639=CARTESIAN_POINT('Ctrl Pts',(-3.64925461664817,-7.26269038791092,
5.76849419333595));
#72640=CARTESIAN_POINT('Ctrl Pts',(-3.83567736629031,-7.16598203319751,
5.76027384425343));
#72641=CARTESIAN_POINT('Ctrl Pts',(-4.01806162330063,-7.06221412546085,
5.75205349517091));
#72642=CARTESIAN_POINT('Ctrl Pts',(-4.20048487649988,-6.95842403076024,
5.74383138846802));
#72643=CARTESIAN_POINT('Ctrl Pts',(-4.37886765541288,-6.84757151347801,
5.73560928176513));
#72644=CARTESIAN_POINT('Ctrl Pts',(-4.55266883186641,-6.72999955942437,
5.72738717506223));
#72645=CARTESIAN_POINT('Ctrl Pts',(-4.62889007783673,-6.6784378783587,5.72378133515836));
#72646=CARTESIAN_POINT('Ctrl Pts',(-4.70423050929684,-6.62558441772932,
5.72017549525449));
#72647=CARTESIAN_POINT('Ctrl Pts',(-4.77864627239449,-6.57147071558797,
5.71656965535063));
#72648=CARTESIAN_POINT('Ctrl Pts',(-4.9483316515537,-6.44807879318686,5.70834749534304));
#72649=CARTESIAN_POINT('Ctrl Pts',(-5.11326322577337,-6.31809069393865,
5.70012533533545));
#72650=CARTESIAN_POINT('Ctrl Pts',(-5.27293378566799,-6.18189751245207,
5.69190317532786));
#72651=CARTESIAN_POINT('Ctrl Pts',(-5.43257491360501,-6.04572943535508,
5.68368253090502));
#72652=CARTESIAN_POINT('Ctrl Pts',(-5.58695673828264,-5.90335875028178,
5.67546188648218));
#72653=CARTESIAN_POINT('Ctrl Pts',(-5.73560548418229,-5.75521652870837,
5.66724124205934));
#72654=CARTESIAN_POINT('Ctrl Pts',(-5.88423753039618,-5.60709094991612,
5.65902152117055));
#72655=CARTESIAN_POINT('Ctrl Pts',(-6.02713757470671,-5.45319533735453,
5.65080180028176));
#72656=CARTESIAN_POINT('Ctrl Pts',(-6.16386844811541,-5.29399785765231,
5.64258207939297));
#72657=CARTESIAN_POINT('Ctrl Pts',(-6.30061027725098,-5.13478762205919,
5.63436169988909));
#72658=CARTESIAN_POINT('Ctrl Pts',(-6.43118175342137,-4.97027489262195,
5.6261413203852));
#72659=CARTESIAN_POINT('Ctrl Pts',(-6.55518509520167,-4.80096197966052,
5.61792094088132));
#72660=CARTESIAN_POINT('Ctrl Pts',(-6.6791879780798,-4.63164969327948,5.6097005917988));
#72661=CARTESIAN_POINT('Ctrl Pts',(-6.79662260295266,-4.45753749859879,
5.60148024271627));
#72662=CARTESIAN_POINT('Ctrl Pts',(-6.90713342654288,-4.27915825723167,
5.59325989363375));
#72663=CARTESIAN_POINT('Ctrl Pts',(-7.01766787882271,-4.10074087600106,
5.58503778693083));
#72664=CARTESIAN_POINT('Ctrl Pts',(-7.12127541679716,-3.91805487633051,
5.57681568022792));
#72665=CARTESIAN_POINT('Ctrl Pts',(-7.21764495598233,-3.7316603344735,5.56859357352501));
#72666=CARTESIAN_POINT('Ctrl Pts',(-7.25990822772958,-3.64991621448168,
5.56498773362105));
#72667=CARTESIAN_POINT('Ctrl Pts',(-7.3007800083315,-3.56745915617885,5.56138189371708));
#72668=CARTESIAN_POINT('Ctrl Pts',(-7.34023687728877,-3.48433783491067,
5.55777605381312));
#72669=CARTESIAN_POINT('Ctrl Pts',(-7.42988527438341,-3.29548115639035,
5.54958336706141));
#72670=CARTESIAN_POINT('Ctrl Pts',(-7.5122579616518,-3.10312729128265,5.5413906803097));
#72671=CARTESIAN_POINT('Ctrl Pts',(-7.58709759951355,-2.90785790195389,
5.533197993558));
#72672=CARTESIAN_POINT('Ctrl Pts',(-7.66192252875972,-2.71262688991375,
5.52500691695679));
#72673=CARTESIAN_POINT('Ctrl Pts',(-7.72921725615911,-2.51448177661229,
5.51681584035558));
#72674=CARTESIAN_POINT('Ctrl Pts',(-7.78877289866171,-2.31402339996225,
5.50862476375437));
#72675=CARTESIAN_POINT('Ctrl Pts',(-7.84832856774633,-2.11356493383977,
5.50043368349716));
#72676=CARTESIAN_POINT('Ctrl Pts',(-7.90014505578914,-1.9107934881051,5.49224260323995));
#72677=CARTESIAN_POINT('Ctrl Pts',(-7.94406331021462,-1.70632519931046,
5.48405152298274));
#72678=CARTESIAN_POINT('Ctrl Pts',(-7.98797906389208,-1.5018685531386,5.47586090913359));
#72679=CARTESIAN_POINT('Ctrl Pts',(-8.02399742093537,-1.29571554997155,
5.46767029528444));
#72680=CARTESIAN_POINT('Ctrl Pts',(-8.05201031857506,-1.08849317501803,
5.45947968143529));
#72681=CARTESIAN_POINT('Ctrl Pts',(-8.0800290291043,-0.881227799843871,
5.4512873679714));
#72682=CARTESIAN_POINT('Ctrl Pts',(-8.10003891956644,-0.67289290616256,
5.4430950545075));
#72683=CARTESIAN_POINT('Ctrl Pts',(-8.11198360200186,-0.464122401261746,
5.43490274104361));
#72684=CARTESIAN_POINT('Ctrl Pts',(-8.12082910586603,-0.309519688480521,
5.42883601295827));
#72685=CARTESIAN_POINT('Ctrl Pts',(-8.12525273576271,-0.15467824512713,
5.42276928487294));
#72686=CARTESIAN_POINT('Ctrl Pts',(-8.1252499987303,0.000143642949229983,
5.41670255678761));
#72687=CARTESIAN_POINT('Ctrl Pts',(-8.12573213003729,0.000143651472636081,
5.41670255678761));
#72688=CARTESIAN_POINT('Ctrl Pts',(-8.12585620087823,0.150890634550742,
5.4107958552836));
#72689=CARTESIAN_POINT('Ctrl Pts',(-8.08492819103664,1.65244585104497,5.35195795326709));
#72690=CARTESIAN_POINT('Ctrl Pts',(-7.20076958702257,4.45987723445766,5.24018885073806));
#72691=CARTESIAN_POINT('Ctrl Pts',(-4.18945003805173,7.3613922576165,5.08139524920055));
#72692=CARTESIAN_POINT('Ctrl Pts',(-0.156962385468667,8.46858609222108,
4.92260164766304));
#72693=CARTESIAN_POINT('Ctrl Pts',(3.03083502612948,7.71915799554154,4.79825055164931));
#72694=CARTESIAN_POINT('Ctrl Pts',(4.57224865441187,6.73316530009744,4.7268306561481));
#72695=CARTESIAN_POINT('Ctrl Pts',(4.94648442104396,6.445513583535,4.7083419611594));
#72696=CARTESIAN_POINT('',(-8.12524999734671,0.000207647102394412,5.58329744321239));
#72697=CARTESIAN_POINT('Ctrl Pts',(-8.12533441219635,0.000207649259680899,
5.58329744321239));
#72698=CARTESIAN_POINT('Ctrl Pts',(-8.12562907062817,0.28536548919225,5.57212571550358));
#72699=CARTESIAN_POINT('Ctrl Pts',(-8.04117065934008,1.92141613527934,5.50802278728225));
#72700=CARTESIAN_POINT('Ctrl Pts',(-6.97069019979266,4.81155535844047,5.39098865854841));
#72701=CARTESIAN_POINT('Ctrl Pts',(-3.81915827587035,7.56013339119582,5.2321950570109));
#72702=CARTESIAN_POINT('Ctrl Pts',(0.263284048831229,8.46594757475224,5.07340145547338));
#72703=CARTESIAN_POINT('Ctrl Pts',(3.27676851279123,7.59770512482637,4.95431479619517));
#72704=CARTESIAN_POINT('Ctrl Pts',(4.67912522857444,6.65160043926574,4.88815933742947));
#72705=CARTESIAN_POINT('Ctrl Pts',(4.94671019697112,6.44580737750965,4.87493507917627));
#72706=CARTESIAN_POINT('Ctrl Pts',(4.94675954817621,6.44587135576157,6.8749472715138));
#72707=CARTESIAN_POINT('Ctrl Pts',(5.11324656279799,6.31810411006692,6.86672685106715));
#72708=CARTESIAN_POINT('Ctrl Pts',(5.27477223251341,6.18388990291018,6.85850643062051));
#72709=CARTESIAN_POINT('Ctrl Pts',(5.43084628687882,6.04364096971308,6.85028601017386));
#72710=CARTESIAN_POINT('Ctrl Pts',(5.58695183458293,5.90336373644284,6.84206393097306));
#72711=CARTESIAN_POINT('Ctrl Pts',(5.73760335044615,5.75704954245965,6.83384185177226));
#72712=CARTESIAN_POINT('Ctrl Pts',(5.88234568684138,5.60514913120057,6.82561977257147));
#72713=CARTESIAN_POINT('Ctrl Pts',(5.91455356959241,5.57134844262867,6.823790205843));
#72714=CARTESIAN_POINT('Ctrl Pts',(5.94646900781122,5.53727129789113,6.82196063911454));
#72715=CARTESIAN_POINT('Ctrl Pts',(5.97808724146106,5.50292290478255,6.82013107238607));
#72716=CARTESIAN_POINT('Ctrl Pts',(6.12018108924529,5.34855959037181,6.81190891237851));
#72717=CARTESIAN_POINT('Ctrl Pts',(6.2563163451145,5.18866424262867,6.80368675237095));
#72718=CARTESIAN_POINT('Ctrl Pts',(6.38607265362911,5.02372009820118,6.79546459236338));
#72719=CARTESIAN_POINT('Ctrl Pts',(6.51580504425887,4.85880635780642,6.78724394794052));
#72720=CARTESIAN_POINT('Ctrl Pts',(6.63916065193111,4.68884591001028,6.77902330351766));
#72721=CARTESIAN_POINT('Ctrl Pts',(6.75575976647367,4.51435460948691,6.7708026590948));
#72722=CARTESIAN_POINT('Ctrl Pts',(6.87234578189167,4.33988291188495,6.76258293820593));
#72723=CARTESIAN_POINT('Ctrl Pts',(6.98217665564701,4.16088162306084,6.75436321731706));
#72724=CARTESIAN_POINT('Ctrl Pts',(7.08491586655426,3.97789576614919,6.74614349642818));
#72725=CARTESIAN_POINT('Ctrl Pts',(7.18766330956431,3.79489524727575,6.73792311692429));
#72726=CARTESIAN_POINT('Ctrl Pts',(7.28331780747041,3.60790977841086,6.7297027374204));
#72727=CARTESIAN_POINT('Ctrl Pts',(7.37158817412478,3.41751011024161,6.72148235791651));
#72728=CARTESIAN_POINT('Ctrl Pts',(7.45985821411461,3.2271111466896,6.713262008834));
#72729=CARTESIAN_POINT('Ctrl Pts',(7.54074405579936,3.03329827799834,6.70504165975149));
#72730=CARTESIAN_POINT('Ctrl Pts',(7.61400193618793,2.83666389941184,6.69682131066898));
#72731=CARTESIAN_POINT('Ctrl Pts',(7.68727548008957,2.63998747776947,6.68859920396607));
#72732=CARTESIAN_POINT('Ctrl Pts',(7.75291770129322,2.44048861763195,6.68037709726316));
#72733=CARTESIAN_POINT('Ctrl Pts',(7.81073378077975,2.23877765047939,6.67215499056025));
#72734=CARTESIAN_POINT('Ctrl Pts',(7.83608926861664,2.15031644695909,6.66854915065635));
#72735=CARTESIAN_POINT('Ctrl Pts',(7.85994020024479,2.06142999144596,6.66494331075246));
#72736=CARTESIAN_POINT('Ctrl Pts',(7.88227318895816,1.97217061562417,6.66133747084856));
#72737=CARTESIAN_POINT('Ctrl Pts',(7.93319763694886,1.76863832086244,6.65311531084099));
#72738=CARTESIAN_POINT('Ctrl Pts',(7.97624300383516,1.56309896572517,6.64489315083341));
#72739=CARTESIAN_POINT('Ctrl Pts',(8.01127135890826,1.35617800322678,6.63667099082583));
#72740=CARTESIAN_POINT('Ctrl Pts',(8.04629325723027,1.14929518231821,6.628450346403));
#72741=CARTESIAN_POINT('Ctrl Pts',(8.07330104392661,0.941031553192318,6.62022970198017));
#72742=CARTESIAN_POINT('Ctrl Pts',(8.09220808537406,0.732021765732926,6.61200905755734));
#72743=CARTESIAN_POINT('Ctrl Pts',(8.11111300274323,0.523035459109987,6.60378933666833));
#72744=CARTESIAN_POINT('Ctrl Pts',(8.12191896516244,0.313303455333208,6.59556961577933));
#72745=CARTESIAN_POINT('Ctrl Pts',(8.12459121942834,0.103465355012618,6.58734989489032));
#72746=CARTESIAN_POINT('Ctrl Pts',(8.12726368781179,-0.106389558834649,
6.57912951538642));
#72747=CARTESIAN_POINT('Ctrl Pts',(8.12180113934578,-0.316350291117155,
6.57090913588252));
#72748=CARTESIAN_POINT('Ctrl Pts',(8.10822093952032,-0.52577633878319,6.56268875637863));
#72749=CARTESIAN_POINT('Ctrl Pts',(8.09464078995146,-0.735201611420664,
6.55446840729611));
#72750=CARTESIAN_POINT('Ctrl Pts',(8.07294307087896,-0.944091909047287,
6.54624805821359));
#72751=CARTESIAN_POINT('Ctrl Pts',(8.04319714669472,-1.15181041057196,6.53802770913107));
#72752=CARTESIAN_POINT('Ctrl Pts',(8.01344486243466,-1.35957332508609,6.52980560242814));
#72753=CARTESIAN_POINT('Ctrl Pts',(7.9756409770586,-1.56616365073405,6.52158349572522));
#72754=CARTESIAN_POINT('Ctrl Pts',(7.92990641515993,-1.77095223236128,6.5133613890223));
#72755=CARTESIAN_POINT('Ctrl Pts',(7.90984932830451,-1.8607631368102,6.50975554911854));
#72756=CARTESIAN_POINT('Ctrl Pts',(7.88826759828174,-1.95022764285475,6.50614970921479));
#72757=CARTESIAN_POINT('Ctrl Pts',(7.86517450686964,-2.03929339208167,6.50254386931103));
#72758=CARTESIAN_POINT('Ctrl Pts',(7.81251684659427,-2.24238417283806,6.49432170930347));
#72759=CARTESIAN_POINT('Ctrl Pts',(7.75198012259201,-2.44346782500171,6.48609954929591));
#72760=CARTESIAN_POINT('Ctrl Pts',(7.68374244915463,-2.64192913182,6.47787738928836));
#72761=CARTESIAN_POINT('Ctrl Pts',(7.6155173539177,-2.84035385641074,6.46965674486554));
#72762=CARTESIAN_POINT('Ctrl Pts',(7.53959423830998,-3.03615692144081,6.46143610044273));
#72763=CARTESIAN_POINT('Ctrl Pts',(7.45620066198893,-3.22873957615907,6.45321545601991));
#72764=CARTESIAN_POINT('Ctrl Pts',(7.37281645437288,-3.42130059551691,6.44499573513097));
#72765=CARTESIAN_POINT('Ctrl Pts',(7.2819635787938,-3.61064165611998,6.43677601424204));
#72766=CARTESIAN_POINT('Ctrl Pts',(7.18391752103794,-3.79618448095243,6.4285562933531));
#72767=CARTESIAN_POINT('Ctrl Pts',(7.08586360722461,-3.98174217262531,6.4203359138492));
#72768=CARTESIAN_POINT('Ctrl Pts',(6.98061549508917,-4.16350075819488,6.41211553434531));
#72769=CARTESIAN_POINT('Ctrl Pts',(6.86849486896408,-4.34090610328237,6.40389515484141));
#72770=CARTESIAN_POINT('Ctrl Pts',(6.75637465776682,-4.51831079184111,6.3956748057589));
#72771=CARTESIAN_POINT('Ctrl Pts',(6.63738214339274,-4.69136202407706,6.38745445667638));
#72772=CARTESIAN_POINT('Ctrl Pts',(6.51188291021747,-4.85953377662072,6.37923410759387));
#72773=CARTESIAN_POINT('Ctrl Pts',(6.38635684363019,-5.0277414865309,6.37101200089094));
#72774=CARTESIAN_POINT('Ctrl Pts',(6.25432145540267,-5.19106739585481,6.36278989418801));
#72775=CARTESIAN_POINT('Ctrl Pts',(6.11618393866971,-5.34901688077899,6.35456778748508));
#72776=CARTESIAN_POINT('Ctrl Pts',(6.05560314252433,-5.41828629993294,6.35096194758123));
#72777=CARTESIAN_POINT('Ctrl Pts',(5.99384924426072,-5.48652210404114,6.34735610767737));
#72778=CARTESIAN_POINT('Ctrl Pts',(5.93095895674036,-5.55368467019521,6.34375026777352));
#72779=CARTESIAN_POINT('Ctrl Pts',(5.78755436288664,-5.70683106054015,6.33552810776595));
#72780=CARTESIAN_POINT('Ctrl Pts',(5.63819122501462,-5.85444536596324,6.32730594775838));
#72781=CARTESIAN_POINT('Ctrl Pts',(5.48332028749775,-5.9960725635382,6.31908378775082));
#72782=CARTESIAN_POINT('Ctrl Pts',(5.32847789722709,-6.13767365507582,6.31086314332797));
#72783=CARTESIAN_POINT('Ctrl Pts',(5.16812995130048,-6.27328964232015,6.30264249890511));
#72784=CARTESIAN_POINT('Ctrl Pts',(5.00276273555141,-6.40250361767005,6.29442185448227));
#72785=CARTESIAN_POINT('Ctrl Pts',(4.83741409769366,-6.53170307670136,6.28620213359337));
#72786=CARTESIAN_POINT('Ctrl Pts',(4.66704754823662,-6.65450177806621,6.27798241270448));
#72787=CARTESIAN_POINT('Ctrl Pts',(4.49218166297588,-6.77052372193786,6.26976269181559));
#72788=CARTESIAN_POINT('Ctrl Pts',(4.31730176637635,-6.88655496220691,6.2615423123117));
#72789=CARTESIAN_POINT('Ctrl Pts',(4.1379220580616,-6.99580819456734,6.25332193280781));
#72790=CARTESIAN_POINT('Ctrl Pts',(3.95459013144472,-7.09795072220003,6.24510155330392));
#72791=CARTESIAN_POINT('Ctrl Pts',(3.77125888328944,-7.20009287183102,6.23688120422142));
#72792=CARTESIAN_POINT('Ctrl Pts',(3.58397570521678,-7.29512422805787,6.22866085513891));
#72793=CARTESIAN_POINT('Ctrl Pts',(3.3933132912971,-7.38275778213036,6.22044050605641));
#72794=CARTESIAN_POINT('Ctrl Pts',(3.20261011120727,-7.47041007342695,6.2122183993535));
#72795=CARTESIAN_POINT('Ctrl Pts',(3.00852652003218,-7.55066127925759,6.20399629265059));
#72796=CARTESIAN_POINT('Ctrl Pts',(2.81165672712676,-7.62327187048336,6.19577418594768));
#72797=CARTESIAN_POINT('Ctrl Pts',(2.7253186411861,-7.65511555443778,6.19216834604379));
#72798=CARTESIAN_POINT('Ctrl Pts',(2.63844493492152,-7.68549034782062,6.18856250613991));
#72799=CARTESIAN_POINT('Ctrl Pts',(2.55108680360857,-7.71437902121449,6.18495666623602));
#72800=CARTESIAN_POINT('Ctrl Pts',(2.35188979188242,-7.78025196659809,6.17673450622844));
#72801=CARTESIAN_POINT('Ctrl Pts',(2.1501071362402,-7.83841630277248,6.16851234622086));
#72802=CARTESIAN_POINT('Ctrl Pts',(1.9463523433089,-7.88868811135261,6.16029018621328));
#72803=CARTESIAN_POINT('Ctrl Pts',(1.74263510834874,-7.93895065336723,6.15206954179041));
#72804=CARTESIAN_POINT('Ctrl Pts',(1.53694674804625,-7.98132350075102,6.14384889736755));
#72805=CARTESIAN_POINT('Ctrl Pts',(1.32991374343956,-8.0156732092514,6.13562825294468));
#72806=CARTESIAN_POINT('Ctrl Pts',(1.12290399759584,-8.05001905879348,6.12740853205581));
#72807=CARTESIAN_POINT('Ctrl Pts',(0.914550200080307,-8.07634352063609,
6.11918881116696));
#72808=CARTESIAN_POINT('Ctrl Pts',(0.70548761512801,-8.09456452117104,6.11096909027809));
#72809=CARTESIAN_POINT('Ctrl Pts',(0.496408278784366,-8.11278698168561,
6.1027487107742));
#72810=CARTESIAN_POINT('Ctrl Pts',(0.286620335328576,-8.12290465517997,
6.0945283312703));
#72811=CARTESIAN_POINT('Ctrl Pts',(0.0767638127118421,-8.12488737642301,
6.0863079517664));
#72812=CARTESIAN_POINT('Ctrl Pts',(-0.133091933283915,-8.12687009032854,
6.07808760268386));
#72813=CARTESIAN_POINT('Ctrl Pts',(-0.343015962777012,-8.12071791208522,
6.06986725360131));
#72814=CARTESIAN_POINT('Ctrl Pts',(-0.552368064768117,-8.10645280523635,
6.06164690451877));
#72815=CARTESIAN_POINT('Ctrl Pts',(-0.761764929032563,-8.09218464831727,
6.05342479781588));
#72816=CARTESIAN_POINT('Ctrl Pts',(-0.97058932697103,-8.06980011736266,
6.045202691113));
#72817=CARTESIAN_POINT('Ctrl Pts',(-1.17820487007173,-8.03937316254441,
6.03698058441012));
#72818=CARTESIAN_POINT('Ctrl Pts',(-1.26925555051546,-8.02602929195236,
6.03337474450623));
#72819=CARTESIAN_POINT('Ctrl Pts',(-1.36007381335723,-8.01113929371327,
6.02976890460236));
#72820=CARTESIAN_POINT('Ctrl Pts',(-1.45060645962936,-7.99471253152867,
6.02616306469848));
#72821=CARTESIAN_POINT('Ctrl Pts',(-1.65704210940815,-7.95725566414464,
6.01794090469093));
#72822=CARTESIAN_POINT('Ctrl Pts',(-1.86206025867977,-7.91179261772738,
6.00971874468338));
#72823=CARTESIAN_POINT('Ctrl Pts',(-2.06503417928948,-7.85845540808537,
6.00149658467583));
#72824=CARTESIAN_POINT('Ctrl Pts',(-2.26797068586497,-7.80512803005217,
5.99327594025302));
#72825=CARTESIAN_POINT('Ctrl Pts',(-2.46886343053342,-7.74392946063848,
5.98505529583021));
#72826=CARTESIAN_POINT('Ctrl Pts',(-2.66709844025841,-7.67504224564732,
5.9768346514074));
#72827=CARTESIAN_POINT('Ctrl Pts',(-2.86531117961673,-7.60616276967027,
5.96861493051856));
#72828=CARTESIAN_POINT('Ctrl Pts',(-3.0608665014427,-7.52959646940878,5.96039520962973));
#72829=CARTESIAN_POINT('Ctrl Pts',(-3.25316729715076,-7.4455752027126,5.95217548874089));
#72830=CARTESIAN_POINT('Ctrl Pts',(-3.4454835011922,-7.36154720371101,5.94395510923699));
#72831=CARTESIAN_POINT('Ctrl Pts',(-3.63454438650858,-7.27006316040427,
5.93573472973309));
#72832=CARTESIAN_POINT('Ctrl Pts',(-3.81977349584356,-7.1714027918498,5.92751435022919));
#72833=CARTESIAN_POINT('Ctrl Pts',(-4.0050019196957,-7.07274278841067,5.9192940011467));
#72834=CARTESIAN_POINT('Ctrl Pts',(-4.18639833669129,-6.9669066539555,5.9110736520642));
#72835=CARTESIAN_POINT('Ctrl Pts',(-4.3634110687525,-6.85421997076168,5.9028533029817));
#72836=CARTESIAN_POINT('Ctrl Pts',(-4.54046164849956,-6.74150919365022,
5.8946311962788));
#72837=CARTESIAN_POINT('Ctrl Pts',(-4.71312642176304,-6.62194510006658,
5.8864090895759));
#72838=CARTESIAN_POINT('Ctrl Pts',(-4.88088193900288,-6.49589709432158,
5.878186982873));
#72839=CARTESIAN_POINT('Ctrl Pts',(-4.95445183538576,-6.44061820469394,
5.87458114296899));
#72840=CARTESIAN_POINT('Ctrl Pts',(-5.02707792745737,-6.38409281514049,
5.87097530306498));
#72841=CARTESIAN_POINT('Ctrl Pts',(-5.09871797967501,-6.32635460010255,
5.86736946316097));
#72842=CARTESIAN_POINT('Ctrl Pts',(-5.26207408753466,-6.19469793889987,
5.85914730315339));
#72843=CARTESIAN_POINT('Ctrl Pts',(-5.42035506271293,-6.05668901521307,
5.85092514314583));
#72844=CARTESIAN_POINT('Ctrl Pts',(-5.57307371896767,-5.91274360051675,
5.84270298313825));
#72845=CARTESIAN_POINT('Ctrl Pts',(-5.72576422470408,-5.76882471917357,
5.83448233871543));
#72846=CARTESIAN_POINT('Ctrl Pts',(-5.87289424320319,-5.61897173316621,
5.8262616942926));
#72847=CARTESIAN_POINT('Ctrl Pts',(-6.01401196384205,-5.46363868326454,
5.81804104986978));
#72848=CARTESIAN_POINT('Ctrl Pts',(-6.15511383085854,-5.30832308398143,
5.8098213289808));
#72849=CARTESIAN_POINT('Ctrl Pts',(-6.29020455010105,-5.14752886827035,
5.80160160809184));
#72850=CARTESIAN_POINT('Ctrl Pts',(-6.41887071237704,-4.98174531066054,
5.79338188720287));
#72851=CARTESIAN_POINT('Ctrl Pts',(-6.54754718418195,-4.81594846944647,
5.785161507699));
#72852=CARTESIAN_POINT('Ctrl Pts',(-6.66979788732694,-4.64516171903379,
5.77694112819514));
#72853=CARTESIAN_POINT('Ctrl Pts',(-6.78525044528358,-4.46990648193885,
5.76872074869128));
#72854=CARTESIAN_POINT('Ctrl Pts',(-6.9007025759817,-4.29465189341588,5.76050039960881));
#72855=CARTESIAN_POINT('Ctrl Pts',(-7.00935645168,-4.11492909922792,5.75228005052633));
#72856=CARTESIAN_POINT('Ctrl Pts',(-7.11088339739159,-3.93128794051016,
5.74405970144386));
#72857=CARTESIAN_POINT('Ctrl Pts',(-7.21243205092006,-3.74760751686015,
5.73583759474098));
#72858=CARTESIAN_POINT('Ctrl Pts',(-7.3068505873098,-3.56000731327155,5.72761548803809));
#72859=CARTESIAN_POINT('Ctrl Pts',(-7.39385608552553,-3.36906214680541,
5.7193933813352));
#72860=CARTESIAN_POINT('Ctrl Pts',(-7.43201271723356,-3.28532233101569,
5.71578754143129));
#72861=CARTESIAN_POINT('Ctrl Pts',(-7.46874420789188,-3.20093947430102,
5.71218170152737));
#72862=CARTESIAN_POINT('Ctrl Pts',(-7.50402958019199,-3.11596335378059,
5.70857586162345));
#72863=CARTESIAN_POINT('Ctrl Pts',(-7.58418660423391,-2.92292492194509,
5.70038455239166));
#72864=CARTESIAN_POINT('Ctrl Pts',(-7.65690599965396,-2.72675532862698,
5.69219324315985));
#72865=CARTESIAN_POINT('Ctrl Pts',(-7.72195962781729,-2.52804807487117,
5.68400193392806));
#72866=CARTESIAN_POINT('Ctrl Pts',(-7.78860742395512,-2.3244714118421,5.67560989303508));
#72867=CARTESIAN_POINT('Ctrl Pts',(-7.84720881983712,-2.11823142459329,
5.66721785214211));
#72868=CARTESIAN_POINT('Ctrl Pts',(-7.89757210617641,-1.9099849188526,5.65882581124914));
#72869=CARTESIAN_POINT('Ctrl Pts',(-7.9467185781731,-1.70676980310642,5.65063652828688));
#72870=CARTESIAN_POINT('Ctrl Pts',(-7.98802034313663,-1.50164430971879,
5.64244724532462));
#72871=CARTESIAN_POINT('Ctrl Pts',(-8.02135041567727,-1.29523166708281,
5.63425796236236));
#72872=CARTESIAN_POINT('Ctrl Pts',(-8.05591831390485,-1.0811531884108,5.62576454250403));
#72873=CARTESIAN_POINT('Ctrl Pts',(-8.0819110099373,-0.865690460132721,
5.61727112264571));
#72874=CARTESIAN_POINT('Ctrl Pts',(-8.09924532175734,-0.649548135623411,
5.60877770278738));
#72875=CARTESIAN_POINT('Ctrl Pts',(-8.11657963357738,-0.433405811114101,
5.60028428292905));
#72876=CARTESIAN_POINT('Ctrl Pts',(-8.12525553763274,-0.216584249013234,
5.59179086307072));
#72877=CARTESIAN_POINT('Ctrl Pts',(-8.12524999734671,0.000207647102394412,
5.58329744321239));
#72878=CARTESIAN_POINT('Origin',(0.,0.,24.4167025567876));
#72879=CARTESIAN_POINT('',(4.9467595481762,6.44587135576158,8.87494054454767));
#72880=CARTESIAN_POINT('',(4.94675954817621,6.44587135576157,8.70834331018201));
#72881=CARTESIAN_POINT('',(4.9467595481762,6.44587135576158,24.4167025567876));
#72882=CARTESIAN_POINT('',(-8.12524999753662,-0.000200077936422182,7.41670255682301));
#72883=CARTESIAN_POINT('Ctrl Pts',(4.94675954817621,6.44587135576157,8.708343310182));
#72884=CARTESIAN_POINT('Ctrl Pts',(5.11321786853059,6.31812613092856,8.70012269712016));
#72885=CARTESIAN_POINT('Ctrl Pts',(5.27474386885071,6.18391519945133,8.69190208405833));
#72886=CARTESIAN_POINT('Ctrl Pts',(5.43084219160774,6.04364464974184,8.68368147099649));
#72887=CARTESIAN_POINT('Ctrl Pts',(5.58692326850953,5.90338959722383,8.67546176615391));
#72888=CARTESIAN_POINT('Ctrl Pts',(5.73757764558412,5.75707646023444,8.66724206131133));
#72889=CARTESIAN_POINT('Ctrl Pts',(5.88234461276443,5.60515025839462,8.65902235646874));
#72890=CARTESIAN_POINT('Ctrl Pts',(6.0271233166663,5.45321173941117,8.65080198522837));
#72891=CARTESIAN_POINT('Ctrl Pts',(6.16601345141907,5.2956594581423,8.642581613988));
#72892=CARTESIAN_POINT('Ctrl Pts',(6.29859188485475,5.13297455970141,8.63436124274763));
#72893=CARTESIAN_POINT('Ctrl Pts',(6.43117007521497,4.97028995953456,8.62614088657887));
#72894=CARTESIAN_POINT('Ctrl Pts',(6.55743640308595,4.80247299154491,8.61792053041011));
#72895=CARTESIAN_POINT('Ctrl Pts',(6.67700834462886,4.63003748670101,8.60970017424135));
#72896=CARTESIAN_POINT('Ctrl Pts',(6.79660566708931,4.45756537986442,8.6014780731801));
#72897=CARTESIAN_POINT('Ctrl Pts',(6.90950559627171,4.28047302027635,8.59325597211886));
#72898=CARTESIAN_POINT('Ctrl Pts',(7.01536860951096,4.09930370126297,8.58503387105761));
#72899=CARTESIAN_POINT('Ctrl Pts',(7.05905657855677,4.02453802665272,8.58164074171372));
#72900=CARTESIAN_POINT('Ctrl Pts',(7.10154662717555,3.94907833495743,8.57824761236983));
#72901=CARTESIAN_POINT('Ctrl Pts',(7.14281713462611,3.87296410308586,8.57485448302593));
#72902=CARTESIAN_POINT('Ctrl Pts',(7.24282296448423,3.68852568949356,8.56663232301836));
#72903=CARTESIAN_POINT('Ctrl Pts',(7.33569775733754,3.50018131614254,8.55841016301079));
#72904=CARTESIAN_POINT('Ctrl Pts',(7.42115217109695,3.30850238263825,8.55018800300323));
#72905=CARTESIAN_POINT('Ctrl Pts',(7.50659083310692,3.11685878117127,8.54196735858038));
#72906=CARTESIAN_POINT('Ctrl Pts',(7.58461172583095,2.9218821157531,8.53374671415755));
#72907=CARTESIAN_POINT('Ctrl Pts',(7.65497289788578,2.72416546764954,8.52552606973471));
#72908=CARTESIAN_POINT('Ctrl Pts',(7.72532616533749,2.52647103167784,8.51730634884582));
#72909=CARTESIAN_POINT('Ctrl Pts',(7.78802133116929,2.32603750551014,8.50908662795694));
#72910=CARTESIAN_POINT('Ctrl Pts',(7.84286545707911,2.12347568496917,8.50086690706805));
#72911=CARTESIAN_POINT('Ctrl Pts',(7.89771397744039,1.92089763391905,8.49264652756416));
#72912=CARTESIAN_POINT('Ctrl Pts',(7.94471012115541,1.71619123193746,8.48442614806026));
#72913=CARTESIAN_POINT('Ctrl Pts',(7.98371120191593,1.50998112799536,8.47620576855636));
#72914=CARTESIAN_POINT('Ctrl Pts',(8.02271213834406,1.30377178718071,8.46798541947385));
#72915=CARTESIAN_POINT('Ctrl Pts',(8.05371801877767,1.09605904603583,8.45976507039135));
#72916=CARTESIAN_POINT('Ctrl Pts',(8.0766374345402,0.887476936874398,8.45154472130884));
#72917=CARTESIAN_POINT('Ctrl Pts',(8.09956175077984,0.678850230072898,8.44332261460593));
#72918=CARTESIAN_POINT('Ctrl Pts',(8.11439611591062,0.46935407733536,8.43510050790302));
#72919=CARTESIAN_POINT('Ctrl Pts',(8.12110096613918,0.259627926605015,8.42687840120012));
#72920=CARTESIAN_POINT('Ctrl Pts',(8.12404140675585,0.167651630198292,8.42327256129622));
#72921=CARTESIAN_POINT('Ctrl Pts',(8.12541897333413,0.0756311367006419,
8.41966672139232));
#72922=CARTESIAN_POINT('Ctrl Pts',(8.12523349038375,-0.0163795374249914,
8.41606088148843));
#72923=CARTESIAN_POINT('Ctrl Pts',(8.12481054578905,-0.226185437084521,
8.40783872148086));
#72924=CARTESIAN_POINT('Ctrl Pts',(8.11625692606618,-0.436009567513309,
8.39961656147329));
#72925=CARTESIAN_POINT('Ctrl Pts',(8.09959192648282,-0.645211738078572,
8.39139440146571));
#72926=CARTESIAN_POINT('Ctrl Pts',(8.08292999874661,-0.854375346561104,
8.38317375704287));
#72927=CARTESIAN_POINT('Ctrl Pts',(8.05815969871724,-1.06291692993365,8.37495311262003));
#72928=CARTESIAN_POINT('Ctrl Pts',(8.02535230981967,-1.27019993141711,8.36673246819718));
#72929=CARTESIAN_POINT('Ctrl Pts',(7.99254860661099,-1.47745964605331,8.3585127473083));
#72930=CARTESIAN_POINT('Ctrl Pts',(7.95170966325661,-1.68346076968223,8.35029302641941));
#72931=CARTESIAN_POINT('Ctrl Pts',(7.90295827801188,-1.88757463918743,8.34207330553052));
#72932=CARTESIAN_POINT('Ctrl Pts',(7.85420298650384,-2.09170486356159,8.33385292602663));
#72933=CARTESIAN_POINT('Ctrl Pts',(7.79753405223371,-2.2939472439496,8.32563254652274));
#72934=CARTESIAN_POINT('Ctrl Pts',(7.7331250287989,-2.49368499443374,8.31741216701884));
#72935=CARTESIAN_POINT('Ctrl Pts',(7.66871624372434,-2.69342200574288,8.30919181793633));
#72936=CARTESIAN_POINT('Ctrl Pts',(7.59656751990552,-2.89065412560853,8.30097146885382));
#72937=CARTESIAN_POINT('Ctrl Pts',(7.51690192843684,-3.08478086106007,8.29275111977131));
#72938=CARTESIAN_POINT('Ctrl Pts',(7.43721930340095,-3.27894910339977,8.28452901306841));
#72939=CARTESIAN_POINT('Ctrl Pts',(7.35001671190377,-3.47001036173554,8.2763069063655));
#72940=CARTESIAN_POINT('Ctrl Pts',(7.25556534238605,-3.65738419158643,8.26808479966259));
#72941=CARTESIAN_POINT('Ctrl Pts',(7.21414329211456,-3.73955778249652,8.26447895975869));
#72942=CARTESIAN_POINT('Ctrl Pts',(7.17132769597844,-3.82102245975466,8.26087311985478));
#72943=CARTESIAN_POINT('Ctrl Pts',(7.1271442429179,-3.90173070612801,8.25726727995088));
#72944=CARTESIAN_POINT('Ctrl Pts',(7.02639561557108,-4.08576442179398,8.24904511994331));
#72945=CARTESIAN_POINT('Ctrl Pts',(6.91849850696173,-4.26592419553473,8.24082295993573));
#72946=CARTESIAN_POINT('Ctrl Pts',(6.80377614654044,-4.44165709057637,8.23260079992816));
#72947=CARTESIAN_POINT('Ctrl Pts',(6.68907493280776,-4.61735759290226,8.22438015550532));
#72948=CARTESIAN_POINT('Ctrl Pts',(6.56755113950271,-4.78863259814186,8.21615951108247));
#72949=CARTESIAN_POINT('Ctrl Pts',(6.43957190969968,-4.9549572331461,8.20793886665963));
#72950=CARTESIAN_POINT('Ctrl Pts',(6.31160705749997,-5.12126318269934,8.19971914577075));
#72951=CARTESIAN_POINT('Ctrl Pts',(6.17718839657641,-5.28261963849276,8.19149942488187));
#72952=CARTESIAN_POINT('Ctrl Pts',(6.03672452997019,-5.43853330519877,8.18327970399298));
#72953=CARTESIAN_POINT('Ctrl Pts',(5.89624940852793,-5.59445946467459,8.17505932448909));
#72954=CARTESIAN_POINT('Ctrl Pts',(5.74972830909333,-5.74494174255745,8.1668389449852));
#72955=CARTESIAN_POINT('Ctrl Pts',(5.59760872190857,-5.88952155602754,8.1586185654813));
#72956=CARTESIAN_POINT('Ctrl Pts',(5.44548969767696,-6.03410083444713,8.15039821639879));
#72957=CARTESIAN_POINT('Ctrl Pts',(5.28777244291146,-6.17277749075465,8.14217786731628));
#72958=CARTESIAN_POINT('Ctrl Pts',(5.12494013544889,-6.30513094000157,8.13395751823377));
#72959=CARTESIAN_POINT('Ctrl Pts',(4.96207301226475,-6.4375126881832,8.12573541153087));
#72960=CARTESIAN_POINT('Ctrl Pts',(4.7940888805261,-6.56356834210117,8.11751330482795));
#72961=CARTESIAN_POINT('Ctrl Pts',(4.62150357939489,-6.68291794264603,8.10929119812504));
#72962=CARTESIAN_POINT('Ctrl Pts',(4.54581556072405,-6.73525921814972,8.10568535822116));
#72963=CARTESIAN_POINT('Ctrl Pts',(4.46924299772639,-6.78631126521106,8.10207951831727));
#72964=CARTESIAN_POINT('Ctrl Pts',(4.39183118215686,-6.83604464803549,8.09847367841338));
#72965=CARTESIAN_POINT('Ctrl Pts',(4.21531410123973,-6.94944841586751,8.09025151840582));
#72966=CARTESIAN_POINT('Ctrl Pts',(4.03437315758485,-7.05603033285991,8.08202935839825));
#72967=CARTESIAN_POINT('Ctrl Pts',(3.84955672844517,-7.15545949307118,8.07380719839069));
#72968=CARTESIAN_POINT('Ctrl Pts',(3.66477436638238,-7.25487032557825,8.06558655396785));
#72969=CARTESIAN_POINT('Ctrl Pts',(3.4761182043948,-7.34713089301159,8.05736590954501));
#72970=CARTESIAN_POINT('Ctrl Pts',(3.28416175498827,-7.43195594238639,8.04914526512217));
#72971=CARTESIAN_POINT('Ctrl Pts',(3.09222687059411,-7.51677146223903,8.04092554423329));
#72972=CARTESIAN_POINT('Ctrl Pts',(2.89699270884084,-7.59415301246364,8.03270582334441));
#72973=CARTESIAN_POINT('Ctrl Pts',(2.69905408157299,-7.66386290503974,8.02448610245552));
#72974=CARTESIAN_POINT('Ctrl Pts',(2.50109959423505,-7.73357838320465,8.01626572295164));
#72975=CARTESIAN_POINT('Ctrl Pts',(2.30044048588349,-7.79562087486791,8.00804534344775));
#72976=CARTESIAN_POINT('Ctrl Pts',(2.09768910876352,-7.84980177873779,7.99982496394386));
#72977=CARTESIAN_POINT('Ctrl Pts',(1.89493848197112,-7.90398248209891,7.99160461486136));
#72978=CARTESIAN_POINT('Ctrl Pts',(1.69009588772657,-7.95030158224647,7.98338426577886));
#72979=CARTESIAN_POINT('Ctrl Pts',(1.48378683720432,-7.98862091879688,7.97516391669636));
#72980=CARTESIAN_POINT('Ctrl Pts',(1.27743367505221,-8.02694844853313,7.96694180999345));
#72981=CARTESIAN_POINT('Ctrl Pts',(1.06961372045437,-8.05727274360453,7.95871970329055));
#72982=CARTESIAN_POINT('Ctrl Pts',(0.860961728771738,-8.07950694436798,
7.95049759658764));
#72983=CARTESIAN_POINT('Ctrl Pts',(0.769456509388262,-8.08925784778504,
7.94689175668371));
#72984=CARTESIAN_POINT('Ctrl Pts',(0.677791352711616,-8.0974534542192,7.94328591677978));
#72985=CARTESIAN_POINT('Ctrl Pts',(0.586020113558015,-8.10408958421644,
7.93968007687586));
#72986=CARTESIAN_POINT('Ctrl Pts',(0.376760181747902,-8.11922151578361,
7.93145791686828));
#72987=CARTESIAN_POINT('Ctrl Pts',(0.166879311345257,-8.12624649689666,
7.92323575686071));
#72988=CARTESIAN_POINT('Ctrl Pts',(-0.0429826381961779,-8.12513630995282,
7.91501359685313));
#72989=CARTESIAN_POINT('Ctrl Pts',(-0.252805904038364,-8.12402632764892,
7.90679295243028));
#72990=CARTESIAN_POINT('Ctrl Pts',(-0.462609960989967,-8.11478417174254,
7.89857230800743));
#72991=CARTESIAN_POINT('Ctrl Pts',(-0.671754719371072,-8.09743373912394,
7.89035166358458));
#72992=CARTESIAN_POINT('Ctrl Pts',(-0.88087598174945,-8.0800852557094,7.88213194269567));
#72993=CARTESIAN_POINT('Ctrl Pts',(-1.08933779941136,-8.05463033854202,
7.87391222180677));
#72994=CARTESIAN_POINT('Ctrl Pts',(-1.29650413562753,-8.02114484277654,
7.86569250091787));
#72995=CARTESIAN_POINT('Ctrl Pts',(-1.50368707129472,-7.98765666394558,
7.85747212141397));
#72996=CARTESIAN_POINT('Ctrl Pts',(-1.70957402630208,-7.9461366652205,7.84925174191007));
#72997=CARTESIAN_POINT('Ctrl Pts',(-1.91353704574931,-7.89671219793687,
7.84103136240618));
#72998=CARTESIAN_POINT('Ctrl Pts',(-2.11749931038528,-7.84728791355966,
7.83281101332366));
#72999=CARTESIAN_POINT('Ctrl Pts',(-2.31953736748993,-7.78995929124146,
7.82459066424115));
#73000=CARTESIAN_POINT('Ctrl Pts',(-2.51903583935572,-7.72490427141602,
7.81637031515863));
#73001=CARTESIAN_POINT('Ctrl Pts',(-2.71857696665826,-7.6598353419588,7.80814820845572));
#73002=CARTESIAN_POINT('Ctrl Pts',(-2.91557714326042,-7.58703680612623,
7.79992610175281));
#73003=CARTESIAN_POINT('Ctrl Pts',(-3.10943741765436,-7.50673607556513,
7.7917039950499));
#73004=CARTESIAN_POINT('Ctrl Pts',(-3.19445566643648,-7.47151984826135,
7.78809815514605));
#73005=CARTESIAN_POINT('Ctrl Pts',(-3.2788702611578,-7.43486135523398,7.78449231524221));
#73006=CARTESIAN_POINT('Ctrl Pts',(-3.3626319109193,-7.39678269210115,7.78088647533836));
#73007=CARTESIAN_POINT('Ctrl Pts',(-3.55362810187657,-7.30995441644249,
7.77266431533079));
#73008=CARTESIAN_POINT('Ctrl Pts',(-3.74129095503225,-7.21571013987357,
7.76444215532323));
#73009=CARTESIAN_POINT('Ctrl Pts',(-3.9250450928939,-7.11433121110126,7.75621999531566));
#73010=CARTESIAN_POINT('Ctrl Pts',(-4.10876535949,-7.01297096943259,7.74799935089282));
#73011=CARTESIAN_POINT('Ctrl Pts',(-4.2885780904998,-6.90447884287115,7.73977870646998));
#73012=CARTESIAN_POINT('Ctrl Pts',(-4.46393263934849,-6.78918205337426,
7.73155806204714));
#73013=CARTESIAN_POINT('Ctrl Pts',(-4.63926748829637,-6.67389821669402,
7.72333834115826));
#73014=CARTESIAN_POINT('Ctrl Pts',(-4.81014490847376,-6.55181140534979,
7.71511862026937));
#73015=CARTESIAN_POINT('Ctrl Pts',(-4.97604267064916,-6.42329252816488,
7.70689889938048));
#73016=CARTESIAN_POINT('Ctrl Pts',(-5.141953725582,-6.29476335325058,7.69867851987659));
#73017=CARTESIAN_POINT('Ctrl Pts',(-5.3028840902678,-6.15980126131947,7.6904581403727));
#73018=CARTESIAN_POINT('Ctrl Pts',(-5.45834326960779,-6.0188185147608,7.6822377608688));
#73019=CARTESIAN_POINT('Ctrl Pts',(-5.61380187363556,-5.87783628994099,
7.6740174117863));
#73020=CARTESIAN_POINT('Ctrl Pts',(-5.76378911598376,-5.73083365531125,
7.6657970627038));
#73021=CARTESIAN_POINT('Ctrl Pts',(-5.90784974920863,-5.57826127958126,
7.6575767136213));
#73022=CARTESIAN_POINT('Ctrl Pts',(-6.05194118452063,-5.42565628183991,
7.64935460691839));
#73023=CARTESIAN_POINT('Ctrl Pts',(-6.1901032764461,-5.26747937848341,7.64113250021548));
#73024=CARTESIAN_POINT('Ctrl Pts',(-6.32191887028163,-5.104216821421,7.63291039351257));
#73025=CARTESIAN_POINT('Ctrl Pts',(-6.37972716022301,-5.03261733185672,
7.62930455360866));
#73026=CARTESIAN_POINT('Ctrl Pts',(-6.43631534393656,-4.96004015653743,
7.62569871370474));
#73027=CARTESIAN_POINT('Ctrl Pts',(-6.4916507089754,-4.88652828040104,7.62209287380082));
#73028=CARTESIAN_POINT('Ctrl Pts',(-6.61782830907694,-4.71890397534152,
7.61387071379325));
#73029=CARTESIAN_POINT('Ctrl Pts',(-6.73753078784233,-4.54636225082834,
7.60564855378568));
#73030=CARTESIAN_POINT('Ctrl Pts',(-6.85038749658374,-4.36942544382544,
7.59742639377811));
#73031=CARTESIAN_POINT('Ctrl Pts',(-6.96322340253104,-4.19252125145402,
7.58920574935524));
#73032=CARTESIAN_POINT('Ctrl Pts',(-7.06921589834827,-4.0112238422345,7.58098510493238));
#73033=CARTESIAN_POINT('Ctrl Pts',(-7.16803799930891,-3.82608400364701,
7.57276446050952));
#73034=CARTESIAN_POINT('Ctrl Pts',(-7.26684899827252,-3.64096496427262,
7.56454473962066));
#73035=CARTESIAN_POINT('Ctrl Pts',(-7.35849107166973,-3.45200461760183,
7.55632501873179));
#73036=CARTESIAN_POINT('Ctrl Pts',(-7.44268308985259,-3.25977851801656,
7.54810529784292));
#73037=CARTESIAN_POINT('Ctrl Pts',(-7.52688185402229,-3.0675370160836,7.53988491833902));
#73038=CARTESIAN_POINT('Ctrl Pts',(-7.60362924930881,-2.87202950765201,
7.53166453883512));
#73039=CARTESIAN_POINT('Ctrl Pts',(-7.67269179738429,-2.67385267822515,
7.52344415933122));
#73040=CARTESIAN_POINT('Ctrl Pts',(-7.74175408987807,-2.47567658219683,
7.51522381024871));
#73041=CARTESIAN_POINT('Ctrl Pts',(-7.80313149744535,-2.2748314645172,7.5070034611662));
#73042=CARTESIAN_POINT('Ctrl Pts',(-7.85663986834665,-2.07193087278654,
7.49878311208368));
#73043=CARTESIAN_POINT('Ctrl Pts',(-7.91015968005217,-1.86898689819991,
7.49056100538076));
#73044=CARTESIAN_POINT('Ctrl Pts',(-7.95580701849676,-1.66398685699576,
7.48233889867785));
#73045=CARTESIAN_POINT('Ctrl Pts',(-7.99344820621045,-1.45755731864338,
7.47411679197493));
#73046=CARTESIAN_POINT('Ctrl Pts',(-8.00995590935653,-1.36702676563262,
7.47051095207106));
#73047=CARTESIAN_POINT('Ctrl Pts',(-8.02492445198856,-1.27622141532451,
7.46690511216719));
#73048=CARTESIAN_POINT('Ctrl Pts',(-8.03834567369,-1.18519466450424,7.46329927226332));
#73049=CARTESIAN_POINT('Ctrl Pts',(-8.07024341346567,-0.968854626698262,
7.45472940094421));
#73050=CARTESIAN_POINT('Ctrl Pts',(-8.09340493463014,-0.751214168910868,
7.44615952962511));
#73051=CARTESIAN_POINT('Ctrl Pts',(-8.1077516028081,-0.532964829667744,
7.43758965830601));
#73052=CARTESIAN_POINT('Ctrl Pts',(-8.11940717704868,-0.355653878793876,
7.430627291145));
#73053=CARTESIAN_POINT('Ctrl Pts',(-8.12524562079903,-0.177941250951312,
7.423664923984));
#73054=CARTESIAN_POINT('Ctrl Pts',(-8.12524999753662,-0.000200077936449244,
7.41670255682299));
#73055=CARTESIAN_POINT('Ctrl Pts',(-8.12524999753664,-0.000200077032885864,
7.41670255678761));
#73056=CARTESIAN_POINT('Ctrl Pts',(-8.12525515579502,0.209279933090809,
7.40849693555404));
#73057=CARTESIAN_POINT('Ctrl Pts',(-8.11715495148673,0.418776541723859,
7.40029131432047));
#73058=CARTESIAN_POINT('Ctrl Pts',(-8.10097160197948,0.627651707893815,
7.3920856930869));
#73059=CARTESIAN_POINT('Ctrl Pts',(-8.08478712724863,0.836541397093457,
7.38387950131887));
#73060=CARTESIAN_POINT('Ctrl Pts',(-8.06051840414201,1.04480926092786,7.37567330955084));
#73061=CARTESIAN_POINT('Ctrl Pts',(-8.02823964397931,1.25182098613935,7.36746711778281));
#73062=CARTESIAN_POINT('Ctrl Pts',(-7.99596128150152,1.45883016089853,7.35926102711775));
#73063=CARTESIAN_POINT('Ctrl Pts',(-7.95567312746925,1.6645829346883,7.35105493645269));
#73064=CARTESIAN_POINT('Ctrl Pts',(-7.90750085760631,1.86845330406072,7.34284884578763));
#73065=CARTESIAN_POINT('Ctrl Pts',(-7.85931743671705,2.07237086580882,7.33464085555808));
#73066=CARTESIAN_POINT('Ctrl Pts',(-7.80324632174305,2.27440486314619,7.32643286532853));
#73067=CARTESIAN_POINT('Ctrl Pts',(-7.73946386678466,2.47394151451377,7.31822487509899));
#73068=CARTESIAN_POINT('Ctrl Pts',(-7.7039275779358,2.58511302842863,7.31365180697459));
#73069=CARTESIAN_POINT('Ctrl Pts',(-7.6659984760938,2.69550958120614,7.3090787388502));
#73070=CARTESIAN_POINT('Ctrl Pts',(-7.62571372598687,2.80502722478685,7.30450567072581));
#73071=CARTESIAN_POINT('Ctrl Pts',(-7.55328365229577,3.00193476359422,7.29628351071824));
#73072=CARTESIAN_POINT('Ctrl Pts',(-7.4732108712274,3.19606791339749,7.28806135071066));
#73073=CARTESIAN_POINT('Ctrl Pts',(-7.38573330237192,3.38683202251519,7.27983919070309));
#73074=CARTESIAN_POINT('Ctrl Pts',(-7.29827185819268,3.57756096822429,7.27161854628026));
#73075=CARTESIAN_POINT('Ctrl Pts',(-7.2034084733784,3.76492184455805,7.26339790185742));
#73076=CARTESIAN_POINT('Ctrl Pts',(-7.10142864793773,3.94834126194145,7.25517725743459));
#73077=CARTESIAN_POINT('Ctrl Pts',(-6.99946027924215,4.13174007339124,7.24695753654567));
#73078=CARTESIAN_POINT('Ctrl Pts',(-6.89037720939769,4.31119805205013,7.23873781565676));
#73079=CARTESIAN_POINT('Ctrl Pts',(-6.7745106117521,4.48616690881627,7.23051809476784));
#73080=CARTESIAN_POINT('Ctrl Pts',(-6.65863473015665,4.66114978517155,7.22229771526395));
#73081=CARTESIAN_POINT('Ctrl Pts',(-6.5359743954019,4.83164257333042,7.21407733576005));
#73082=CARTESIAN_POINT('Ctrl Pts',(-6.40690437318145,4.99712556530336,7.20585695625616));
#73083=CARTESIAN_POINT('Ctrl Pts',(-6.27783482861379,5.16260794486907,7.19763660717364));
#73084=CARTESIAN_POINT('Ctrl Pts',(-6.14235582765208,5.323080334251,7.18941625809111));
#73085=CARTESIAN_POINT('Ctrl Pts',(-6.00088304967101,5.47805532891656,7.18119590900859));
#73086=CARTESIAN_POINT('Ctrl Pts',(-5.85938002292125,5.633063459305,7.17297380230569));
#73087=CARTESIAN_POINT('Ctrl Pts',(-5.71188085789198,5.78257162870153,7.16475169560278));
#73088=CARTESIAN_POINT('Ctrl Pts',(-5.55883954320356,5.92612778257577,7.15652958889988));
#73089=CARTESIAN_POINT('Ctrl Pts',(-5.49172262300483,5.98908494511211,7.15292374899601));
#73090=CARTESIAN_POINT('Ctrl Pts',(-5.42354025621363,6.05089783836143,7.14931790909214));
#73091=CARTESIAN_POINT('Ctrl Pts',(-5.35433288438774,6.11153065325406,7.14571206918827));
#73092=CARTESIAN_POINT('Ctrl Pts',(-5.19652385791237,6.24978768047856,7.1374899091807));
#73093=CARTESIAN_POINT('Ctrl Pts',(-5.03333091776804,6.38195195101942,7.12926774917313));
#73094=CARTESIAN_POINT('Ctrl Pts',(-4.8652474860031,6.50761511326849,7.12104558916556));
#73095=CARTESIAN_POINT('Ctrl Pts',(-4.6971950369337,6.63325511211915,7.1128249447427));
#73096=CARTESIAN_POINT('Ctrl Pts',(-4.52425413169958,6.75239621777111,7.10460430031985));
#73097=CARTESIAN_POINT('Ctrl Pts',(-4.34694980155426,6.86467151328214,7.096383655897));
#73098=CARTESIAN_POINT('Ctrl Pts',(-4.16966539035582,6.97693419542019,7.08816393500816));
#73099=CARTESIAN_POINT('Ctrl Pts',(-3.98801878215426,7.08233244948104,7.07994421411932));
#73100=CARTESIAN_POINT('Ctrl Pts',(-3.80256310636589,7.18054325135675,7.07172449323048));
#73101=CARTESIAN_POINT('Ctrl Pts',(-3.61709257071779,7.27876192249143,7.06350411372658));
#73102=CARTESIAN_POINT('Ctrl Pts',(-3.42781261720923,7.3697918501861,7.05528373422269));
#73103=CARTESIAN_POINT('Ctrl Pts',(-3.23530098080577,7.45335596400019,7.0470633547188));
#73104=CARTESIAN_POINT('Ctrl Pts',(-3.04279005683416,7.53691976856681,7.03884300563624));
#73105=CARTESIAN_POINT('Ctrl Pts',(-2.84704774569189,7.61301769944957,7.03062265655368));
#73106=CARTESIAN_POINT('Ctrl Pts',(-2.6486722548104,7.68142062701279,7.02240230747112));
#73107=CARTESIAN_POINT('Ctrl Pts',(-2.45025434860111,7.74983818003494,7.0141802007682));
#73108=CARTESIAN_POINT('Ctrl Pts',(-2.2492024169488,7.81055734652839,7.00595809406528));
#73109=CARTESIAN_POINT('Ctrl Pts',(-2.04613139517198,7.86339836687622,6.99773598736236));
#73110=CARTESIAN_POINT('Ctrl Pts',(-1.95707373390586,7.88657202134409,6.99413014745849));
#73111=CARTESIAN_POINT('Ctrl Pts',(-1.86762792765624,7.90823112237467,6.99052430755463));
#73112=CARTESIAN_POINT('Ctrl Pts',(-1.77784662131366,7.92836357349886,6.98691846765076));
#73113=CARTESIAN_POINT('Ctrl Pts',(-1.57312420264919,7.97427028009167,6.97869630764319));
#73114=CARTESIAN_POINT('Ctrl Pts',(-1.36658897968878,8.01225095672081,6.97047414763563));
#73115=CARTESIAN_POINT('Ctrl Pts',(-1.15886960653281,8.04218308654774,6.96225198762806));
#73116=CARTESIAN_POINT('Ctrl Pts',(-0.951188522136813,8.07210969900709,
6.95403134320523));
#73117=CARTESIAN_POINT('Ctrl Pts',(-0.742324015167708,8.09399068361679,
6.9458106987824));
#73118=CARTESIAN_POINT('Ctrl Pts',(-0.532912673052062,8.10775503116618,
6.93759005435956));
#73119=CARTESIAN_POINT('Ctrl Pts',(-0.323524856888564,8.12151783238394,
6.9293703334707));
#73120=CARTESIAN_POINT('Ctrl Pts',(-0.113590622617442,8.12716579763455,
6.92115061258183));
#73121=CARTESIAN_POINT('Ctrl Pts',(0.0962497682060561,8.12467990413286,
6.91293089169297));
#73122=CARTESIAN_POINT('Ctrl Pts',(0.306106972743071,8.12219381144596,6.90471051218908));
#73123=CARTESIAN_POINT('Ctrl Pts',(0.51587002364315,8.11157255854095,6.89649013268521));
#73124=CARTESIAN_POINT('Ctrl Pts',(0.724899038140248,8.09284924776208,6.88826975318133));
#73125=CARTESIAN_POINT('Ctrl Pts',(0.933927279078422,8.07412600627305,6.88004940409881));
#73126=CARTESIAN_POINT('Ctrl Pts',(1.14222119531879,8.04730079587844,6.87182905501629));
#73127=CARTESIAN_POINT('Ctrl Pts',(1.34914586295771,8.01245861162253,6.86360870593378));
#73128=CARTESIAN_POINT('Ctrl Pts',(1.55611477385339,7.97760897764243,6.85538659923087));
#73129=CARTESIAN_POINT('Ctrl Pts',(1.7617135601569,7.934738994307,6.84716449252797));
#73130=CARTESIAN_POINT('Ctrl Pts',(1.96531622881724,7.88398501287563,6.83894238582506));
#73131=CARTESIAN_POINT('Ctrl Pts',(2.05460704608971,7.86172663821062,6.83533654592113));
#73132=CARTESIAN_POINT('Ctrl Pts',(2.14351409735526,7.83795259461911,6.83173070601718));
#73133=CARTESIAN_POINT('Ctrl Pts',(2.23198536645265,7.81267744671705,6.82812486611325));
#73134=CARTESIAN_POINT('Ctrl Pts',(2.43371860631164,7.75504475390934,6.81990278708515));
#73135=CARTESIAN_POINT('Ctrl Pts',(2.63325171788618,7.68958486235625,6.81168070805706));
#73136=CARTESIAN_POINT('Ctrl Pts',(2.82997406587421,7.61649094721312,6.80345862902897));
#73137=CARTESIAN_POINT('Ctrl Pts',(3.02667271421202,7.54340583788306,6.79523754053601));
#73138=CARTESIAN_POINT('Ctrl Pts',(3.22056099735752,7.46268864090862,6.78701645204305));
#73139=CARTESIAN_POINT('Ctrl Pts',(3.41104584256796,7.37458160320976,6.77879536355009));
#73140=CARTESIAN_POINT('Ctrl Pts',(3.60150474063423,7.28648656712714,6.77057539490353));
#73141=CARTESIAN_POINT('Ctrl Pts',(3.78856085885258,7.19100382461239,6.76235542625698));
#73142=CARTESIAN_POINT('Ctrl Pts',(3.97164281543318,7.08842301990492,6.75413545761042));
#73143=CARTESIAN_POINT('Ctrl Pts',(4.15473889057928,6.9858343045664,6.74591485507198));
#73144=CARTESIAN_POINT('Ctrl Pts',(4.33385993290286,6.87614657530239,6.73769425253354));
#73145=CARTESIAN_POINT('Ctrl Pts',(4.50845983964032,6.75969506981272,6.7294736499951));
#73146=CARTESIAN_POINT('Ctrl Pts',(4.65798384865252,6.65996823557962,6.72243368376022));
#73147=CARTESIAN_POINT('Ctrl Pts',(4.80419244001679,6.55528173096446,6.71539371752536));
#73148=CARTESIAN_POINT('Ctrl Pts',(4.9467595481762,6.44587135576158,6.70835375129049));
#73149=CARTESIAN_POINT('',(-8.1252499974825,-0.000202263843970515,7.5832974431918));
#73150=CARTESIAN_POINT('Ctrl Pts',(-8.1252499974825,-0.000202263844008403,
7.5832974431918));
#73151=CARTESIAN_POINT('Ctrl Pts',(-8.1252552002741,0.208801884231222,7.57510884366752));
#73152=CARTESIAN_POINT('Ctrl Pts',(-8.11719180360737,0.417835476072454,
7.56692024414324));
#73153=CARTESIAN_POINT('Ctrl Pts',(-8.10107906878029,0.626263110736931,
7.55873164461896));
#73154=CARTESIAN_POINT('Ctrl Pts',(-8.08496842127045,0.83466374473374,7.55054410588326));
#73155=CARTESIAN_POINT('Ctrl Pts',(-8.06081054017175,1.04245827946469,7.54235656714756));
#73156=CARTESIAN_POINT('Ctrl Pts',(-8.02867667051253,1.24901500506112,7.53416902841186));
#73157=CARTESIAN_POINT('Ctrl Pts',(-7.99654068670408,1.45558532042276,7.5259809510022));
#73158=CARTESIAN_POINT('Ctrl Pts',(-7.95642770943993,1.6609173673095,7.51779287359254));
#73159=CARTESIAN_POINT('Ctrl Pts',(-7.90846052257459,1.86438722517056,7.50960479618288));
#73160=CARTESIAN_POINT('Ctrl Pts',(-7.86049297173956,2.06785862693837,7.501416656643));
#73161=CARTESIAN_POINT('Ctrl Pts',(-7.80467116400753,2.26946752036822,7.49322851710311));
#73162=CARTESIAN_POINT('Ctrl Pts',(-7.74116853449045,2.46860229342738,7.48504037756323));
#73163=CARTESIAN_POINT('Ctrl Pts',(-7.67765237376068,2.66777949835102,7.47685049328523));
#73164=CARTESIAN_POINT('Ctrl Pts',(-7.60645221399996,2.86448124447907,7.46866060900724));
#73165=CARTESIAN_POINT('Ctrl Pts',(-7.52779101068967,3.05811217287395,7.46047072472924));
#73166=CARTESIAN_POINT('Ctrl Pts',(-7.51125416811851,3.09881895137494,7.45874897599821));
#73167=CARTESIAN_POINT('Ctrl Pts',(-7.49438774727284,3.13939007887198,7.45702722726718));
#73168=CARTESIAN_POINT('Ctrl Pts',(-7.47719409066218,3.1798201353326,7.45530547853615));
#73169=CARTESIAN_POINT('Ctrl Pts',(-7.39508629338615,3.37289267102977,7.44708331852857));
#73170=CARTESIAN_POINT('Ctrl Pts',(-7.30548280958889,3.56281514419167,7.438861158521));
#73171=CARTESIAN_POINT('Ctrl Pts',(-7.20865076152545,3.74900543622686,7.43063899851343));
#73172=CARTESIAN_POINT('Ctrl Pts',(-7.11183656244216,3.93516140794255,7.42241835409057));
#73173=CARTESIAN_POINT('Ctrl Pts',(-7.00779659456183,4.11758630986869,7.41419770966771));
#73174=CARTESIAN_POINT('Ctrl Pts',(-6.89684444736205,4.29572161940124,7.40597706524484));
#73175=CARTESIAN_POINT('Ctrl Pts',(-6.78590476488787,4.47383691663291,7.39775734435595));
#73176=CARTESIAN_POINT('Ctrl Pts',(-6.66805460937235,4.6476633331402,7.38953762346704));
#73177=CARTESIAN_POINT('Ctrl Pts',(-6.54365194239556,4.81666968135482,7.38131790257815));
#73178=CARTESIAN_POINT('Ctrl Pts',(-6.41923930750566,4.98568957140608,7.37309752307425));
#73179=CARTESIAN_POINT('Ctrl Pts',(-6.28827328486527,5.14988838215142,7.36487714357034));
#73180=CARTESIAN_POINT('Ctrl Pts',(-6.15115395708075,5.30876563419311,7.35665676406644));
#73181=CARTESIAN_POINT('Ctrl Pts',(-6.01403513673758,5.4676422982733,7.34843641498392));
#73182=CARTESIAN_POINT('Ctrl Pts',(-5.87076325166009,5.62119722135228,7.34021606590141));
#73183=CARTESIAN_POINT('Ctrl Pts',(-5.72177764548016,5.76896421710028,7.33199571681889));
#73184=CARTESIAN_POINT('Ctrl Pts',(-5.57276018418834,5.91676280740499,7.32377361011599));
#73185=CARTESIAN_POINT('Ctrl Pts',(-5.41802677073111,6.05877079014034,7.31555150341308));
#73186=CARTESIAN_POINT('Ctrl Pts',(-5.25805325742347,6.19455918565627,7.30732939671017));
#73187=CARTESIAN_POINT('Ctrl Pts',(-5.18789619200383,6.25410976468943,7.30372355680632));
#73188=CARTESIAN_POINT('Ctrl Pts',(-5.11673174874588,6.31246463534114,7.30011771690248));
#73189=CARTESIAN_POINT('Ctrl Pts',(-5.04460209560563,6.3695900385748,7.29651187699863));
#73190=CARTESIAN_POINT('Ctrl Pts',(-4.88012958289725,6.49984934525757,7.28828971699106));
#73191=CARTESIAN_POINT('Ctrl Pts',(-4.71058199250573,6.62375634551582,7.28006755698349));
#73192=CARTESIAN_POINT('Ctrl Pts',(-4.53647239391172,6.74092766477856,7.27184539697592));
#73193=CARTESIAN_POINT('Ctrl Pts',(-4.36239488881203,6.85807738593814,7.26362475255306));
#73194=CARTESIAN_POINT('Ctrl Pts',(-4.1837572985887,6.96849373943008,7.25540410813019));
#73195=CARTESIAN_POINT('Ctrl Pts',(-4.00110220780467,7.07183630220614,7.24718346370733));
#73196=CARTESIAN_POINT('Ctrl Pts',(-3.8184676370875,7.17516725514264,7.2389637428184));
#73197=CARTESIAN_POINT('Ctrl Pts',(-3.63181672365398,7.27142585863154,7.23074402192947));
#73198=CARTESIAN_POINT('Ctrl Pts',(-3.4417179385002,7.36031692213766,7.22252430104054));
#73199=CARTESIAN_POINT('Ctrl Pts',(-3.25160392145396,7.44921510814652,7.21430392153664));
#73200=CARTESIAN_POINT('Ctrl Pts',(-3.05804174689303,7.53074444713321,7.20608354203274));
#73201=CARTESIAN_POINT('Ctrl Pts',(-2.86162218171216,7.6046568661336,7.19786316252884));
#73202=CARTESIAN_POINT('Ctrl Pts',(-2.66520334342744,7.67856901160394,7.18964281344636));
#73203=CARTESIAN_POINT('Ctrl Pts',(-2.46592741284939,7.74486419202678,7.18142246436389));
#73204=CARTESIAN_POINT('Ctrl Pts',(-2.26440322621074,7.80334323169412,7.17320211528141));
#73205=CARTESIAN_POINT('Ctrl Pts',(-2.0628359510097,7.8618347749611,7.16498000857852));
#73206=CARTESIAN_POINT('Ctrl Pts',(-1.8590197428969,7.91250675647965,7.15675790187563));
#73207=CARTESIAN_POINT('Ctrl Pts',(-1.65357769658261,7.9552101395164,7.14853579517274));
#73208=CARTESIAN_POINT('Ctrl Pts',(-1.56348021240926,7.97393788997609,7.14492995526886));
#73209=CARTESIAN_POINT('Ctrl Pts',(-1.47307018490379,7.99113369875667,7.14132411536497));
#73210=CARTESIAN_POINT('Ctrl Pts',(-1.38240079415703,8.00678809553581,7.13771827546109));
#73211=CARTESIAN_POINT('Ctrl Pts',(-1.1756533349293,8.0424837887921,7.12949611545351));
#73212=CARTESIAN_POINT('Ctrl Pts',(-0.967488444512142,8.07017329074264,
7.12127395544593));
#73213=CARTESIAN_POINT('Ctrl Pts',(-0.758540080192574,8.08976541744205,
7.11305179543835));
#73214=CARTESIAN_POINT('Ctrl Pts',(-0.54963023117222,8.10935393273908,7.10483115101552));
#73215=CARTESIAN_POINT('Ctrl Pts',(-0.339937490192298,8.12084802423565,
7.09661050659268));
#73216=CARTESIAN_POINT('Ctrl Pts',(-0.130101183253439,8.1242083457169,7.08838986216984));
#73217=CARTESIAN_POINT('Ctrl Pts',(0.079711549991263,8.12756828968869,7.08017014128097));
#73218=CARTESIAN_POINT('Ctrl Pts',(0.289667522005959,8.12279628320706,7.07195042039211));
#73219=CARTESIAN_POINT('Ctrl Pts',(0.499126315780342,8.10990508473407,7.06373069950324));
#73220=CARTESIAN_POINT('Ctrl Pts',(0.708601892691915,8.09701285333834,7.05551031999937));
#73221=CARTESIAN_POINT('Ctrl Pts',(0.917579917001217,8.07600014547325,7.0472899404955));
#73222=CARTESIAN_POINT('Ctrl Pts',(1.12542293549719,8.04693176178081,7.03906956099163));
#73223=CARTESIAN_POINT('Ctrl Pts',(1.33326518482319,8.01786348566248,7.03084921190914));
#73224=CARTESIAN_POINT('Ctrl Pts',(1.53997214480885,7.98073963687538,7.02262886282664));
#73225=CARTESIAN_POINT('Ctrl Pts',(1.7449138889492,7.93567659892036,7.01440851374414));
#73226=CARTESIAN_POINT('Ctrl Pts',(1.94989945237117,7.89060392588606,7.00618640704123));
#73227=CARTESIAN_POINT('Ctrl Pts',(2.15311875760632,7.83758873579499,6.99796430033833));
#73228=CARTESIAN_POINT('Ctrl Pts',(2.35395334534642,7.77679826216627,6.98974219363543));
#73229=CARTESIAN_POINT('Ctrl Pts',(2.44203020894514,7.7501383411131,6.98613635373148));
#73230=CARTESIAN_POINT('Ctrl Pts',(2.52964859970418,7.72198365208525,6.98253051382753));
#73231=CARTESIAN_POINT('Ctrl Pts',(2.61675728791372,7.69235132184239,6.97892467392359));
#73232=CARTESIAN_POINT('Ctrl Pts',(2.81538378825199,7.62478325057437,6.97070258522472));
#73233=CARTESIAN_POINT('Ctrl Pts',(3.01142462280939,7.5495067262633,6.96248049652585));
#73234=CARTESIAN_POINT('Ctrl Pts',(3.20427948755665,7.46674497543097,6.95425840782698));
#73235=CARTESIAN_POINT('Ctrl Pts',(3.39710413541919,7.38399619187477,6.94603760738136));
#73236=CARTESIAN_POINT('Ctrl Pts',(3.58674353824727,7.29376463787685,6.93781680693574));
#73237=CARTESIAN_POINT('Ctrl Pts',(3.7726174297204,7.19632165008415,6.92959600649013));
#73238=CARTESIAN_POINT('Ctrl Pts',(3.95846688806202,7.09889147117664,6.9213762866691));
#73239=CARTESIAN_POINT('Ctrl Pts',(4.14055156224465,6.99425188856954,6.91315656684808));
#73240=CARTESIAN_POINT('Ctrl Pts',(4.31831518978921,6.88272050021906,6.90493684702706));
#73241=CARTESIAN_POINT('Ctrl Pts',(4.4960786909369,6.77118919117176,6.89671713305057));
#73242=CARTESIAN_POINT('Ctrl Pts',(4.66952090125097,6.65276624237792,6.88849741907409));
#73243=CARTESIAN_POINT('Ctrl Pts',(4.8381131863584,6.52781344390945,6.88027770509761));
#73244=CARTESIAN_POINT('Ctrl Pts',(4.87455687045246,6.50080307204604,6.87850089390301));
#73245=CARTESIAN_POINT('Ctrl Pts',(4.9107740419292,6.47348773790737,6.8767240827084));
#73246=CARTESIAN_POINT('Ctrl Pts',(4.94675954817621,6.44587135576157,6.8749472715138));
#73247=CARTESIAN_POINT('Ctrl Pts',(4.9467595481762,6.44587135576158,8.87494054454767));
#73248=CARTESIAN_POINT('Ctrl Pts',(5.11320844408724,6.31813336353569,8.86671903882184));
#73249=CARTESIAN_POINT('Ctrl Pts',(5.27473107141465,6.18392618048737,8.85849753309601));
#73250=CARTESIAN_POINT('Ctrl Pts',(5.43083107949353,6.0436546351117,8.85027602737019));
#73251=CARTESIAN_POINT('Ctrl Pts',(5.58690664532328,5.90340505355332,8.84205580897351));
#73252=CARTESIAN_POINT('Ctrl Pts',(5.73756106725395,5.75709320220086,8.83383559057684));
#73253=CARTESIAN_POINT('Ctrl Pts',(5.88233252242706,5.60516294661421,8.82561537218016));
#73254=CARTESIAN_POINT('Ctrl Pts',(6.02903899773482,5.45120198612603,8.81728528206817));
#73255=CARTESIAN_POINT('Ctrl Pts',(6.16970388967293,5.29147156466319,8.80895519195618));
#73256=CARTESIAN_POINT('Ctrl Pts',(6.30388591896933,5.12647148466859,8.80062510184419));
#73257=CARTESIAN_POINT('Ctrl Pts',(6.43629937652069,4.96364617040781,8.79240480558524));
#73258=CARTESIAN_POINT('Ctrl Pts',(6.56239963966013,4.7956895020486,8.7841845093263));
#73259=CARTESIAN_POINT('Ctrl Pts',(6.6818033980155,4.62311484961909,8.77596421306735));
#73260=CARTESIAN_POINT('Ctrl Pts',(6.80359936918501,4.44708272398585,8.76757922602884));
#73261=CARTESIAN_POINT('Ctrl Pts',(6.91842749572302,4.26624588128782,8.75919423899032));
#73262=CARTESIAN_POINT('Ctrl Pts',(7.02592720131281,4.08118053072303,8.75080925195181));
#73263=CARTESIAN_POINT('Ctrl Pts',(7.13342690690261,3.89611518015824,8.74242426491329));
#73264=CARTESIAN_POINT('Ctrl Pts',(7.23359803514733,3.70682160736471,8.73403927787478));
#73265=CARTESIAN_POINT('Ctrl Pts',(7.32612922650988,3.51390354434748,8.72565429083627));
#73266=CARTESIAN_POINT('Ctrl Pts',(7.41686356605974,3.32473173344402,8.7174321308287));
#73267=CARTESIAN_POINT('Ctrl Pts',(7.50028190538392,3.13201247964481,8.70920997082113));
#73268=CARTESIAN_POINT('Ctrl Pts',(7.57612360073261,2.93633083097296,8.70098781081357));
#73269=CARTESIAN_POINT('Ctrl Pts',(7.65195131623721,2.74068525215593,8.69276716639072));
#73270=CARTESIAN_POINT('Ctrl Pts',(7.72020506857548,2.54207864337667,8.68454652196788));
#73271=CARTESIAN_POINT('Ctrl Pts',(7.78067262180944,2.34111535698798,8.67632587754504));
#73272=CARTESIAN_POINT('Ctrl Pts',(7.84113338192164,2.14017464746909,8.66810615665615));
#73273=CARTESIAN_POINT('Ctrl Pts',(7.89380960425461,1.93687807142458,8.65988643576727));
#73274=CARTESIAN_POINT('Ctrl Pts',(7.93853888428697,1.73184524284469,8.65166671487838));
#73275=CARTESIAN_POINT('Ctrl Pts',(7.98327174830661,1.5267959857632,8.64344633537448));
#73276=CARTESIAN_POINT('Ctrl Pts',(8.02005633214138,1.32001048596106,8.63522595587059));
#73277=CARTESIAN_POINT('Ctrl Pts',(8.04878110854307,1.11211970095856,8.6270055763667));
#73278=CARTESIAN_POINT('Ctrl Pts',(8.07750577864218,0.904229685303227,8.61878522728419));
#73279=CARTESIAN_POINT('Ctrl Pts',(8.0981706632209,0.695234685361304,8.61056487820168));
#73280=CARTESIAN_POINT('Ctrl Pts',(8.11071591497123,0.485772487006474,8.60234452911917));
#73281=CARTESIAN_POINT('Ctrl Pts',(8.12326384906389,0.276265502836732,8.59412242241627));
#73282=CARTESIAN_POINT('Ctrl Pts',(8.12768866431693,0.0662914153624913,
8.58590031571336));
#73283=CARTESIAN_POINT('Ctrl Pts',(8.123982563112,-0.143509152154886,8.57767820901045));
#73284=CARTESIAN_POINT('Ctrl Pts',(8.12235723664817,-0.235518084360483,
8.57407236910655));
#73285=CARTESIAN_POINT('Ctrl Pts',(8.11916876765902,-0.327493638605861,
8.57046652920265));
#73286=CARTESIAN_POINT('Ctrl Pts',(8.11441966015929,-0.419381856212609,
8.56686068929876));
#73287=CARTESIAN_POINT('Ctrl Pts',(8.10359058210908,-0.62890852631129,8.55863852929119));
#73288=CARTESIAN_POINT('Ctrl Pts',(8.08463993274142,-0.838050112345938,
8.55041636928362));
#73289=CARTESIAN_POINT('Ctrl Pts',(8.05761873788753,-1.04616816876821,8.54219420927605));
#73290=CARTESIAN_POINT('Ctrl Pts',(8.03060252383067,-1.25424786294171,8.53397356485321));
#73291=CARTESIAN_POINT('Ctrl Pts',(7.99551877138917,-1.46130411151605,8.52575292043037));
#73292=CARTESIAN_POINT('Ctrl Pts',(7.95247025031508,-1.66670467700599,8.51753227600752));
#73293=CARTESIAN_POINT('Ctrl Pts',(7.90942656545197,-1.87208216712783,8.50931255511864));
#73294=CARTESIAN_POINT('Ctrl Pts',(7.85841995885542,-2.0758040567574,8.50109283422974));
#73295=CARTESIAN_POINT('Ctrl Pts',(7.79960426016178,-2.27724854756045,8.49287311334086));
#73296=CARTESIAN_POINT('Ctrl Pts',(7.74078384878968,-2.47870917934514,8.48465273383696));
#73297=CARTESIAN_POINT('Ctrl Pts',(7.67415317518488,-2.67789176360212,8.47643235433307));
#73298=CARTESIAN_POINT('Ctrl Pts',(7.59991617272585,-2.87418888210919,8.46821197482918));
#73299=CARTESIAN_POINT('Ctrl Pts',(7.52567944499771,-3.07048527417417,8.45999162574667));
#73300=CARTESIAN_POINT('Ctrl Pts',(7.44383655162332,-3.26389594673264,8.45177127666416));
#73301=CARTESIAN_POINT('Ctrl Pts',(7.35464007437481,-3.45383221058871,8.44355092758165));
#73302=CARTESIAN_POINT('Ctrl Pts',(7.26542452572847,-3.64380908535411,8.43532882087874));
#73303=CARTESIAN_POINT('Ctrl Pts',(7.16885237755272,-3.83030980009103,8.42710671417583));
#73304=CARTESIAN_POINT('Ctrl Pts',(7.06522327530623,-4.01276807610048,8.41888460747293));
#73305=CARTESIAN_POINT('Ctrl Pts',(7.01977629126834,-4.0927859299429,8.41527876756903));
#73306=CARTESIAN_POINT('Ctrl Pts',(6.97297263975525,-4.17202662099389,8.41167292766515));
#73307=CARTESIAN_POINT('Ctrl Pts',(6.92484033500501,-4.25044396471565,8.40806708776126));
#73308=CARTESIAN_POINT('Ctrl Pts',(6.81508740039395,-4.42925388546487,8.39984492775369));
#73309=CARTESIAN_POINT('Ctrl Pts',(6.69838693633129,-4.60384005848017,8.39162276774611));
#73310=CARTESIAN_POINT('Ctrl Pts',(6.57508920080886,-4.77366626021412,8.38340060773854));
#73311=CARTESIAN_POINT('Ctrl Pts',(6.45181419266758,-4.94346115800889,8.37517996331569));
#73312=CARTESIAN_POINT('Ctrl Pts',(6.32194451348697,-5.10849759698116,8.36695931889285));
#73313=CARTESIAN_POINT('Ctrl Pts',(6.18587288883578,-5.26826956083935,8.35873867447));
#73314=CARTESIAN_POINT('Ctrl Pts',(6.04981655091383,-5.42802357539506,8.3505189535811));
#73315=CARTESIAN_POINT('Ctrl Pts',(5.90755984981741,-5.58251407097313,8.34229923269221));
#73316=CARTESIAN_POINT('Ctrl Pts',(5.75953535374654,-5.73126862670419,8.33407951180331));
#73317=CARTESIAN_POINT('Ctrl Pts',(5.61149899703531,-5.8800351015725,8.32585913229942));
#73318=CARTESIAN_POINT('Ctrl Pts',(5.45769412818033,-6.02306450712544,8.31763875279552));
#73319=CARTESIAN_POINT('Ctrl Pts',(5.29859043292924,-6.15992102113093,8.30941837329163));
#73320=CARTESIAN_POINT('Ctrl Pts',(5.13948732647769,-6.29677702866765,8.30119802420912));
#73321=CARTESIAN_POINT('Ctrl Pts',(4.97508565835178,-6.42745999991004,8.29297767512662));
#73322=CARTESIAN_POINT('Ctrl Pts',(4.80588887322038,-6.55157383387813,8.28475732604412));
#73323=CARTESIAN_POINT('Ctrl Pts',(4.63665591155685,-6.67571420504135,8.2765352193412));
#73324=CARTESIAN_POINT('Ctrl Pts',(4.462626022647,-6.79328245826792,8.2683131126383));
#73325=CARTESIAN_POINT('Ctrl Pts',(4.28433325718575,-6.90392468845599,8.26009100593539));
#73326=CARTESIAN_POINT('Ctrl Pts',(4.20614220573086,-6.95244730961417,8.2564851660315));
#73327=CARTESIAN_POINT('Ctrl Pts',(4.12713164619852,-6.99963841466141,8.2528793261276));
#73328=CARTESIAN_POINT('Ctrl Pts',(4.04734827464875,-7.0454708505676,8.24927348622371));
#73329=CARTESIAN_POINT('Ctrl Pts',(3.8654234903237,-7.14997954524122,8.24105132621614));
#73330=CARTESIAN_POINT('Ctrl Pts',(3.67941866156424,-7.24745535659331,8.23282916620857));
#73331=CARTESIAN_POINT('Ctrl Pts',(3.48989790400209,-7.33759498624323,8.224607006201));
#73332=CARTESIAN_POINT('Ctrl Pts',(3.30041208066243,-7.4277180005212,8.21638636177816));
#73333=CARTESIAN_POINT('Ctrl Pts',(3.10741188841331,-7.51050740534339,8.20816571735532));
#73334=CARTESIAN_POINT('Ctrl Pts',(2.91148428275235,-7.58570674583364,8.19994507293248));
#73335=CARTESIAN_POINT('Ctrl Pts',(2.71557868823589,-7.66089763818539,8.19172535204357));
#73336=CARTESIAN_POINT('Ctrl Pts',(2.5167466123199,-7.72850006283006,8.18350563115468));
#73337=CARTESIAN_POINT('Ctrl Pts',(2.31559392433724,-7.78830612778366,8.17528591026577));
#73338=CARTESIAN_POINT('Ctrl Pts',(2.11442511875439,-7.84811698476988,8.16706553076188));
#73339=CARTESIAN_POINT('Ctrl Pts',(1.91093561171014,-7.90013014713468,8.15884515125798));
#73340=CARTESIAN_POINT('Ctrl Pts',(1.70574635657988,-7.9441876192292,8.15062477175409));
#73341=CARTESIAN_POINT('Ctrl Pts',(1.50055786079896,-7.98824492827905,8.14240442267157));
#73342=CARTESIAN_POINT('Ctrl Pts',(1.29366991864227,-8.02434654660311,8.13418407358906));
#73343=CARTESIAN_POINT('Ctrl Pts',(1.08571412428032,-8.05238551007329,8.12596372450655));
#73344=CARTESIAN_POINT('Ctrl Pts',(0.877713866193068,-8.0804304686482,8.11774161780365));
#73345=CARTESIAN_POINT('Ctrl Pts',(0.668645592315945,-8.10040928889974,
8.10951951110075));
#73346=CARTESIAN_POINT('Ctrl Pts',(0.459147585041741,-8.11226670281804,
8.10129740439785));
#73347=CARTESIAN_POINT('Ctrl Pts',(0.367271341919506,-8.1174668221802,8.09769156449397));
#73348=CARTESIAN_POINT('Ctrl Pts',(0.275312503188222,-8.12110562587664,
8.09408572459009));
#73349=CARTESIAN_POINT('Ctrl Pts',(0.183325064680515,-8.12318161086898,
8.09047988468621));
#73350=CARTESIAN_POINT('Ctrl Pts',(-0.0264278523258185,-8.12791534315752,
8.08225772467864));
#73351=CARTESIAN_POINT('Ctrl Pts',(-0.23639882799153,-8.12452130448339,
8.07403556467107));
#73352=CARTESIAN_POINT('Ctrl Pts',(-0.445947390837542,-8.11300304986416,
8.0658134046635));
#73353=CARTESIAN_POINT('Ctrl Pts',(-0.655457327750723,-8.10148691839635,
8.05759276024066));
#73354=CARTESIAN_POINT('Ctrl Pts',(-0.864544712698323,-8.08184957603862,
8.04937211581781));
#73355=CARTESIAN_POINT('Ctrl Pts',(-1.07257142920726,-8.0541466395732,8.04115147139497));
#73356=CARTESIAN_POINT('Ctrl Pts',(-1.28057477531725,-8.0264468153459,8.03293175050609));
#73357=CARTESIAN_POINT('Ctrl Pts',(-1.48751739843576,-7.99068324495086,
8.02471202961722));
#73358=CARTESIAN_POINT('Ctrl Pts',(-1.69276780725117,-7.94696323844738,
8.01649230872834));
#73359=CARTESIAN_POINT('Ctrl Pts',(-1.89803466200229,-7.90323972882582,
8.00827192922445));
#73360=CARTESIAN_POINT('Ctrl Pts',(-2.10160874228074,-7.85155856808936,
8.00005154972057));
#73361=CARTESIAN_POINT('Ctrl Pts',(-2.30286918293556,-7.79207809822166,
7.99183117021667));
#73362=CARTESIAN_POINT('Ctrl Pts',(-2.50412887878015,-7.73259784847503,
7.98361082113418));
#73363=CARTESIAN_POINT('Ctrl Pts',(-2.70307466984352,-7.66531843354412,
7.97539047205168));
#73364=CARTESIAN_POINT('Ctrl Pts',(-2.89910076197325,-7.59044809839486,
7.96717012296918));
#73365=CARTESIAN_POINT('Ctrl Pts',(-3.0951687670989,-7.51556175496824,7.95894801626629));
#73366=CARTESIAN_POINT('Ctrl Pts',(-3.28831555034599,-7.43308135413365,
7.95072590956339));
#73367=CARTESIAN_POINT('Ctrl Pts',(-3.47795417738127,-7.34326373641422,
7.9425038028605));
#73368=CARTESIAN_POINT('Ctrl Pts',(-3.56112100474076,-7.30387383772379,
7.93889796295656));
#73369=CARTESIAN_POINT('Ctrl Pts',(-3.64361338276509,-7.26307339065166,
7.93529212305263));
#73370=CARTESIAN_POINT('Ctrl Pts',(-3.72538317719994,-7.22088690851309,
7.9316862831487));
#73371=CARTESIAN_POINT('Ctrl Pts',(-3.9118374712177,-7.12469184285827,7.92346412314114));
#73372=CARTESIAN_POINT('Ctrl Pts',(-4.09459468685995,-7.02125524270543,
7.91524196313357));
#73373=CARTESIAN_POINT('Ctrl Pts',(-4.27309411014204,-6.91088664994365,
7.90701980312601));
#73374=CARTESIAN_POINT('Ctrl Pts',(-4.4515606307568,-6.80053840134335,7.89879915870315));
#73375=CARTESIAN_POINT('Ctrl Pts',(-4.6257706745293,-6.68326086552329,7.89057851428029));
#73376=CARTESIAN_POINT('Ctrl Pts',(-4.79519050332591,-6.5594081744707,7.88235786985743));
#73377=CARTESIAN_POINT('Ctrl Pts',(-4.96459129894741,-6.43556939743261,
7.87413814896852));
#73378=CARTESIAN_POINT('Ctrl Pts',(-5.12920271579681,-6.30515711398618,
7.86591842807962));
#73379=CARTESIAN_POINT('Ctrl Pts',(-5.28852156503186,-6.16856767967192,
7.85769870719072));
#73380=CARTESIAN_POINT('Ctrl Pts',(-5.44785317988055,-6.03196730096561,
7.84947832768683));
#73381=CARTESIAN_POINT('Ctrl Pts',(-5.60189115392101,-5.88918897246384,
7.84125794818294));
#73382=CARTESIAN_POINT('Ctrl Pts',(-5.7501660445744,-5.74066877831525,7.83303756867906));
#73383=CARTESIAN_POINT('Ctrl Pts',(-5.89844038650325,-5.59214913379901,
7.82481721959653));
#73384=CARTESIAN_POINT('Ctrl Pts',(-6.04095148107157,-5.43788787689858,
7.81659687051401));
#73385=CARTESIAN_POINT('Ctrl Pts',(-6.17726699497406,-5.27835770247755,
7.80837652143148));
#73386=CARTESIAN_POINT('Ctrl Pts',(-6.3136116549533,-5.11879341837543,7.80015441472858));
#73387=CARTESIAN_POINT('Ctrl Pts',(-6.44375789600635,-4.95395819052529,
7.79193230802567));
#73388=CARTESIAN_POINT('Ctrl Pts',(-6.56731319565416,-4.78435836373977,
7.78371020132277));
#73389=CARTESIAN_POINT('Ctrl Pts',(-6.62149889840672,-4.70997963755579,
7.78010436141891));
#73390=CARTESIAN_POINT('Ctrl Pts',(-6.6744175022403,-4.6346849479598,7.77649852151505));
#73391=CARTESIAN_POINT('Ctrl Pts',(-6.72603846708451,-4.55851884956062,
7.77289268161119));
#73392=CARTESIAN_POINT('Ctrl Pts',(-6.84374636427645,-4.38484229572363,
7.76467052160362));
#73393=CARTESIAN_POINT('Ctrl Pts',(-6.95474319978445,-4.20657555000885,
7.75644836159605));
#73394=CARTESIAN_POINT('Ctrl Pts',(-7.05868468976772,-4.02425869110558,
7.74822620158848));
#73395=CARTESIAN_POINT('Ctrl Pts',(-7.16260702029215,-3.84197543853559,
7.74000555716566));
#73396=CARTESIAN_POINT('Ctrl Pts',(-7.25947645481937,-3.65564381906843,
7.73178491274283));
#73397=CARTESIAN_POINT('Ctrl Pts',(-7.34899373090753,-3.46583016109876,
7.72356426832001));
#73398=CARTESIAN_POINT('Ctrl Pts',(-7.4385009503334,-3.2760378274135,7.71534454743114));
#73399=CARTESIAN_POINT('Ctrl Pts',(-7.52065753445803,-3.08276450303734,
7.70712482654229));
#73400=CARTESIAN_POINT('Ctrl Pts',(-7.59521124794654,-2.88659897830758,
7.69890510565342));
#73401=CARTESIAN_POINT('Ctrl Pts',(-7.66977093514102,-2.69041773557919,
7.69068472614954));
#73402=CARTESIAN_POINT('Ctrl Pts',(-7.73672642706943,-2.49134410438495,
7.68246434664565));
#73403=CARTESIAN_POINT('Ctrl Pts',(-7.79587412919473,-2.28998561660382,
7.67424396714176));
#73404=CARTESIAN_POINT('Ctrl Pts',(-7.85502161243047,-2.08862787399564,
7.66602361805926));
#73405=CARTESIAN_POINT('Ctrl Pts',(-7.90636128304193,-1.88498557564683,
7.65780326897677));
#73406=CARTESIAN_POINT('Ctrl Pts',(-7.94973964874673,-1.67968064811268,
7.64958291989427));
#73407=CARTESIAN_POINT('Ctrl Pts',(-7.99312728932537,-1.47433182364348,
7.64136081319136));
#73408=CARTESIAN_POINT('Ctrl Pts',(-8.02855016324043,-1.26731994861156,
7.63313870648846));
#73409=CARTESIAN_POINT('Ctrl Pts',(-8.05590583625226,-1.05927745182114,
7.62491659978555));
#73410=CARTESIAN_POINT('Ctrl Pts',(-8.06790278313099,-0.968039529016909,
7.62131075988159));
#73411=CARTESIAN_POINT('Ctrl Pts',(-8.07834883374,-0.876603491590593,7.61770491997762));
#73412=CARTESIAN_POINT('Ctrl Pts',(-8.08723848625962,-0.785023075368658,
7.61409908007365));
#73413=CARTESIAN_POINT('Ctrl Pts',(-8.10880793006934,-0.56281656758756,
7.60535003605603));
#73414=CARTESIAN_POINT('Ctrl Pts',(-8.12121555449676,-0.339714641363502,
7.59660099203841));
#73415=CARTESIAN_POINT('Ctrl Pts',(-8.12441558747629,-0.116442794849301,
7.58785194802079));
#73416=CARTESIAN_POINT('Ctrl Pts',(-8.12497086969009,-0.0776997925098787,
7.58633377975132));
#73417=CARTESIAN_POINT('Ctrl Pts',(-8.1252490328812,-0.0389516823687162,
7.58481561148186));
#73418=CARTESIAN_POINT('Ctrl Pts',(-8.12524999748248,-0.000202264369551694,
7.58329744321239));
#73419=CARTESIAN_POINT('Origin',(0.,0.,24.4167025567876));
#73420=CARTESIAN_POINT('',(4.94675954817619,6.44587135576159,10.8749423500932));
#73421=CARTESIAN_POINT('',(4.9467595481762,6.44587135576158,10.7083502273763));
#73422=CARTESIAN_POINT('',(4.9467595481762,6.44587135576158,24.4167025567876));
#73423=CARTESIAN_POINT('',(-8.12524999762442,0.000196479806862634,9.41670255674903));
#73424=CARTESIAN_POINT('Ctrl Pts',(4.9467595481762,6.44587135576158,10.7083502273763));
#73425=CARTESIAN_POINT('Ctrl Pts',(5.11325096527104,6.31810073147397,10.7001299359995));
#73426=CARTESIAN_POINT('Ctrl Pts',(5.27478576238475,6.18387897582806,10.6919096446227));
#73427=CARTESIAN_POINT('Ctrl Pts',(5.43087265766335,6.04361727268899,10.6836893532459));
#73428=CARTESIAN_POINT('Ctrl Pts',(5.5869968406379,5.90332206234399,10.6754670981186));
#73429=CARTESIAN_POINT('Ctrl Pts',(5.73767030074121,5.75698421778979,10.6672448429912));
#73430=CARTESIAN_POINT('Ctrl Pts',(5.88243667227605,5.60505364462838,10.6590225878639));
#73431=CARTESIAN_POINT('Ctrl Pts',(5.99894154973237,5.48278317103445,10.6524054929138));
#73432=CARTESIAN_POINT('Ctrl Pts',(6.11162122338302,5.35689124117962,10.6457883979637));
#73433=CARTESIAN_POINT('Ctrl Pts',(6.22025579367875,5.2276290441945,10.6391713030136));
#73434=CARTESIAN_POINT('Ctrl Pts',(6.35524113483892,5.06701256905541,10.630949143006));
#73435=CARTESIAN_POINT('Ctrl Pts',(6.4840243824159,4.90113850458407,10.6227269829984));
#73436=CARTESIAN_POINT('Ctrl Pts',(6.60620740934068,4.73050855905286,10.6145048229909));
#73437=CARTESIAN_POINT('Ctrl Pts',(6.72836791435707,4.55991006561525,10.606284178568));
#73438=CARTESIAN_POINT('Ctrl Pts',(6.84393045516928,4.38455768063056,10.5980635341452));
#73439=CARTESIAN_POINT('Ctrl Pts',(6.95253898010046,4.20498386354617,10.5898428897224));
#73440=CARTESIAN_POINT('Ctrl Pts',(7.06113530359661,4.02543022036859,10.5816231688335));
#73441=CARTESIAN_POINT('Ctrl Pts',(7.16277901821338,3.84165634434287,10.5734034479446));
#73442=CARTESIAN_POINT('Ctrl Pts',(7.25715853317428,3.65422188528224,10.5651837270558));
#73443=CARTESIAN_POINT('Ctrl Pts',(7.35154561040727,3.46677240781028,10.5569633475519));
#73444=CARTESIAN_POINT('Ctrl Pts',(7.43866718980509,3.27566202363514,10.548742968048));
#73445=CARTESIAN_POINT('Ctrl Pts',(7.51825813012694,3.08147403871591,10.5405225885441));
#73446=CARTESIAN_POINT('Ctrl Pts',(7.59784877590435,2.88728677243362,10.5323022394616));
#73447=CARTESIAN_POINT('Ctrl Pts',(7.66990872889148,2.69002220229786,10.5240818903791));
#73448=CARTESIAN_POINT('Ctrl Pts',(7.73422119917883,2.49028311737297,10.5158615412966));
#73449=CARTESIAN_POINT('Ctrl Pts',(7.79854742033114,2.29050132556445,10.5076394345937));
#73450=CARTESIAN_POINT('Ctrl Pts',(7.85512275891198,2.08824424295622,10.4994173278907));
#73451=CARTESIAN_POINT('Ctrl Pts',(7.90378012831557,1.88413036856366,10.4911952211878));
#73452=CARTESIAN_POINT('Ctrl Pts',(7.92511902484832,1.79461535984148,10.4875893812839));
#73453=CARTESIAN_POINT('Ctrl Pts',(7.94493571247724,1.70474340757218,10.48398354138));
#73454=CARTESIAN_POINT('Ctrl Pts',(7.96321917898028,1.61456739407823,10.4803777014761));
#73455=CARTESIAN_POINT('Ctrl Pts',(8.00490976732789,1.40894495061114,10.4721555414685));
#73456=CARTESIAN_POINT('Ctrl Pts',(8.03863875133913,1.20167294150668,10.463933381461));
#73457=CARTESIAN_POINT('Ctrl Pts',(8.06429655698148,0.993382405499821,10.4557112214534));
#73458=CARTESIAN_POINT('Ctrl Pts',(8.08994963313922,0.785130263535682,10.4474905770306));
#73459=CARTESIAN_POINT('Ctrl Pts',(8.10753446421489,0.575860262162351,10.4392699326078));
#73460=CARTESIAN_POINT('Ctrl Pts',(8.11699313593587,0.36621031344013,10.4310492881849));
#73461=CARTESIAN_POINT('Ctrl Pts',(8.12645074503888,0.156583917475535,10.4228295672961));
#73462=CARTESIAN_POINT('Ctrl Pts',(8.127784004069,-0.0534220458940956,10.4146098464072));
#73463=CARTESIAN_POINT('Ctrl Pts',(8.1209870496964,-0.263167059419303,10.4063901255184));
#73464=CARTESIAN_POINT('Ctrl Pts',(8.11418955070965,-0.472928879016114,
10.3981697460145));
#73465=CARTESIAN_POINT('Ctrl Pts',(8.09926054350255,-0.682429411903492,
10.3899493665106));
#73466=CARTESIAN_POINT('Ctrl Pts',(8.07624627108753,-0.891029590555041,
10.3817289870067));
#73467=CARTESIAN_POINT('Ctrl Pts',(8.05323208384199,-1.0996289972349,10.3735086379242));
#73468=CARTESIAN_POINT('Ctrl Pts',(8.02213272626158,-1.30732776327298,10.3652882888416));
#73469=CARTESIAN_POINT('Ctrl Pts',(7.98304622121398,-1.51349284519658,10.3570679397591));
#73470=CARTESIAN_POINT('Ctrl Pts',(7.94395135894986,-1.7197020079666,10.3488458330562));
#73471=CARTESIAN_POINT('Ctrl Pts',(7.89686599243614,-1.92437654146016,10.3406237263533));
#73472=CARTESIAN_POINT('Ctrl Pts',(7.84193930641168,-2.12689338638669,10.3324016196504));
#73473=CARTESIAN_POINT('Ctrl Pts',(7.81785097438013,-2.21570801103744,10.3287957797465));
#73474=CARTESIAN_POINT('Ctrl Pts',(7.7922551786284,-2.30410780828417,10.3251899398425));
#73475=CARTESIAN_POINT('Ctrl Pts',(7.76516754947252,-2.39204107220568,10.3215840999386));
#73476=CARTESIAN_POINT('Ctrl Pts',(7.70340140702625,-2.59254952105839,10.313361939931));
#73477=CARTESIAN_POINT('Ctrl Pts',(7.63385477089133,-2.79069743430204,10.3051397799235));
#73478=CARTESIAN_POINT('Ctrl Pts',(7.55673332847167,-2.98587825687275,10.2969176199159));
#73479=CARTESIAN_POINT('Ctrl Pts',(7.47962610179115,-3.18102310190504,10.2886969754931));
#73480=CARTESIAN_POINT('Ctrl Pts',(7.39494696397008,-3.37320167349059,10.2804763310703));
#73481=CARTESIAN_POINT('Ctrl Pts',(7.30295025460098,-3.56182609644596,10.2722556866475));
#73482=CARTESIAN_POINT('Ctrl Pts',(7.2109638804418,-3.75042932871941,10.2640359657586));
#73483=CARTESIAN_POINT('Ctrl Pts',(7.11166170528859,-3.9354789443369,10.2558162448697));
#73484=CARTESIAN_POINT('Ctrl Pts',(7.00534502243036,-4.11640968311102,10.2475965239809));
#73485=CARTESIAN_POINT('Ctrl Pts',(6.89901982081973,-4.29735491917872,10.239376144477));
#73486=CARTESIAN_POINT('Ctrl Pts',(6.78567913565673,-4.47418036311471,10.2311557649731));
#73487=CARTESIAN_POINT('Ctrl Pts',(6.66566932258686,-4.64634695695708,10.2229353854692));
#73488=CARTESIAN_POINT('Ctrl Pts',(6.54565995364141,-4.81851291365667,10.2147150363867));
#73489=CARTESIAN_POINT('Ctrl Pts',(6.41898167712468,-4.98601981415219,10.2064946873043));
#73490=CARTESIAN_POINT('Ctrl Pts',(6.28602343584947,-5.14835866334613,10.1982743382218));
#73491=CARTESIAN_POINT('Ctrl Pts',(6.15303676632627,-5.31073222275451,10.1900522315189));
#73492=CARTESIAN_POINT('Ctrl Pts',(6.01376763655867,-5.4679352949076,10.181830124816));
#73493=CARTESIAN_POINT('Ctrl Pts',(5.86864513921844,-5.61949212940349,10.1736080181131));
#73494=CARTESIAN_POINT('Ctrl Pts',(5.80500105008321,-5.68595802449553,10.1700021782091));
#73495=CARTESIAN_POINT('Ctrl Pts',(5.7402316829715,-5.75133843438792,10.1663963383051));
#73496=CARTESIAN_POINT('Ctrl Pts',(5.6743755008865,-5.81559543275142,10.1627904984011));
#73497=CARTESIAN_POINT('Ctrl Pts',(5.52420797237592,-5.9621164476092,10.1545683383935));
#73498=CARTESIAN_POINT('Ctrl Pts',(5.36833753695209,-6.10284220033841,10.146346178386));
#73499=CARTESIAN_POINT('Ctrl Pts',(5.20723500765842,-6.23733846584555,10.1381240183784));
#73500=CARTESIAN_POINT('Ctrl Pts',(5.04616217427546,-6.37180993975503,10.1299033739556));
#73501=CARTESIAN_POINT('Ctrl Pts',(4.87985939833995,-6.50005402919111,10.1216827295327));
#73502=CARTESIAN_POINT('Ctrl Pts',(4.70883127866183,-6.62167618897179,10.1134620851099));
#73503=CARTESIAN_POINT('Ctrl Pts',(4.5378223728397,-6.74328468532293,10.105242364221));
#73504=CARTESIAN_POINT('Ctrl Pts',(4.36208942353297,-6.85827256624359,10.0970226433321));
#73505=CARTESIAN_POINT('Ctrl Pts',(4.18216744115413,-6.96628760938352,10.0888029224432));
#73506=CARTESIAN_POINT('Ctrl Pts',(4.00223104231048,-7.07431130735843,10.0805825429393));
#73507=CARTESIAN_POINT('Ctrl Pts',(3.81810519137809,-7.1753608969403,10.0723621634355));
#73508=CARTESIAN_POINT('Ctrl Pts',(3.63035193330211,-7.26912872377905,10.0641417839316));
#73509=CARTESIAN_POINT('Ctrl Pts',(3.44259937005134,-7.36289620360784,10.0559214348491));
#73510=CARTESIAN_POINT('Ctrl Pts',(3.25121969174863,-7.4493818451175,10.0477010857667));
#73511=CARTESIAN_POINT('Ctrl Pts',(3.0567979573016,-7.52832476788407,10.0394807366843));
#73512=CARTESIAN_POINT('Ctrl Pts',(2.86233465288943,-7.60728456970255,10.0312586299813));
#73513=CARTESIAN_POINT('Ctrl Pts',(2.66482826641217,-7.67869831979012,10.0230365232784));
#73514=CARTESIAN_POINT('Ctrl Pts',(2.46488320819504,-7.74235353961947,10.0148144165755));
#73515=CARTESIAN_POINT('Ctrl Pts',(2.377196451556,-7.77026980731696,10.0112085766715));
#73516=CARTESIAN_POINT('Ctrl Pts',(2.28904088641286,-7.79669451635676,10.0076027367676));
#73517=CARTESIAN_POINT('Ctrl Pts',(2.20046843319389,-7.82161276445064,10.0039968968636));
#73518=CARTESIAN_POINT('Ctrl Pts',(1.99850248295017,-7.87843220968209,9.99577473685601));
#73519=CARTESIAN_POINT('Ctrl Pts',(1.79430128204897,-7.92743424710151,9.98755257684843));
#73520=CARTESIAN_POINT('Ctrl Pts',(1.58848600965627,-7.96846282288035,9.97933041684084));
#73521=CARTESIAN_POINT('Ctrl Pts',(1.38270867504208,-8.00948383589185,9.97110977241799));
#73522=CARTESIAN_POINT('Ctrl Pts',(1.1753181520486,-8.04253426299419,9.96288912799513));
#73523=CARTESIAN_POINT('Ctrl Pts',(0.966946303989035,-8.06750905842082,
9.95466848357228));
#73524=CARTESIAN_POINT('Ctrl Pts',(0.758597865100385,-8.09248104809773,
9.94644876268335));
#73525=CARTESIAN_POINT('Ctrl Pts',(0.549268614172991,-8.10937918223538,
9.93822904179442));
#73526=CARTESIAN_POINT('Ctrl Pts',(0.339596871275645,-8.11815012964898,
9.93000932090549));
#73527=CARTESIAN_POINT('Ctrl Pts',(0.129908328179361,-8.12692177984522,
9.9217889414016));
#73528=CARTESIAN_POINT('Ctrl Pts',(-0.0801224669385747,-8.12756492708978,
9.91356856189771));
#73529=CARTESIAN_POINT('Ctrl Pts',(-0.289854776901162,-8.1200783106327,
9.90534818239382));
#73530=CARTESIAN_POINT('Ctrl Pts',(-0.499586310701988,-8.11259172188153,
9.89712783331131));
#73531=CARTESIAN_POINT('Ctrl Pts',(-0.709019066696316,-8.0969754428084,
9.88890748422879));
#73532=CARTESIAN_POINT('Ctrl Pts',(-0.917514476546098,-8.0732802966222,
9.88068713514627));
#73533=CARTESIAN_POINT('Ctrl Pts',(-1.12605446549789,-8.04958008409743,
9.87246502844338));
#73534=CARTESIAN_POINT('Ctrl Pts',(-1.33365641459504,-8.01779758684553,
9.86424292174049));
#73535=CARTESIAN_POINT('Ctrl Pts',(-1.53968791938338,-7.97803538933019,
9.8560208150376));
#73536=CARTESIAN_POINT('Ctrl Pts',(-1.63004391307954,-7.9605975083045,9.85241497513375));
#73537=CARTESIAN_POINT('Ctrl Pts',(-1.72009797489201,-7.94162555890349,
9.8488091352299));
#73538=CARTESIAN_POINT('Ctrl Pts',(-1.80979738244364,-7.92113129527596,
9.84520329532605));
#73539=CARTESIAN_POINT('Ctrl Pts',(-2.01433305267289,-7.8743995713847,9.83698113531849));
#73540=CARTESIAN_POINT('Ctrl Pts',(-2.21709148047456,-7.81973376785216,
9.82875897531093));
#73541=CARTESIAN_POINT('Ctrl Pts',(-2.41745253144821,-7.75729403985015,
9.82053681530337));
#73542=CARTESIAN_POINT('Ctrl Pts',(-2.61777665001656,-7.69486582131732,
9.81231617088052));
#73543=CARTESIAN_POINT('Ctrl Pts',(-2.81570399210626,-7.62466662607666,
9.80409552645767));
#73544=CARTESIAN_POINT('Ctrl Pts',(-3.01062944502338,-7.54690651242337,
9.79587488203482));
#73545=CARTESIAN_POINT('Ctrl Pts',(-3.20553299938062,-7.46915513459436,
9.78765516114593));
#73546=CARTESIAN_POINT('Ctrl Pts',(-3.39743506381779,-7.38384464347193,
9.77943544025704));
#73547=CARTESIAN_POINT('Ctrl Pts',(-3.58574959755062,-7.29123359838138,
9.77121571936814));
#73548=CARTESIAN_POINT('Ctrl Pts',(-3.77407922021035,-7.19861513272025,
9.7629953398643));
#73549=CARTESIAN_POINT('Ctrl Pts',(-3.95882047173939,-7.09869507207521,
9.75477496036045));
#73550=CARTESIAN_POINT('Ctrl Pts',(-4.13941010083388,-6.99177885660112,
9.7465545808566));
#73551=CARTESIAN_POINT('Ctrl Pts',(-4.31999906161615,-6.88486303679434,
9.73833423177411));
#73552=CARTESIAN_POINT('Ctrl Pts',(-4.49643617808616,-6.77095126660788,
9.73011388269161));
#73553=CARTESIAN_POINT('Ctrl Pts',(-4.66818502193127,-6.65039368485179,
9.72189353360911));
#73554=CARTESIAN_POINT('Ctrl Pts',(-4.83997058797186,-6.52981032627539,
9.71367142690625));
#73555=CARTESIAN_POINT('Ctrl Pts',(-5.00706563713683,-6.40257848692383,
9.70544932020339));
#73556=CARTESIAN_POINT('Ctrl Pts',(-5.16896391786744,-6.26909080954204,
9.69722721350052));
#73557=CARTESIAN_POINT('Ctrl Pts',(-5.23996509823912,-6.21054922024035,
9.69362137359653));
#73558=CARTESIAN_POINT('Ctrl Pts',(-5.30996720149048,-6.15080497822461,
9.69001553369255));
#73559=CARTESIAN_POINT('Ctrl Pts',(-5.37892955424479,-6.08989362903589,
9.68640969378856));
#73560=CARTESIAN_POINT('Ctrl Pts',(-5.53617987981134,-5.95100147834681,
9.67818753378101));
#73561=CARTESIAN_POINT('Ctrl Pts',(-5.68807366831926,-5.80599248851161,
9.66996537377346));
#73562=CARTESIAN_POINT('Ctrl Pts',(-5.83414298636272,-5.65530398627472,
9.66174321376591));
#73563=CARTESIAN_POINT('Ctrl Pts',(-5.98018537955678,-5.50464326033803,
9.65352256934304));
#73564=CARTESIAN_POINT('Ctrl Pts',(-6.12040523976354,-5.34830532328191,
9.64530192492017));
#73565=CARTESIAN_POINT('Ctrl Pts',(-6.25437169963365,-5.18676413627241,
9.6370812804973));
#73566=CARTESIAN_POINT('Ctrl Pts',(-6.38832310927675,-5.02524109732429,
9.62886155960831));
#73567=CARTESIAN_POINT('Ctrl Pts',(-6.51602233279856,-4.85851620253131,
9.62064183871932));
#73568=CARTESIAN_POINT('Ctrl Pts',(-6.63707845469368,-4.68709687853164,
9.61242211783033));
#73569=CARTESIAN_POINT('Ctrl Pts',(-6.75814427635433,-4.51566381935504,
9.60420173832644));
#73570=CARTESIAN_POINT('Ctrl Pts',(-6.87256576033579,-4.33953581891294,
9.59598135882255));
#73571=CARTESIAN_POINT('Ctrl Pts',(-6.97999443232209,-4.15925056798129,
9.58776097931866));
#73572=CARTESIAN_POINT('Ctrl Pts',(-7.08742270674293,-3.97896598423826,
9.57954063023625));
#73573=CARTESIAN_POINT('Ctrl Pts',(-7.18785807214671,-3.79452443569092,
9.57132028115384));
#73574=CARTESIAN_POINT('Ctrl Pts',(-7.28099699332299,-3.60649003127994,
9.56309993207143));
#73575=CARTESIAN_POINT('Ctrl Pts',(-7.37415582884511,-3.41841542260084,
9.55487782536855));
#73576=CARTESIAN_POINT('Ctrl Pts',(-7.46001497237877,-3.22674668787325,
9.54665571866566));
#73577=CARTESIAN_POINT('Ctrl Pts',(-7.53831772282828,-3.03207082242369,
9.53843361196278));
#73578=CARTESIAN_POINT('Ctrl Pts',(-7.57265772744753,-2.94669489270962,
9.53482777205886));
#73579=CARTESIAN_POINT('Ctrl Pts',(-7.60554503229144,-2.86074086957279,
9.53122193215495));
#73580=CARTESIAN_POINT('Ctrl Pts',(-7.6369609270188,-2.77425942580864,9.52761609225104));
#73581=CARTESIAN_POINT('Ctrl Pts',(-7.70849460051845,-2.57734205593301,
9.51940563138029));
#73582=CARTESIAN_POINT('Ctrl Pts',(-7.77242068385816,-2.3776215238446,9.51119517050955));
#73583=CARTESIAN_POINT('Ctrl Pts',(-7.82853754939877,-2.17570388613743,
9.5029847096388));
#73584=CARTESIAN_POINT('Ctrl Pts',(-7.88464584510249,-1.97381708410153,
9.49477550262124));
#73585=CARTESIAN_POINT('Ctrl Pts',(-7.93294722207455,-1.76973413150191,
9.48656629560367));
#73586=CARTESIAN_POINT('Ctrl Pts',(-7.97329009568077,-1.56407564159122,
9.47835708858611));
#73587=CARTESIAN_POINT('Ctrl Pts',(-8.0136274393253,-1.35844534212574,9.47014900683793));
#73588=CARTESIAN_POINT('Ctrl Pts',(-8.04600840102247,-1.15124022782422,
9.46194092508974));
#73589=CARTESIAN_POINT('Ctrl Pts',(-8.07033249590858,-0.943091176918756,
9.45373284334155));
#73590=CARTESIAN_POINT('Ctrl Pts',(-8.0946573894938,-0.734935291289829,
9.44552449207511));
#73591=CARTESIAN_POINT('Ctrl Pts',(-8.11092485171777,-0.525835701756375,
9.43731614080867));
#73592=CARTESIAN_POINT('Ctrl Pts',(-8.11908615222914,-0.31642947900122,
9.42910778954223));
#73593=CARTESIAN_POINT('Ctrl Pts',(-8.12319752730466,-0.210938016740431,
9.42497271195736));
#73594=CARTESIAN_POINT('Ctrl Pts',(-8.12525255032656,-0.105368806605526,
9.42083763437249));
#73595=CARTESIAN_POINT('Ctrl Pts',(-8.12524999762445,0.000196478821525156,
9.41670255678762));
#73596=CARTESIAN_POINT('Ctrl Pts',(-8.12524999762442,0.000196479806864624,
9.41670255674902));
#73597=CARTESIAN_POINT('Ctrl Pts',(-8.12524471491808,0.218658164704561,
9.40814523591463));
#73598=CARTESIAN_POINT('Ctrl Pts',(-8.11642450034241,0.437076972197306,
9.39958791508024));
#73599=CARTESIAN_POINT('Ctrl Pts',(-8.09882569277387,0.65475946771759,9.39103059424584));
#73600=CARTESIAN_POINT('Ctrl Pts',(-8.0836014519127,0.843070563804878,9.38362789306841));
#73601=CARTESIAN_POINT('Ctrl Pts',(-8.0618085813484,1.03083057646112,9.37622519189097));
#73602=CARTESIAN_POINT('Ctrl Pts',(-8.0335019284137,1.21759366320348,9.36882249071354));
#73603=CARTESIAN_POINT('Ctrl Pts',(-8.00206180620298,1.42503091426872,9.36060033070596));
#73604=CARTESIAN_POINT('Ctrl Pts',(-7.96257768277085,1.63128399695455,9.35237817069839));
#73605=CARTESIAN_POINT('Ctrl Pts',(-7.91516329965985,1.83572261036843,9.34415601069081));
#73606=CARTESIAN_POINT('Ctrl Pts',(-7.86775765640737,2.04012353976234,9.33593536626797));
#73607=CARTESIAN_POINT('Ctrl Pts',(-7.81242473763258,2.24271038005284,9.32771472184513));
#73608=CARTESIAN_POINT('Ctrl Pts',(-7.74932916429956,2.44286411120968,9.31949407742229));
#73609=CARTESIAN_POINT('Ctrl Pts',(-7.68624067932869,2.64299535644468,9.31127435653341));
#73610=CARTESIAN_POINT('Ctrl Pts',(-7.6153913695498,2.84069375687948,9.30305463564453));
#73611=CARTESIAN_POINT('Ctrl Pts',(-7.53699563737041,3.03535571634684,9.29483491475565));
#73612=CARTESIAN_POINT('Ctrl Pts',(-7.45859362363877,3.23003327333762,9.28661453525176));
#73613=CARTESIAN_POINT('Ctrl Pts',(-7.37264408705129,3.42167362842161,9.27839415574786));
#73614=CARTESIAN_POINT('Ctrl Pts',(-7.27940987131439,3.6096924367473,9.27017377624397));
#73615=CARTESIAN_POINT('Ctrl Pts',(-7.18617600061185,3.79771054926673,9.26195342716146));
#73616=CARTESIAN_POINT('Ctrl Pts',(-7.08565763819809,3.98210687860411,9.25373307807894));
#73617=CARTESIAN_POINT('Ctrl Pts',(-6.9781641919283,4.1623205154084,9.24551272899642));
#73618=CARTESIAN_POINT('Ctrl Pts',(-6.87064776212451,4.34257268429433,9.23729062229352));
#73619=CARTESIAN_POINT('Ctrl Pts',(-6.75615342022911,4.51864012045031,9.22906851559062));
#73620=CARTESIAN_POINT('Ctrl Pts',(-6.63503519819217,4.68998885726299,9.22084640888772));
#73621=CARTESIAN_POINT('Ctrl Pts',(-6.58191828620201,4.76513457538729,9.2172405689838));
#73622=CARTESIAN_POINT('Ctrl Pts',(-6.52752796543296,4.83937312278643,9.2136347290799));
#73623=CARTESIAN_POINT('Ctrl Pts',(-6.47189666834279,4.91266130287785,9.21002888917599));
#73624=CARTESIAN_POINT('Ctrl Pts',(-6.34504427381251,5.07977552853205,9.20180672916842));
#73625=CARTESIAN_POINT('Ctrl Pts',(-6.21169477128387,5.24200142133564,9.19358456916085));
#73626=CARTESIAN_POINT('Ctrl Pts',(-6.07224959442057,5.39883991479273,9.18536240915328));
#73627=CARTESIAN_POINT('Ctrl Pts',(-5.93283012138445,5.55564949832535,9.17714176473043));
#73628=CARTESIAN_POINT('Ctrl Pts',(-5.78731741259613,5.70707344405449,9.16892112030758));
#73629=CARTESIAN_POINT('Ctrl Pts',(-5.63615218318239,5.85264693369662,9.16070047588474));
#73630=CARTESIAN_POINT('Ctrl Pts',(-5.48500393616324,5.99820406913843,9.15248075499588));
#73631=CARTESIAN_POINT('Ctrl Pts',(-5.32820464880557,6.137911856017,9.14426103410703));
#73632=CARTESIAN_POINT('Ctrl Pts',(-5.16623137140413,6.27134283703417,9.13604131321817));
#73633=CARTESIAN_POINT('Ctrl Pts',(-5.0042451156988,6.40478450936936,9.12782093371428));
#73634=CARTESIAN_POINT('Ctrl Pts',(-4.83708426766641,6.53194818115257,9.11960055421039));
#73635=CARTESIAN_POINT('Ctrl Pts',(-4.66525920478921,6.65244647589363,9.1113801747065));
#73636=CARTESIAN_POINT('Ctrl Pts',(-4.49343477778953,6.77294432470348,9.10315982562398));
#73637=CARTESIAN_POINT('Ctrl Pts',(-4.31694641365142,6.88677667853716,9.09493947654147));
#73638=CARTESIAN_POINT('Ctrl Pts',(-4.13633416683445,6.99359901787184,9.08671912745896));
#73639=CARTESIAN_POINT('Ctrl Pts',(-3.95568330270774,7.10044419724886,9.07849702075606));
#73640=CARTESIAN_POINT('Ctrl Pts',(-3.77090704844366,7.20027621746656,9.07027491405315));
#73641=CARTESIAN_POINT('Ctrl Pts',(-3.58257175390296,7.29279556758838,9.06205280735025));
#73642=CARTESIAN_POINT('Ctrl Pts',(-3.49997650855884,7.33337032252757,9.05844696744633));
#73643=CARTESIAN_POINT('Ctrl Pts',(-3.4166970663496,7.37253923135409,9.05484112754241));
#73644=CARTESIAN_POINT('Ctrl Pts',(-3.33278257356546,7.41027987864415,9.05123528763849));
#73645=CARTESIAN_POINT('Ctrl Pts',(-3.14143786470172,7.49633739896573,9.04301312763092));
#73646=CARTESIAN_POINT('Ctrl Pts',(-2.94672659509682,7.57499394102922,9.03479096762335));
#73647=CARTESIAN_POINT('Ctrl Pts',(-2.74924004207116,7.64600331896165,9.02656880761579));
#73648=CARTESIAN_POINT('Ctrl Pts',(-2.55178989159727,7.71699960778742,9.01834816319296));
#73649=CARTESIAN_POINT('Ctrl Pts',(-2.3515657563126,7.78035144602788,9.01012751877012));
#73650=CARTESIAN_POINT('Ctrl Pts',(-2.14917702228249,7.83586151545527,9.00190687434729));
#73651=CARTESIAN_POINT('Ctrl Pts',(-1.94681102526134,7.89136534870083,8.9936871534584));
#73652=CARTESIAN_POINT('Ctrl Pts',(-1.742281199502,7.93902909389111,8.98546743256951));
#73653=CARTESIAN_POINT('Ctrl Pts',(-1.53621096335487,7.97870562425813,8.97724771168062));
#73654=CARTESIAN_POINT('Ctrl Pts',(-1.33012421558289,8.01838533375473,8.96902733217674));
#73655=CARTESIAN_POINT('Ctrl Pts',(-1.12249710011702,8.0500764911892,8.96080695267286));
#73656=CARTESIAN_POINT('Ctrl Pts',(-0.913963124964075,8.07368311049585,
8.95258657316898));
#73657=CARTESIAN_POINT('Ctrl Pts',(-0.705429921538258,8.09728964244086,
8.94436622408647));
#73658=CARTESIAN_POINT('Ctrl Pts',(-0.495990158709673,8.11281166555987,
8.93614587500396));
#73659=CARTESIAN_POINT('Ctrl Pts',(-0.28628290060111,8.12020502594136,8.92792552592145));
#73660=CARTESIAN_POINT('Ctrl Pts',(-0.0765308042804336,8.12759996712204,
8.91970341921853));
#73661=CARTESIAN_POINT('Ctrl Pts',(0.133488606562358,8.12686276294456,8.91148131251562));
#73662=CARTESIAN_POINT('Ctrl Pts',(0.343134710536223,8.1180013632005,8.9032592058127));
#73663=CARTESIAN_POINT('Ctrl Pts',(0.435075902097195,8.11411515861132,8.89965336590879));
#73664=CARTESIAN_POINT('Ctrl Pts',(0.526945307312809,8.10866710404108,8.89604752600489));
#73665=CARTESIAN_POINT('Ctrl Pts',(0.618689045347321,8.10166102892902,8.89244168610098));
#73666=CARTESIAN_POINT('Ctrl Pts',(0.827886268162179,8.08568553580354,8.88421952609341));
#73667=CARTESIAN_POINT('Ctrl Pts',(1.0364989135919,8.06160038919091,8.87599736608584));
#73668=CARTESIAN_POINT('Ctrl Pts',(1.24388998304645,8.02947229103985,8.86777520607827));
#73669=CARTESIAN_POINT('Ctrl Pts',(1.45124282425733,7.99735011503754,8.85955456165543));
#73670=CARTESIAN_POINT('Ctrl Pts',(1.65737424738856,7.95718799162515,8.85133391723258));
#73671=CARTESIAN_POINT('Ctrl Pts',(1.86165473178512,7.90910419846155,8.84311327280973));
#73672=CARTESIAN_POINT('Ctrl Pts',(2.06591226664706,7.8610258071878,8.83489355192084));
#73673=CARTESIAN_POINT('Ctrl Pts',(2.26831899073408,7.80502759047416,8.82667383103195));
#73674=CARTESIAN_POINT('Ctrl Pts',(2.46825707432388,7.74127861386929,8.81845411014306));
#73675=CARTESIAN_POINT('Ctrl Pts',(2.66821117819268,7.67752452930114,8.81023373063917));
#73676=CARTESIAN_POINT('Ctrl Pts',(2.86569596429976,7.60601853100322,8.80201335113527));
#73677=CARTESIAN_POINT('Ctrl Pts',(3.06010921012636,7.52697941970083,8.79379297163138));
#73678=CARTESIAN_POINT('Ctrl Pts',(3.25452173648234,7.44794060090072,8.78557262254887));
#73679=CARTESIAN_POINT('Ctrl Pts',(3.44586247288917,7.3613688384916,8.77735227346638));
#73680=CARTESIAN_POINT('Ctrl Pts',(3.63354911586303,7.26753110658021,8.76913192438387));
#73681=CARTESIAN_POINT('Ctrl Pts',(3.82127588874745,7.17367331090867,8.76090981768097));
#73682=CARTESIAN_POINT('Ctrl Pts',(4.00534674328393,7.07254657403411,8.75268771097805));
#73683=CARTESIAN_POINT('Ctrl Pts',(4.18520293643357,6.96446436873417,8.74446560427515));
#73684=CARTESIAN_POINT('Ctrl Pts',(4.26407963575847,6.91706445739098,8.74085976437125));
#73685=CARTESIAN_POINT('Ctrl Pts',(4.342146063272,6.86832738927524,8.73725392446735));
#73686=CARTESIAN_POINT('Ctrl Pts',(4.41935673691357,6.81828230527284,8.73364808456345));
#73687=CARTESIAN_POINT('Ctrl Pts',(4.59997103006115,6.70121484495554,8.72521315976963));
#73688=CARTESIAN_POINT('Ctrl Pts',(4.77596165233416,6.57694690403634,8.71677823497582));
#73689=CARTESIAN_POINT('Ctrl Pts',(4.94675954817621,6.44587135576157,8.708343310182));
#73690=CARTESIAN_POINT('',(-8.12524999914414,0.000117932813409655,9.58329744318989));
#73691=CARTESIAN_POINT('Ctrl Pts',(-8.12524999914414,0.000117932813416063,
9.58329744318989));
#73692=CARTESIAN_POINT('Ctrl Pts',(-8.12524687827972,0.215137000972684,
9.57487617318252));
#73693=CARTESIAN_POINT('Ctrl Pts',(-8.11670432117231,0.430123072685182,
9.56645490317514));
#73694=CARTESIAN_POINT('Ctrl Pts',(-8.09965616022477,0.644404879429754,
9.55803363316777));
#73695=CARTESIAN_POINT('Ctrl Pts',(-8.08260242067832,0.858756804720182,
9.54960960750319));
#73696=CARTESIAN_POINT('Ctrl Pts',(-8.05703753698575,1.07240374231327,9.5411855818386));
#73697=CARTESIAN_POINT('Ctrl Pts',(-8.0230472757909,1.2846789376822,9.53276155617401));
#73698=CARTESIAN_POINT('Ctrl Pts',(-8.00537532901957,1.39504337212792,9.52838180362397));
#73699=CARTESIAN_POINT('Ctrl Pts',(-7.98542678141814,1.50503712219184,9.52400205107392));
#73700=CARTESIAN_POINT('Ctrl Pts',(-7.96321917898033,1.614567394078,9.51962229852387));
#73701=CARTESIAN_POINT('Ctrl Pts',(-7.92152859063276,1.82018983754495,9.5114001385163));
#73702=CARTESIAN_POINT('Ctrl Pts',(-7.87186263879791,2.02423057697928,9.50317797850873));
#73703=CARTESIAN_POINT('Ctrl Pts',(-7.81436618878319,2.22606572906147,9.49495581850116));
#73704=CARTESIAN_POINT('Ctrl Pts',(-7.75688033704689,2.42786367701829,9.48673517407831));
#73705=CARTESIAN_POINT('Ctrl Pts',(-7.69156694875712,2.62745656534174,9.47851452965545));
#73706=CARTESIAN_POINT('Ctrl Pts',(-7.61862114646925,2.82423430137648,9.4702938852326));
#73707=CARTESIAN_POINT('Ctrl Pts',(-7.5456835391503,3.02098993075972,9.4620741643437));
#73708=CARTESIAN_POINT('Ctrl Pts',(-7.4651153322199,3.21493076262044,9.4538544434548));
#73709=CARTESIAN_POINT('Ctrl Pts',(-7.37716060335633,3.40546457840736,9.4456347225659));
#73710=CARTESIAN_POINT('Ctrl Pts',(-7.28919882701457,3.59601366094492,9.43741434306201));
#73711=CARTESIAN_POINT('Ctrl Pts',(-7.19384946738251,3.78315491282193,9.42919396355811));
#73712=CARTESIAN_POINT('Ctrl Pts',(-7.09140402891963,3.9663177458598,9.42097358405421));
#73713=CARTESIAN_POINT('Ctrl Pts',(-6.98895896957954,4.1494799010617,9.41275323497171));
#73714=CARTESIAN_POINT('Ctrl Pts',(-6.87941803034309,4.32866341058893,9.40453288588921));
#73715=CARTESIAN_POINT('Ctrl Pts',(-6.76311806007029,4.50332340256072,9.39631253680671));
#73716=CARTESIAN_POINT('Ctrl Pts',(-6.64679322331064,4.6780207391714,9.38809043010379));
#73717=CARTESIAN_POINT('Ctrl Pts',(-6.52370663195679,4.84819238025677,9.37986832340088));
#73718=CARTESIAN_POINT('Ctrl Pts',(-6.39423836763975,5.01332257692478,9.37164621669796));
#73719=CARTESIAN_POINT('Ctrl Pts',(-6.33745950905437,5.08574112778933,9.36804037679409));
#73720=CARTESIAN_POINT('Ctrl Pts',(-6.27945380601907,5.15719046178532,9.36443453689022));
#73721=CARTESIAN_POINT('Ctrl Pts',(-6.22025579367882,5.22762904419442,9.36082869698635));
#73722=CARTESIAN_POINT('Ctrl Pts',(-6.08527045251885,5.38824551933327,9.35260653697878));
#73723=CARTESIAN_POINT('Ctrl Pts',(-5.94403846854405,5.54365741341841,9.34438437697121));
#73724=CARTESIAN_POINT('Ctrl Pts',(-5.79698553565942,5.69338618590514,9.33616221696363));
#73725=CARTESIAN_POINT('Ctrl Pts',(-5.64995970893422,5.84308735899689,9.32794157254079));
#73726=CARTESIAN_POINT('Ctrl Pts',(-5.49711528150511,5.98710729082194,9.31972092811796));
#73727=CARTESIAN_POINT('Ctrl Pts',(-5.33891548163119,6.12500359530496,9.31150028369512));
#73728=CARTESIAN_POINT('Ctrl Pts',(-5.18073345443798,6.26288440806808,9.30328056280625));
#73729=CARTESIAN_POINT('Ctrl Pts',(-5.01719747833007,6.39464277307387,9.29506084191737));
#73730=CARTESIAN_POINT('Ctrl Pts',(-4.84880521885444,6.51987542151765,9.2868411210285));
#73731=CARTESIAN_POINT('Ctrl Pts',(-4.68039946674644,6.64511810437804,9.2786207415246));
#73732=CARTESIAN_POINT('Ctrl Pts',(-4.50713688898706,6.76383384758233,9.2704003620207));
#73733=CARTESIAN_POINT('Ctrl Pts',(-4.32954644922633,6.87566106687143,9.2621799825168));
#73734=CARTESIAN_POINT('Ctrl Pts',(-4.15195666667983,6.98748787231822,9.2539596334343));
#73735=CARTESIAN_POINT('Ctrl Pts',(-3.97003930534624,7.09242604983562,9.24573928435181));
#73736=CARTESIAN_POINT('Ctrl Pts',(-3.7843508435604,7.19015829139691,9.23751893526931));
#73737=CARTESIAN_POINT('Ctrl Pts',(-3.59862267910182,7.28791142941651,9.22929682856641));
#73738=CARTESIAN_POINT('Ctrl Pts',(-3.40912206456737,7.37845541591847,9.22107472186351));
#73739=CARTESIAN_POINT('Ctrl Pts',(-3.21642950883962,7.46151920034826,9.21285261516061));
#73740=CARTESIAN_POINT('Ctrl Pts',(-3.13192336804865,7.49794717669194,9.20924677525668));
#73741=CARTESIAN_POINT('Ctrl Pts',(-3.04680360442628,7.53293710030239,9.20564093535275));
#73742=CARTESIAN_POINT('Ctrl Pts',(-2.96112041560347,7.56646902106896,9.20203509544882));
#73743=CARTESIAN_POINT('Ctrl Pts',(-2.76574266527916,7.64292965860399,9.19381293544125));
#73744=CARTESIAN_POINT('Ctrl Pts',(-2.56736959657649,7.71183144184668,9.18559077543368));
#73745=CARTESIAN_POINT('Ctrl Pts',(-2.3666039701597,7.77295781610349,9.17736861542611));
#73746=CARTESIAN_POINT('Ctrl Pts',(-2.16587535072395,7.83407292298046,9.16914797100329));
#73747=CARTESIAN_POINT('Ctrl Pts',(-1.96275533599007,7.88741539549,9.16092732658046));
#73748=CARTESIAN_POINT('Ctrl Pts',(-1.75786234917643,7.93281838465043,9.15270668215763));
#73749=CARTESIAN_POINT('Ctrl Pts',(-1.55299238070759,7.97821627309134,9.14448696126874));
#73750=CARTESIAN_POINT('Ctrl Pts',(-1.34635012585057,8.01567639506547,9.13626724037985));
#73751=CARTESIAN_POINT('Ctrl Pts',(-1.13856553327261,8.04508272729023,9.12804751949097));
#73752=CARTESIAN_POINT('Ctrl Pts',(-0.930764291704717,8.07449141573266,
9.11982713998708));
#73753=CARTESIAN_POINT('Ctrl Pts',(-0.721820821386084,8.09584498095052,
9.11160676048318));
#73754=CARTESIAN_POINT('Ctrl Pts',(-0.512372611573524,8.1090789778747,9.10338638097929));
#73755=CARTESIAN_POINT('Ctrl Pts',(-0.302925176871561,8.12231292582346,
9.09516603189678));
#73756=CARTESIAN_POINT('Ctrl Pts',(-0.0929733011369583,8.12742734963881,
9.08694568281426));
#73757=CARTESIAN_POINT('Ctrl Pts',(0.116842548040901,8.12440984819619,9.07872533373175));
#73758=CARTESIAN_POINT('Ctrl Pts',(0.326703258648862,8.12139170157148,9.07050322702884));
#73759=CARTESIAN_POINT('Ctrl Pts',(0.536427589422058,8.11023816032079,9.06228112032593));
#73760=CARTESIAN_POINT('Ctrl Pts',(0.745376101833266,8.09098894013061,9.05405901362302));
#73761=CARTESIAN_POINT('Ctrl Pts',(0.837011361644048,8.08254711265394,9.05045317371912));
#73762=CARTESIAN_POINT('Ctrl Pts',(0.928497453617433,8.07254891838278,9.04684733381522));
#73763=CARTESIAN_POINT('Ctrl Pts',(1.01978075318514,8.06100085460442,9.04324149391132));
#73764=CARTESIAN_POINT('Ctrl Pts',(1.22792806839248,8.03466856290712,9.03501933390375));
#73765=CARTESIAN_POINT('Ctrl Pts',(1.43508927608202,8.00026559575085,9.02679717389618));
#73766=CARTESIAN_POINT('Ctrl Pts',(1.64063147025403,7.95789016896514,9.01857501388861));
#73767=CARTESIAN_POINT('Ctrl Pts',(1.84613577698402,7.9155225532108,9.01035436946577));
#73768=CARTESIAN_POINT('Ctrl Pts',(2.05002137690645,7.86518547042578,9.00213372504293));
#73769=CARTESIAN_POINT('Ctrl Pts',(2.25166539097638,7.80702827774943,8.99391308062009));
#73770=CARTESIAN_POINT('Ctrl Pts',(2.45328675170146,7.74887761864139,8.9856933597312));
#73771=CARTESIAN_POINT('Ctrl Pts',(2.65266674585659,7.68290868533619,8.97747363884231));
#73772=CARTESIAN_POINT('Ctrl Pts',(2.84919669008664,7.60932098046201,8.96925391795342));
#73773=CARTESIAN_POINT('Ctrl Pts',(3.04574238151431,7.53572737928467,8.96103353844953));
#73774=CARTESIAN_POINT('Ctrl Pts',(3.2394372893541,7.4545138877133,8.95281315894564));
#73775=CARTESIAN_POINT('Ctrl Pts',(3.42969078517489,7.36592890819525,8.94459277944175));
#73776=CARTESIAN_POINT('Ctrl Pts',(3.61994357691957,7.27734425650596,8.93637243035924));
#73777=CARTESIAN_POINT('Ctrl Pts',(3.80675471568613,7.18138829844081,8.92815208127672));
#73778=CARTESIAN_POINT('Ctrl Pts',(3.98955585702429,7.07835656252094,8.9199317321942));
#73779=CARTESIAN_POINT('Ctrl Pts',(4.17239608368721,6.97530279704025,8.91170962549129));
#73780=CARTESIAN_POINT('Ctrl Pts',(4.35122434285274,6.86517037618022,8.90348751878839));
#73781=CARTESIAN_POINT('Ctrl Pts',(4.52549812791133,6.7483001012678,8.89526541208548));
#73782=CARTESIAN_POINT('Ctrl Pts',(4.60192663839813,6.69704614457698,8.89165957218159));
#73783=CARTESIAN_POINT('Ctrl Pts',(4.67747954967086,6.6444968675941,8.88805373227769));
#73784=CARTESIAN_POINT('Ctrl Pts',(4.75211288108001,6.59068363130665,8.8844478923738));
#73785=CARTESIAN_POINT('Ctrl Pts',(4.81770694146005,6.54338802485793,8.88127877643176));
#73786=CARTESIAN_POINT('Ctrl Pts',(4.88259905651463,6.49511008660576,8.87810966048971));
#73787=CARTESIAN_POINT('Ctrl Pts',(4.9467595481762,6.44587135576158,8.87494054454767));
#73788=CARTESIAN_POINT('Ctrl Pts',(4.94675954817619,6.44587135576158,10.8749423500932));
#73789=CARTESIAN_POINT('Ctrl Pts',(5.11325382428399,6.31809853737967,10.8667219683852));
#73790=CARTESIAN_POINT('Ctrl Pts',(5.27479679333856,6.18387015657815,10.8585015866772));
#73791=CARTESIAN_POINT('Ctrl Pts',(5.43089607779182,6.04359622697657,10.8502812049692));
#73792=CARTESIAN_POINT('Ctrl Pts',(5.58699470910173,5.90332288430262,10.8420608576566));
#73793=CARTESIAN_POINT('Ctrl Pts',(5.73764948361426,5.75700424267344,10.8338405103439));
#73794=CARTESIAN_POINT('Ctrl Pts',(5.88240309512541,5.6050888832345,10.8256201630313));
#73795=CARTESIAN_POINT('Ctrl Pts',(6.02718771561716,5.45314098063215,10.8173980547636));
#73796=CARTESIAN_POINT('Ctrl Pts',(6.16606844392976,5.29559417869845,10.809175946496));
#73797=CARTESIAN_POINT('Ctrl Pts',(6.29862590212076,5.13293281736996,10.8009538382284));
#73798=CARTESIAN_POINT('Ctrl Pts',(6.35764735912206,5.06050754100724,10.7972929290936));
#73799=CARTESIAN_POINT('Ctrl Pts',(6.41541575706434,4.98706875720691,10.7936320199588));
#73800=CARTESIAN_POINT('Ctrl Pts',(6.47189666834309,4.91266130287745,10.789971110824));
#73801=CARTESIAN_POINT('Ctrl Pts',(6.59874906287325,4.74554707722338,10.7817489508164));
#73802=CARTESIAN_POINT('Ctrl Pts',(6.71914621451919,4.57348936598663,10.7735267908089));
#73803=CARTESIAN_POINT('Ctrl Pts',(6.83271537167142,4.39700900752148,10.7653046308013));
#73804=CARTESIAN_POINT('Ctrl Pts',(6.94626359470415,4.22056117955148,10.7570839863785));
#73805=CARTESIAN_POINT('Ctrl Pts',(7.05298617559616,4.03969257949409,10.7488633419556));
#73806=CARTESIAN_POINT('Ctrl Pts',(7.15255391163893,3.85495267203096,10.7406426975328));
#73807=CARTESIAN_POINT('Ctrl Pts',(7.25211046191814,3.67023351885036,10.7324229766439));
#73808=CARTESIAN_POINT('Ctrl Pts',(7.34451363210237,3.48164418625025,10.724203255755));
#73809=CARTESIAN_POINT('Ctrl Pts',(7.42947997433496,3.28975909048913,10.7159835348662));
#73810=CARTESIAN_POINT('Ctrl Pts',(7.51445312459773,3.09785861970432,10.7077631553623));
#73811=CARTESIAN_POINT('Ctrl Pts',(7.59198813427315,2.90266212688007,10.6995427758584));
#73812=CARTESIAN_POINT('Ctrl Pts',(7.66184912124185,2.70476535134297,10.6913223963545));
#73813=CARTESIAN_POINT('Ctrl Pts',(7.73170984967406,2.50686930816796,10.683102047272));
#73814=CARTESIAN_POINT('Ctrl Pts',(7.79389651647753,2.30627328146959,10.6748816981895));
#73815=CARTESIAN_POINT('Ctrl Pts',(7.84822249773654,2.10359007140697,10.666661349107));
#73816=CARTESIAN_POINT('Ctrl Pts',(7.90256009461575,1.90086352496766,10.6584392424041));
#73817=CARTESIAN_POINT('Ctrl Pts',(7.94903357177258,1.69604918874693,10.6502171357012));
#73818=CARTESIAN_POINT('Ctrl Pts',(7.98750672664966,1.48977308816695,10.6419950289983));
#73819=CARTESIAN_POINT('Ctrl Pts',(8.00437929253806,1.39930982594273,10.6383891890944));
#73820=CARTESIAN_POINT('Ctrl Pts',(8.01971381833703,1.3085655631382,10.6347833491904));
#73821=CARTESIAN_POINT('Ctrl Pts',(8.03350192841366,1.21759366320376,10.6311775092865));
#73822=CARTESIAN_POINT('Ctrl Pts',(8.06494205062438,1.01015641213862,10.6229553492789));
#73823=CARTESIAN_POINT('Ctrl Pts',(8.08834854780176,0.801466532148104,10.6147331892714));
#73824=CARTESIAN_POINT('Ctrl Pts',(8.10364328115617,0.59215972023803,10.6065110292638));
#73825=CARTESIAN_POINT('Ctrl Pts',(8.1189351952436,0.38289148969915,10.5982903848409));
#73826=CARTESIAN_POINT('Ctrl Pts',(8.12611830829277,0.173006848417312,10.5900697404181));
#73827=CARTESIAN_POINT('Ctrl Pts',(8.12516641861186,-0.0368542041301155,
10.5818490959953));
#73828=CARTESIAN_POINT('Ctrl Pts',(8.12421463586934,-0.246691680203768,
10.5736293751064));
#73829=CARTESIAN_POINT('Ctrl Pts',(8.11512967629721,-0.456505277809638,
10.5654096542175));
#73830=CARTESIAN_POINT('Ctrl Pts',(8.09793745429763,-0.665654977284556,
10.5571899333286));
#73831=CARTESIAN_POINT('Ctrl Pts',(8.08074385475061,-0.874821435130248,
10.5489695538247));
#73832=CARTESIAN_POINT('Ctrl Pts',(8.05544171626132,-1.08332359416993,10.5407491743208));
#73833=CARTESIAN_POINT('Ctrl Pts',(8.022108923528,-1.29052546722349,10.5325287948169));
#73834=CARTESIAN_POINT('Ctrl Pts',(7.98877625415026,-1.49772657347944,10.5243084457344));
#73835=CARTESIAN_POINT('Ctrl Pts',(7.94741303949096,-1.70362711240172,10.5160880966519));
#73836=CARTESIAN_POINT('Ctrl Pts',(7.89814858156644,-1.90759968179911,10.5078677475694));
#73837=CARTESIAN_POINT('Ctrl Pts',(7.848873590243,-2.11161586325541,10.4996456408665));
#73838=CARTESIAN_POINT('Ctrl Pts',(7.79169404988503,-2.31370296468734,10.4914235341636));
#73839=CARTESIAN_POINT('Ctrl Pts',(7.72678986617589,-2.51324609349373,10.4832014274606));
#73840=CARTESIAN_POINT('Ctrl Pts',(7.69832586005151,-2.60075658227635,10.4795955875568));
#73841=CARTESIAN_POINT('Ctrl Pts',(7.66837682174596,-2.68777798204506,10.4759897476529));
#73842=CARTESIAN_POINT('Ctrl Pts',(7.63696092701891,-2.77425942580834,10.472383907749));
#73843=CARTESIAN_POINT('Ctrl Pts',(7.56532532474245,-2.97145738447055,10.4641617477414));
#73844=CARTESIAN_POINT('Ctrl Pts',(7.48603589155157,-3.16591179019283,10.4559395877339));
#73845=CARTESIAN_POINT('Ctrl Pts',(7.39932814761351,-3.35702703689356,10.4477174277263));
#73846=CARTESIAN_POINT('Ctrl Pts',(7.31263638645032,-3.548107055461,10.4394967833035));
#73847=CARTESIAN_POINT('Ctrl Pts',(7.21852916558492,-3.7358488748302,10.4312761388806));
#73848=CARTESIAN_POINT('Ctrl Pts',(7.11728967093991,-3.91967795902061,10.4230554944578));
#73849=CARTESIAN_POINT('Ctrl Pts',(7.01606154986932,-4.10348639125324,10.4148357735689));
#73850=CARTESIAN_POINT('Ctrl Pts',(6.90770289700708,-4.28338270744836,10.40661605268));
#73851=CARTESIAN_POINT('Ctrl Pts',(6.79254267244258,-4.45881728775093,10.3983963317911));
#73852=CARTESIAN_POINT('Ctrl Pts',(6.67737322052681,-4.6342659249599,10.3901759522872));
#73853=CARTESIAN_POINT('Ctrl Pts',(6.5554012676622,-4.80525186371131,10.3819555727833));
#73854=CARTESIAN_POINT('Ctrl Pts',(6.42699948116171,-4.97125388927653,10.3737351932794));
#73855=CARTESIAN_POINT('Ctrl Pts',(6.29859816984121,-5.13725530051354,10.3655148441969));
#73856=CARTESIAN_POINT('Ctrl Pts',(6.16376725517245,-5.29827260363649,10.3572944951144));
#73857=CARTESIAN_POINT('Ctrl Pts',(6.02292044805656,-5.45381672215725,10.3490741460319));
#73858=CARTESIAN_POINT('Ctrl Pts',(5.88204352601259,-5.60939409808753,10.340852039329));
#73859=CARTESIAN_POINT('Ctrl Pts',(5.73514833993392,-5.75949573268095,10.3326299326261));
#73860=CARTESIAN_POINT('Ctrl Pts',(5.58268705217846,-5.90366774471082,10.3244078259232));
#73861=CARTESIAN_POINT('Ctrl Pts',(5.51582450526036,-5.96689499446413,10.3208019860193));
#73862=CARTESIAN_POINT('Ctrl Pts',(5.44789190699709,-6.02898227984894,10.3171961461154));
#73863=CARTESIAN_POINT('Ctrl Pts',(5.3789295542444,-6.08989362903624,10.3135903062115));
#73864=CARTESIAN_POINT('Ctrl Pts',(5.22167922867744,-6.22878577972567,10.3053681462039));
#73865=CARTESIAN_POINT('Ctrl Pts',(5.05902046870411,-6.36160692986553,10.2971459861963));
#73866=CARTESIAN_POINT('Ctrl Pts',(4.89144504598925,-6.48794674181032,10.2889238261888));
#73867=CARTESIAN_POINT('Ctrl Pts',(4.72390051232906,-6.61426326563032,10.2807031817659));
#73868=CARTESIAN_POINT('Ctrl Pts',(4.55144136029741,-6.73410065812387,10.2724825373431));
#73869=CARTESIAN_POINT('Ctrl Pts',(4.37459113756181,-6.84708988853408,10.2642618929202));
#73870=CARTESIAN_POINT('Ctrl Pts',(4.19776078275603,-6.96006642536627,10.2560421720313));
#73871=CARTESIAN_POINT('Ctrl Pts',(4.01654059071647,-7.0661961772169,10.2478224511424));
#73872=CARTESIAN_POINT('Ctrl Pts',(3.83148238401016,-7.16515389252176,10.2396027302535));
#73873=CARTESIAN_POINT('Ctrl Pts',(3.64640934929288,-7.26411953693237,10.2313823507496));
#73874=CARTESIAN_POINT('Ctrl Pts',(3.45749794443206,-7.35591185496512,10.2231619712457));
#73875=CARTESIAN_POINT('Ctrl Pts',(3.26532478261787,-7.44025144914616,10.2149415917418));
#73876=CARTESIAN_POINT('Ctrl Pts',(3.07315233198413,-7.52459073120938,10.2067212426593));
#73877=CARTESIAN_POINT('Ctrl Pts',(2.87771841987778,-7.60147722842589,10.1985008935768));
#73878=CARTESIAN_POINT('Ctrl Pts',(2.67962032507399,-7.67067940119716,10.1902805444943));
#73879=CARTESIAN_POINT('Ctrl Pts',(2.48147987425246,-7.73989637031698,10.1820584377914));
#73880=CARTESIAN_POINT('Ctrl Pts',(2.28067438139625,-7.80142563521947,10.1738363310885));
#73881=CARTESIAN_POINT('Ctrl Pts',(2.07781805207946,-7.85508495848089,10.1656142243856));
#73882=CARTESIAN_POINT('Ctrl Pts',(1.98885454510534,-7.87861748317593,10.1620083844817));
#73883=CARTESIAN_POINT('Ctrl Pts',(1.89949678999567,-7.90063703164834,10.1584025445778));
#73884=CARTESIAN_POINT('Ctrl Pts',(1.80979738244314,-7.92113129527607,10.1547967046739));
#73885=CARTESIAN_POINT('Ctrl Pts',(1.60526171221374,-7.96786301916735,10.1465745446664));
#73886=CARTESIAN_POINT('Ctrl Pts',(1.39888129661992,-8.00667608629494,10.1383523846588));
#73887=CARTESIAN_POINT('Ctrl Pts',(1.19128429069491,-8.03744544623747,10.1301302246512));
#73888=CARTESIAN_POINT('Ctrl Pts',(0.983725550973688,-8.06820913448647,
10.1219095802284));
#73889=CARTESIAN_POINT('Ctrl Pts',(0.774950960306297,-8.0909320315456,10.1136889358055));
#73890=CARTESIAN_POINT('Ctrl Pts',(0.565596814653767,-8.10554056221752,
10.1054682913827));
#73891=CARTESIAN_POINT('Ctrl Pts',(0.356266188527402,-8.12014745171955,
10.0972485704938));
#73892=CARTESIAN_POINT('Ctrl Pts',(0.146356431712985,-8.12664177423147,
10.0890288496049));
#73893=CARTESIAN_POINT('Ctrl Pts',(-0.0634922761331844,-8.12500192574571,
10.080809128716));
#73894=CARTESIAN_POINT('Ctrl Pts',(-0.273357798358859,-8.12336194586511,
10.0725887492121));
#73895=CARTESIAN_POINT('Ctrl Pts',(-0.48316196667668,-8.11358649228104,
10.0643683697082));
#73896=CARTESIAN_POINT('Ctrl Pts',(-0.692264770060775,-8.09570608721887,
10.0561479902043));
#73897=CARTESIAN_POINT('Ctrl Pts',(-0.901366799612261,-8.07782574832722,
10.0479276411218));
#73898=CARTESIAN_POINT('Ctrl Pts',(-1.10976717557884,-8.05184054576274,
10.0397072920393));
#73899=CARTESIAN_POINT('Ctrl Pts',(-1.31683063653816,-8.017832914022,10.0314869429568));
#73900=CARTESIAN_POINT('Ctrl Pts',(-1.52393837043037,-7.98381801099548,
10.0232648362539));
#73901=CARTESIAN_POINT('Ctrl Pts',(-1.72970832694089,-7.9417772997943,10.015042729551));
#73902=CARTESIAN_POINT('Ctrl Pts',(-1.93351396837177,-7.89184460671973,
10.0068206228481));
#73903=CARTESIAN_POINT('Ctrl Pts',(-2.02289380021593,-7.86994641156086,
10.0032147829442));
#73904=CARTESIAN_POINT('Ctrl Pts',(-2.11189597997634,-7.84653101254412,
9.99960894304032));
#73905=CARTESIAN_POINT('Ctrl Pts',(-2.2004684331936,-7.82161276445072,9.99600310313642));
#73906=CARTESIAN_POINT('Ctrl Pts',(-2.40243438343677,-7.76479331921943,
9.98778094312886));
#73907=CARTESIAN_POINT('Ctrl Pts',(-2.60223173787426,-7.70013771404643,
9.97955878312129));
#73908=CARTESIAN_POINT('Ctrl Pts',(-2.79924906934294,-7.62783666646597,
9.97133662311373));
#73909=CARTESIAN_POINT('Ctrl Pts',(-2.99623008475156,-7.55554894608453,
9.96311597869088));
#73910=CARTESIAN_POINT('Ctrl Pts',(-3.19043182301468,-7.47561869765075,
9.95489533426804));
#73911=CARTESIAN_POINT('Ctrl Pts',(-3.38126033544734,-7.38828573529953,
9.94667468984519));
#73912=CARTESIAN_POINT('Ctrl Pts',(-3.57206740958418,-7.30096258421738,
9.93845496895628));
#73913=CARTESIAN_POINT('Ctrl Pts',(-3.75950174618789,-7.2062385023116,9.93023524806737));
#73914=CARTESIAN_POINT('Ctrl Pts',(-3.94299085072363,-7.10440079905475,
9.92201552717846));
#73915=CARTESIAN_POINT('Ctrl Pts',(-4.12649465754374,-7.00255493592989,
9.91379514767456));
#73916=CARTESIAN_POINT('Ctrl Pts',(-4.30605234126817,-6.8935944534058,9.90557476817066));
#73917=CARTESIAN_POINT('Ctrl Pts',(-4.4811164941428,-6.77785235369002,9.89735438866676));
#73918=CARTESIAN_POINT('Ctrl Pts',(-4.65617999915263,-6.66211068230426,
9.88913403958425));
#73919=CARTESIAN_POINT('Ctrl Pts',(-4.82674976184907,-6.53958760893002,
9.88091369050175));
#73920=CARTESIAN_POINT('Ctrl Pts',(-4.99230738156593,-6.41065944895393,
9.87269334141924));
#73921=CARTESIAN_POINT('Ctrl Pts',(-5.15790039971245,-6.28170372241576,
9.86447123471634));
#73922=CARTESIAN_POINT('Ctrl Pts',(-5.3184789009949,-6.14634035467356,9.85624912801343));
#73923=CARTESIAN_POINT('Ctrl Pts',(-5.47355673260854,-6.00498661592311,
9.84802702131052));
#73924=CARTESIAN_POINT('Ctrl Pts',(-5.54156677597637,-5.94299533191693,
9.84442118140665));
#73925=CARTESIAN_POINT('Ctrl Pts',(-5.60851931880421,-5.87985243111227,
9.84081534150277));
#73926=CARTESIAN_POINT('Ctrl Pts',(-5.67437550088683,-5.81559543275109,
9.83720950159889));
#73927=CARTESIAN_POINT('Ctrl Pts',(-5.8245430293976,-5.66907441789309,9.82898734159132));
#73928=CARTESIAN_POINT('Ctrl Pts',(-5.96905721080625,-5.51670978455476,
9.82076518158375));
#73929=CARTESIAN_POINT('Ctrl Pts',(-6.10747237968127,-5.35896153129787,
9.81254302157618));
#73930=CARTESIAN_POINT('Ctrl Pts',(-6.24586203458983,-5.20124235566068,
9.80432237715334));
#73931=CARTESIAN_POINT('Ctrl Pts',(-6.37815472620382,-5.03814176245311,
9.79610173273049));
#73932=CARTESIAN_POINT('Ctrl Pts',(-6.50394362663989,-4.87015450103899,
9.78788108830764));
#73933=CARTESIAN_POINT('Ctrl Pts',(-6.62971839554145,-4.7021861118606,9.77966136741874));
#73934=CARTESIAN_POINT('Ctrl Pts',(-6.74899065513564,-4.5293323866415,9.77144164652984));
#73935=CARTESIAN_POINT('Ctrl Pts',(-6.86139514013848,-4.3521195173598,9.76322192564094));
#73936=CARTESIAN_POINT('Ctrl Pts',(-6.97380863168544,-4.17489244868447,
9.75500154613706));
#73937=CARTESIAN_POINT('Ctrl Pts',(-7.07935308871106,-3.99330578582776,
9.74678116663316));
#73938=CARTESIAN_POINT('Ctrl Pts',(-7.17770713602157,-3.80791384251338,
9.73856078712928));
#73939=CARTESIAN_POINT('Ctrl Pts',(-7.27606081935097,-3.62252258528328,
9.73034043804673));
#73940=CARTESIAN_POINT('Ctrl Pts',(-7.36722401023294,-3.4333263377414,9.7221200889642));
#73941=CARTESIAN_POINT('Ctrl Pts',(-7.45092152763993,-3.24090357021801,
9.71389973988166));
#73942=CARTESIAN_POINT('Ctrl Pts',(-7.53463694069338,-3.04843966013836,
9.70567763317876));
#73943=CARTESIAN_POINT('Ctrl Pts',(-7.6108833735059,-2.85274812254923,9.69745552647585));
#73944=CARTESIAN_POINT('Ctrl Pts',(-7.67943355671181,-2.65442796296086,
9.68923341977295));
#73945=CARTESIAN_POINT('Ctrl Pts',(-7.70949653143982,-2.56745381253664,
9.6856275798691));
#73946=CARTESIAN_POINT('Ctrl Pts',(-7.7380799203174,-2.47997433612477,9.68202173996524));
#73947=CARTESIAN_POINT('Ctrl Pts',(-7.76516754947262,-2.39204107220535,
9.67841590006139));
#73948=CARTESIAN_POINT('Ctrl Pts',(-7.82718015449563,-2.19073254377822,
9.67016093154966));
#73949=CARTESIAN_POINT('Ctrl Pts',(-7.88136995031025,-1.98698011876507,
9.66190596303793));
#73950=CARTESIAN_POINT('Ctrl Pts',(-7.92756461528397,-1.78140585858405,
9.6536509945262));
#73951=CARTESIAN_POINT('Ctrl Pts',(-7.97374954254046,-1.57587493293127,
9.64539776614071));
#73952=CARTESIAN_POINT('Ctrl Pts',(-8.01194263992958,-1.36852322183758,
9.63714453775523));
#73953=CARTESIAN_POINT('Ctrl Pts',(-8.0420223270444,-1.15998467826921,9.62889130936975));
#73954=CARTESIAN_POINT('Ctrl Pts',(-8.07209976663542,-0.951461716489887,
9.62063869765714));
#73955=CARTESIAN_POINT('Ctrl Pts',(-8.09406496248538,-0.741752386149109,
9.61238608594453));
#73956=CARTESIAN_POINT('Ctrl Pts',(-8.10784785788655,-0.531498519155556,
9.60413347423193));
#73957=CARTESIAN_POINT('Ctrl Pts',(-8.11944745189462,-0.354550249233417,
9.59718813055875));
#73958=CARTESIAN_POINT('Ctrl Pts',(-8.12525257302793,-0.177216522463021,
9.59024278688558));
#73959=CARTESIAN_POINT('Ctrl Pts',(-8.12524999914415,0.000117932238638647,
9.5832974432124));
#73960=CARTESIAN_POINT('Origin',(0.,0.,24.4167025567876));
#73961=CARTESIAN_POINT('',(4.94675954817619,6.44587135576159,12.8749480452876));
#73962=CARTESIAN_POINT('',(4.94717300284007,6.4464104346866,12.7083501623644));
#73963=CARTESIAN_POINT('',(4.9467595481762,6.44587135576158,24.4167025567876));
#73964=CARTESIAN_POINT('',(-8.12524999887474,-0.000135225956416249,11.4167025567876));
#73965=CARTESIAN_POINT('Ctrl Pts',(4.94717300284021,6.44641043468649,12.7083501623644));
#73966=CARTESIAN_POINT('Ctrl Pts',(4.97999127047003,6.42124041604394,12.7067294825768));
#73967=CARTESIAN_POINT('Ctrl Pts',(6.0780585597953,5.56544170535072,12.6521776022766));
#73968=CARTESIAN_POINT('Ctrl Pts',(7.79448477834709,3.31475408317713,12.5446945214639));
#73969=CARTESIAN_POINT('Ctrl Pts',(8.43041607796892,-0.818335105043671,
12.3859009199263));
#73970=CARTESIAN_POINT('Ctrl Pts',(7.01145427209639,-4.75195713176425,12.2271073183889));
#73971=CARTESIAN_POINT('Ctrl Pts',(3.88346779769395,-7.52730133953051,12.0683137168513));
#73972=CARTESIAN_POINT('Ctrl Pts',(-0.191104364661067,-8.46788442963361,
11.9095201153138));
#73973=CARTESIAN_POINT('Ctrl Pts',(-4.21909530993973,-7.34444159602813,
11.7507265137763));
#73974=CARTESIAN_POINT('Ctrl Pts',(-7.21869218977298,-4.43080925578325,
11.5919329122388));
#73975=CARTESIAN_POINT('Ctrl Pts',(-8.08818406800785,-1.63059466065753,
11.4805915932426));
#73976=CARTESIAN_POINT('Ctrl Pts',(-8.12586896382392,-0.139963263173689,
11.4221814747588));
#73977=CARTESIAN_POINT('Ctrl Pts',(-8.12575905226067,-0.000135234428430032,
11.4167025567876));
#73978=CARTESIAN_POINT('Ctrl Pts',(-8.12524999887474,-0.000135225956416249,
11.4167025567876));
#73979=CARTESIAN_POINT('Ctrl Pts',(-8.12525347870505,0.208955484150721,
11.4085091877829));
#73980=CARTESIAN_POINT('Ctrl Pts',(-8.11718167762833,0.418082135971698,
11.4003158187783));
#73981=CARTESIAN_POINT('Ctrl Pts',(-8.10105234256317,0.626608734021274,
11.3921224497736));
#73982=CARTESIAN_POINT('Ctrl Pts',(-8.08492580849104,0.835099119694661,
11.3839305036156));
#73983=CARTESIAN_POINT('Ctrl Pts',(-8.06074455612332,1.0429893613643,11.3757385574575));
#73984=CARTESIAN_POINT('Ctrl Pts',(-8.02857832661406,1.24964699652463,11.3675466112995));
#73985=CARTESIAN_POINT('Ctrl Pts',(-7.99641086333345,1.45631255826735,11.3593543509303));
#73986=CARTESIAN_POINT('Ctrl Pts',(-7.95625785296927,1.66174512272453,11.351162090561));
#73987=CARTESIAN_POINT('Ctrl Pts',(-7.90824060897219,1.86531982059464,11.3429698301918));
#73988=CARTESIAN_POINT('Ctrl Pts',(-7.86022522159834,2.0688866470943,11.3347778865826));
#73989=CARTESIAN_POINT('Ctrl Pts',(-7.80434627867582,2.27059545968444,11.3265859429733));
#73990=CARTESIAN_POINT('Ctrl Pts',(-7.74077579324093,2.46983353311014,11.3183939993641));
#73991=CARTESIAN_POINT('Ctrl Pts',(-7.67718969083417,2.66912055213322,11.3102000432902));
#73992=CARTESIAN_POINT('Ctrl Pts',(-7.60590836011643,2.86593533353154,11.3020060872164));
#73993=CARTESIAN_POINT('Ctrl Pts',(-7.52715345565799,3.05968109734919,11.2938121311425));
#73994=CARTESIAN_POINT('Ctrl Pts',(-7.46478731695495,3.21310868719226,11.2873233238162));
#73995=CARTESIAN_POINT('Ctrl Pts',(-7.39773542812496,3.36461194318915,11.28083451649));
#73996=CARTESIAN_POINT('Ctrl Pts',(-7.32612922650967,3.5139035443479,11.2743457091637));
#73997=CARTESIAN_POINT('Ctrl Pts',(-7.23539488695969,3.70307535525159,11.2661235491561));
#73998=CARTESIAN_POINT('Ctrl Pts',(-7.13731460211681,3.88876215565963,11.2579013891486));
#73999=CARTESIAN_POINT('Ctrl Pts',(-7.03218148356007,4.07039447041375,11.249679229141));
#74000=CARTESIAN_POINT('Ctrl Pts',(-6.92706774411427,4.25199330501598,11.2414585847182));
#74001=CARTESIAN_POINT('Ctrl Pts',(-6.81490391344161,4.42953889028286,11.2332379402953));
#74002=CARTESIAN_POINT('Ctrl Pts',(-6.6960284585416,4.60248741930936,11.2250172958725));
#74003=CARTESIAN_POINT('Ctrl Pts',(-6.57716635849726,4.77541651873498,11.2167975749836));
#74004=CARTESIAN_POINT('Ctrl Pts',(-6.45159430666074,4.94374934984069,11.2085778540948));
#74005=CARTESIAN_POINT('Ctrl Pts',(-6.31969386378421,5.10697141469856,11.2003581332059));
#74006=CARTESIAN_POINT('Ctrl Pts',(-6.18778285222611,5.27020655792062,11.192137753702));
#74007=CARTESIAN_POINT('Ctrl Pts',(-6.04954261984108,5.4283298853786,11.1839173741981));
#74008=CARTESIAN_POINT('Ctrl Pts',(-5.90539542017655,5.58085947626867,11.1756969946942));
#74009=CARTESIAN_POINT('Ctrl Pts',(-5.76124875396172,5.73338850268808,11.1674766456117));
#74010=CARTESIAN_POINT('Ctrl Pts',(-5.61119536885646,5.8803236212733,11.1592562965292));
#74011=CARTESIAN_POINT('Ctrl Pts',(-5.45569519238787,6.02121894056808,11.1510359474468));
#74012=CARTESIAN_POINT('Ctrl Pts',(-5.30016176790476,6.16214438516388,11.1428138407438));
#74013=CARTESIAN_POINT('Ctrl Pts',(-5.13917944418118,6.29702725230902,11.1345917340409));
#74014=CARTESIAN_POINT('Ctrl Pts',(-4.97324294174114,6.42546046637297,11.126369627338));
#74015=CARTESIAN_POINT('Ctrl Pts',(-4.90047078204565,6.48178539926375,11.1227637874341));
#74016=CARTESIAN_POINT('Ctrl Pts',(-4.8267462124903,6.53687039501838,11.1191579475301));
#74017=CARTESIAN_POINT('Ctrl Pts',(-4.75211288108026,6.59068363130647,11.1155521076262));
#74018=CARTESIAN_POINT('Ctrl Pts',(-4.58193139518513,6.71339042114571,11.1073299476186));
#74019=CARTESIAN_POINT('Ctrl Pts',(-4.40696657212852,6.8295224185167,11.0991077876111));
#74020=CARTESIAN_POINT('Ctrl Pts',(-4.22774825431306,6.93871978542533,11.0908856276035));
#74021=CARTESIAN_POINT('Ctrl Pts',(-4.04856297167875,7.04789702406336,11.0826649831806));
#74022=CARTESIAN_POINT('Ctrl Pts',(-3.8651260110447,7.15014202996808,11.0744443387578));
#74023=CARTESIAN_POINT('Ctrl Pts',(-3.67799476216117,7.24513920446081,11.0662236943349));
#74024=CARTESIAN_POINT('Ctrl Pts',(-3.49088453621112,7.34012570666181,11.0580039734461));
#74025=CARTESIAN_POINT('Ctrl Pts',(-3.30008111365677,7.42786586948591,11.0497842525571));
#74026=CARTESIAN_POINT('Ctrl Pts',(-3.10616570373832,7.50809044853749,11.0415645316683));
#74027=CARTESIAN_POINT('Ctrl Pts',(-2.91223475611538,7.58832145567955,11.0333441521644));
#74028=CARTESIAN_POINT('Ctrl Pts',(-2.71519159458971,7.66103556044727,11.0251237726605));
#74029=CARTESIAN_POINT('Ctrl Pts',(-2.51563757597134,7.72601159388601,11.0169033931566));
#74030=CARTESIAN_POINT('Ctrl Pts',(-2.3160842958477,7.79098738686626,11.0086830440741));
#74031=CARTESIAN_POINT('Ctrl Pts',(-2.11402045868706,7.84822507696063,11.0004626949916));
#74032=CARTESIAN_POINT('Ctrl Pts',(-1.91006326632435,7.89755315785455,10.9922423459091));
#74033=CARTESIAN_POINT('Ctrl Pts',(-1.70606246519036,7.94689178575087,10.9840202392062));
#74034=CARTESIAN_POINT('Ctrl Pts',(-1.50016778702453,7.98831735640183,10.9757981325032));
#74035=CARTESIAN_POINT('Ctrl Pts',(-1.29300841568809,8.02170909466678,10.9675760258003));
#74036=CARTESIAN_POINT('Ctrl Pts',(-1.20215779131438,8.03635318366321,10.9639701858964));
#74037=CARTESIAN_POINT('Ctrl Pts',(-1.11106405275177,8.0494527908262,10.9603643459926));
#74038=CARTESIAN_POINT('Ctrl Pts',(-1.01978075318463,8.06100085460448,10.9567585060887));
#74039=CARTESIAN_POINT('Ctrl Pts',(-0.811633437977397,8.08733314630175,
10.9485363460811));
#74040=CARTESIAN_POINT('Ctrl Pts',(-0.602431320363802,8.1056034529901,10.9403141860736));
#74041=CARTESIAN_POINT('Ctrl Pts',(-0.392811825792572,8.11574928346222,
10.932092026066));
#74042=CARTESIAN_POINT('Ctrl Pts',(-0.183230970229024,8.12589324376085,
10.9238713816432));
#74043=CARTESIAN_POINT('Ctrl Pts',(0.0267668140914816,8.12791570254229,
10.9156507372203));
#74044=CARTESIAN_POINT('Ctrl Pts',(0.236541077043419,8.12180619575296,10.9074300927975));
#74045=CARTESIAN_POINT('Ctrl Pts',(0.446291773272173,8.11569737532549,10.8992103719086));
#74046=CARTESIAN_POINT('Ctrl Pts',(0.655818703362964,8.1014584217971,10.8909906510197));
#74047=CARTESIAN_POINT('Ctrl Pts',(0.864482677904975,8.07913097196117,10.8827709301308));
#74048=CARTESIAN_POINT('Ctrl Pts',(1.07316337189805,8.05680173311156,10.8745505506269));
#74049=CARTESIAN_POINT('Ctrl Pts',(1.2809806784145,8.0263827316729,10.866330171123));
#74050=CARTESIAN_POINT('Ctrl Pts',(1.48730071661944,7.98796745992642,10.8581097916191));
#74051=CARTESIAN_POINT('Ctrl Pts',(1.69361999129065,7.94955233034429,10.8498894425366));
#74052=CARTESIAN_POINT('Ctrl Pts',(1.89844171906582,7.90314104629872,10.8416690934541));
#74053=CARTESIAN_POINT('Ctrl Pts',(2.10114186522571,7.8488782908576,10.8334487443715));
#74054=CARTESIAN_POINT('Ctrl Pts',(2.30388535138336,7.79460393331484,10.8252266376686));
#74055=CARTESIAN_POINT('Ctrl Pts',(2.50450606451344,7.73247482689936,10.8170045309657));
#74056=CARTESIAN_POINT('Ctrl Pts',(2.70239371943027,7.66268593560273,10.8087824242628));
#74057=CARTESIAN_POINT('Ctrl Pts',(2.78917819308923,7.63207972016717,10.8051765843589));
#74058=CARTESIAN_POINT('Ctrl Pts',(2.87543722678284,7.60000094183469,10.801570744455));
#74059=CARTESIAN_POINT('Ctrl Pts',(2.96112041560399,7.56646902106876,10.7979649045512));
#74060=CARTESIAN_POINT('Ctrl Pts',(3.15650058942059,7.49000743510553,10.7897426425548));
#74061=CARTESIAN_POINT('Ctrl Pts',(3.34894985265458,7.40596157228609,10.7815203805584));
#74062=CARTESIAN_POINT('Ctrl Pts',(3.5378785458744,7.31458152987179,10.7732981185621));
#74063=CARTESIAN_POINT('Ctrl Pts',(3.72676958833246,7.22321969818107,10.7650774951439));
#74064=CARTESIAN_POINT('Ctrl Pts',(3.91214119575806,7.12452673301637,10.7568568717256));
#74065=CARTESIAN_POINT('Ctrl Pts',(4.09342597040225,7.01879985377389,10.7486362483074));
#74066=CARTESIAN_POINT('Ctrl Pts',(4.27470096158518,6.9130786803323,10.7404160685346));
#74067=CARTESIAN_POINT('Ctrl Pts',(4.45188930434596,6.80032449748332,10.7321958887617));
#74068=CARTESIAN_POINT('Ctrl Pts',(4.6244495403283,6.6808797333478,10.7239757089889));
#74069=CARTESIAN_POINT('Ctrl Pts',(4.7337876516959,6.60519679950745,10.718767215118));
#74070=CARTESIAN_POINT('Ctrl Pts',(4.84126821146589,6.52682864583457,10.7135587212472));
#74071=CARTESIAN_POINT('Ctrl Pts',(4.9467595481762,6.44587135576158,10.7083502273763));
#74072=CARTESIAN_POINT('',(-8.12524999999793,-5.8050124092788E-6,11.5832974432392));
#74073=CARTESIAN_POINT('Ctrl Pts',(-8.12524999999793,-5.80432776886074E-6,
11.5832974432124));
#74074=CARTESIAN_POINT('Ctrl Pts',(-8.1252501498455,0.209759912077751,11.575076876068));
#74075=CARTESIAN_POINT('Ctrl Pts',(-8.11712282336244,0.419560513241832,
11.5668563089237));
#74076=CARTESIAN_POINT('Ctrl Pts',(-8.10088596652066,0.628756009854853,
11.5586357417793));
#74077=CARTESIAN_POINT('Ctrl Pts',(-8.0846521127155,0.837912815374886,11.550416695044));
#74078=CARTESIAN_POINT('Ctrl Pts',(-8.06031174491846,1.04646444536909,11.5421976483087));
#74079=CARTESIAN_POINT('Ctrl Pts',(-8.02793480465863,1.25377443531546,11.5339786015733));
#74080=CARTESIAN_POINT('Ctrl Pts',(-7.99556150104078,1.46106113979361,11.5257604780176));
#74081=CARTESIAN_POINT('Ctrl Pts',(-7.95515347266073,1.66710619092948,11.5175423544619));
#74082=CARTESIAN_POINT('Ctrl Pts',(-7.90683219188853,1.87128091205336,11.5093242309062));
#74083=CARTESIAN_POINT('Ctrl Pts',(-7.85850705403901,2.0754719307106,11.5011054513675));
#74084=CARTESIAN_POINT('Ctrl Pts',(-7.80226746711589,2.27779203299136,11.4928866718287));
#74085=CARTESIAN_POINT('Ctrl Pts',(-7.73828568192483,2.47762431926577,11.48466789229));
#74086=CARTESIAN_POINT('Ctrl Pts',(-7.67430403741296,2.67745616616131,11.4764491308223));
#74087=CARTESIAN_POINT('Ctrl Pts',(-7.60258032135703,2.87479992751923,11.4682303693545));
#74088=CARTESIAN_POINT('Ctrl Pts',(-7.52333633373635,3.06905489882188,11.4600116078867));
#74089=CARTESIAN_POINT('Ctrl Pts',(-7.44407546709598,3.26335124655675,11.4517910958176));
#74090=CARTESIAN_POINT('Ctrl Pts',(-7.35729124047569,3.45455721635805,11.4435705837484));
#74091=CARTESIAN_POINT('Ctrl Pts',(-7.26325360681933,3.64209206439458,11.4353500716792));
#74092=CARTESIAN_POINT('Ctrl Pts',(-7.22434231723412,3.71969102659236,11.4319485534442));
#74093=CARTESIAN_POINT('Ctrl Pts',(-7.18418967585113,3.79666169270989,11.4285470352091));
#74094=CARTESIAN_POINT('Ctrl Pts',(-7.14281713462595,3.87296410308615,11.4251455169741));
#74095=CARTESIAN_POINT('Ctrl Pts',(-7.04281130476781,4.05740251667848,11.4169233569665));
#74096=CARTESIAN_POINT('Ctrl Pts',(-6.93564143296636,4.23799584074839,11.408701196959));
#74097=CARTESIAN_POINT('Ctrl Pts',(-6.82162851674016,4.41418983983442,11.4004790369514));
#74098=CARTESIAN_POINT('Ctrl Pts',(-6.70763661643125,4.59035136120973,11.3922583925285));
#74099=CARTESIAN_POINT('Ctrl Pts',(-6.58680434948576,4.76211492842893,11.3840377481057));
#74100=CARTESIAN_POINT('Ctrl Pts',(-6.45949673983474,4.92895419237837,11.3758171036829));
#74101=CARTESIAN_POINT('Ctrl Pts',(-6.33220343233532,5.09577471306139,11.367597382794));
#74102=CARTESIAN_POINT('Ctrl Pts',(-6.19843641342503,5.25767180038029,11.3593776619051));
#74103=CARTESIAN_POINT('Ctrl Pts',(-6.05860229397876,5.41415051562988,11.3511579410163));
#74104=CARTESIAN_POINT('Ctrl Pts',(-5.91875697015549,5.57064176892473,11.3429375615124));
#74105=CARTESIAN_POINT('Ctrl Pts',(-5.7728437690881,5.72171356076734,11.3347171820085));
#74106=CARTESIAN_POINT('Ctrl Pts',(-5.62130832848872,5.86690550789454,11.3264968025046));
#74107=CARTESIAN_POINT('Ctrl Pts',(-5.46977344868068,6.01209691770594,11.3182764534221));
#74108=CARTESIAN_POINT('Ctrl Pts',(-5.31261658591901,6.15140832406688,11.3100561043396));
#74109=CARTESIAN_POINT('Ctrl Pts',(-5.15031921841847,6.28441719739303,11.3018357552571));
#74110=CARTESIAN_POINT('Ctrl Pts',(-4.98798714957372,6.41745450979228,11.2936136485542));
#74111=CARTESIAN_POINT('Ctrl Pts',(-4.82051260850807,6.54418640986268,11.2853915418513));
#74112=CARTESIAN_POINT('Ctrl Pts',(-4.64840989828935,6.66423086184637,11.2771694351484));
#74113=CARTESIAN_POINT('Ctrl Pts',(-4.57293352191708,6.71687686740787,11.2735635952444));
#74114=CARTESIAN_POINT('Ctrl Pts',(-4.49656741055537,6.76823722127028,11.2699577553405));
#74115=CARTESIAN_POINT('Ctrl Pts',(-4.41935673691317,6.81828230527309,11.2663519154366));
#74116=CARTESIAN_POINT('Ctrl Pts',(-4.24329830672989,6.93239682483752,11.258129755429));
#74117=CARTESIAN_POINT('Ctrl Pts',(-4.06278854574039,7.03970738493306,11.2499075954214));
#74118=CARTESIAN_POINT('Ctrl Pts',(-3.87837449260932,7.13988087138556,11.2416854354139));
#74119=CARTESIAN_POINT('Ctrl Pts',(-3.69399443238534,7.24003589293281,11.233464790991));
#74120=CARTESIAN_POINT('Ctrl Pts',(-3.50571177561206,7.3330563257284,11.2252441465682));
#74121=CARTESIAN_POINT('Ctrl Pts',(-3.31409888006422,7.41865460684463,11.2170235021453));
#74122=CARTESIAN_POINT('Ctrl Pts',(-3.12250751093267,7.50424327157139,11.2088037812564));
#74123=CARTESIAN_POINT('Ctrl Pts',(-2.92758691932108,7.58241132896441,11.2005840603675));
#74124=CARTESIAN_POINT('Ctrl Pts',(-2.72993095394003,7.65291869480005,11.1923643394786));
#74125=CARTESIAN_POINT('Ctrl Pts',(-2.5322591511377,7.72343171012293,11.1841439599747));
#74126=CARTESIAN_POINT('Ctrl Pts',(-2.33185181371052,7.78628270567305,11.1759235804709));
#74127=CARTESIAN_POINT('Ctrl Pts',(-2.12932052853281,7.84128061283798,11.167703200967));
#74128=CARTESIAN_POINT('Ctrl Pts',(-1.92678999286815,7.89627831647065,11.1594828518844));
#74129=CARTESIAN_POINT('Ctrl Pts',(-1.7221358107046,7.94342291508327,11.1512625028019));
#74130=CARTESIAN_POINT('Ctrl Pts',(-1.51598293110405,7.98257372750801,11.1430421537194));
#74131=CARTESIAN_POINT('Ctrl Pts',(-1.30978597326509,8.02173291089924,11.1348200470165));
#74132=CARTESIAN_POINT('Ctrl Pts',(-1.10208996782934,8.05289483841846,11.1265979403136));
#74133=CARTESIAN_POINT('Ctrl Pts',(-0.893529314802037,8.07597009195115,
11.1183758336107));
#74134=CARTESIAN_POINT('Ctrl Pts',(-0.802064152375844,8.08608984264121,
11.1147699937068));
#74135=CARTESIAN_POINT('Ctrl Pts',(-0.710432783381724,8.09465495381696,
11.1111641538029));
#74136=CARTESIAN_POINT('Ctrl Pts',(-0.618689045347654,8.10166102892899,
11.107558313899));
#74137=CARTESIAN_POINT('Ctrl Pts',(-0.40949182253276,8.11763652205449,11.0993361538915));
#74138=CARTESIAN_POINT('Ctrl Pts',(-0.19964098094302,8.12550763408714,11.0911139938839));
#74139=CARTESIAN_POINT('Ctrl Pts',(0.0102237389347411,8.12524356789765,
11.0828918338763));
#74140=CARTESIAN_POINT('Ctrl Pts',(0.22004977460258,8.12497955038329,11.0746711894535));
#74141=CARTESIAN_POINT('Ctrl Pts',(0.429889388458503,8.11658334791561,11.0664505450306));
#74142=CARTESIAN_POINT('Ctrl Pts',(0.639102399678589,8.1000762765066,11.0582299006078));
#74143=CARTESIAN_POINT('Ctrl Pts',(0.848291907227683,8.08357105955575,11.0500101797189));
#74144=CARTESIAN_POINT('Ctrl Pts',(1.0568546585658,8.05895681601877,11.04179045883));
#74145=CARTESIAN_POINT('Ctrl Pts',(1.26415431630378,8.02630683609034,11.0335707379411));
#74146=CARTESIAN_POINT('Ctrl Pts',(1.47147058417592,7.99365424004304,11.0253503584372));
#74147=CARTESIAN_POINT('Ctrl Pts',(1.67752326424249,7.9529646643056,11.0171299789334));
#74148=CARTESIAN_POINT('Ctrl Pts',(1.88168389325767,7.90436292741892,11.0089095994295));
#74149=CARTESIAN_POINT('Ctrl Pts',(2.08584376673018,7.85576137039399,11.0006892503469));
#74150=CARTESIAN_POINT('Ctrl Pts',(2.28811131665572,7.7992477817398,10.9924689012644));
#74151=CARTESIAN_POINT('Ctrl Pts',(2.48787045291621,7.73499761939243,10.9842485521819));
#74152=CARTESIAN_POINT('Ctrl Pts',(2.68767230034718,7.67073371950248,10.976026445479));
#74153=CARTESIAN_POINT('Ctrl Pts',(2.88496438160005,7.5987300315721,10.9678043387761));
#74154=CARTESIAN_POINT('Ctrl Pts',(3.07914683316719,7.51921155057473,10.9595822320732));
#74155=CARTESIAN_POINT('Ctrl Pts',(3.16430637412174,7.48433838214737,10.9559763921693));
#74156=CARTESIAN_POINT('Ctrl Pts',(3.24886808078214,7.44802052593385,10.9523705522654));
#74157=CARTESIAN_POINT('Ctrl Pts',(3.33278257356589,7.41027987864396,10.9487647123615));
#74158=CARTESIAN_POINT('Ctrl Pts',(3.52412638941611,7.3242227599563,10.9405425907271));
#74159=CARTESIAN_POINT('Ctrl Pts',(3.71216682489899,7.23073633081746,10.9323204690927));
#74160=CARTESIAN_POINT('Ctrl Pts',(3.89632738088859,7.13009961385098,10.9240983474582));
#74161=CARTESIAN_POINT('Ctrl Pts',(4.08046637411999,7.0294746801091,10.9158771885252));
#74162=CARTESIAN_POINT('Ctrl Pts',(4.26072613435067,6.92170126860998,10.9076560295922));
#74163=CARTESIAN_POINT('Ctrl Pts',(4.43655459726775,6.80710444080024,10.8994348706591));
#74164=CARTESIAN_POINT('Ctrl Pts',(4.61116429561427,6.69330194714617,10.8912706971372));
#74165=CARTESIAN_POINT('Ctrl Pts',(4.78140370353987,6.57277050688571,10.8831065236152));
#74166=CARTESIAN_POINT('Ctrl Pts',(4.94675954817619,6.44587135576158,10.8749423500932));
#74167=CARTESIAN_POINT('Ctrl Pts',(4.94675954817619,6.44587135576158,12.8749480452876));
#74168=CARTESIAN_POINT('Ctrl Pts',(5.08620153897348,6.33885929155453,12.8680613404623));
#74169=CARTESIAN_POINT('Ctrl Pts',(5.22215542942478,6.22733177311037,12.861174635637));
#74170=CARTESIAN_POINT('Ctrl Pts',(5.35433288438807,6.11153065325378,12.8542879308117));
#74171=CARTESIAN_POINT('Ctrl Pts',(5.51214191086351,5.97327362602921,12.8460657708041));
#74172=CARTESIAN_POINT('Ctrl Pts',(5.66461910540582,5.8288782131343,12.8378436107966));
#74173=CARTESIAN_POINT('Ctrl Pts',(5.81129477521856,5.67877985116675,12.829621450789));
#74174=CARTESIAN_POINT('Ctrl Pts',(5.95794340841248,5.52870915672035,12.8214008063662));
#74175=CARTESIAN_POINT('Ctrl Pts',(6.09879244506011,5.37293782227638,12.8131801619433));
#74176=CARTESIAN_POINT('Ctrl Pts',(6.23340911041919,5.21193806799764,12.8049595175205));
#74177=CARTESIAN_POINT('Ctrl Pts',(6.36801065250421,5.05095640095501,12.7967397966316));
#74178=CARTESIAN_POINT('Ctrl Pts',(6.49638103188557,4.88474771307027,12.7885200757427));
#74179=CARTESIAN_POINT('Ctrl Pts',(6.61812729041575,4.71381785078234,12.7803003548538));
#74180=CARTESIAN_POINT('Ctrl Pts',(6.73988330401075,4.54287429253442,12.7720799753499));
#74181=CARTESIAN_POINT('Ctrl Pts',(6.85501396277648,4.36720904284507,12.763859595846));
#74182=CARTESIAN_POINT('Ctrl Pts',(6.96316862739231,4.1873583831575,12.7556392163421));
#74183=CARTESIAN_POINT('Ctrl Pts',(7.071322891757,4.00750838904856,12.7474188672596));
#74184=CARTESIAN_POINT('Ctrl Pts',(7.17250106379876,3.82347327023304,12.7391985181771));
#74185=CARTESIAN_POINT('Ctrl Pts',(7.26639733642572,3.63581590728755,12.7309781690946));
#74186=CARTESIAN_POINT('Ctrl Pts',(7.36031368533006,3.44811842069108,12.7227560623917));
#74187=CARTESIAN_POINT('Ctrl Pts',(7.44694489220615,3.25679740669599,12.7145339556888));
#74188=CARTESIAN_POINT('Ctrl Pts',(7.52603189142397,3.06243882090227,12.7063118489859));
#74189=CARTESIAN_POINT('Ctrl Pts',(7.56071583167937,2.97720203553345,12.702706009082));
#74190=CARTESIAN_POINT('Ctrl Pts',(7.59394941469675,2.8913813045124,12.6991001691781));
#74191=CARTESIAN_POINT('Ctrl Pts',(7.62571372598674,2.80502722478721,12.6954943292742));
#74192=CARTESIAN_POINT('Ctrl Pts',(7.69814379967779,2.60811968597999,12.6872721692666));
#74193=CARTESIAN_POINT('Ctrl Pts',(7.76295507009928,2.40837277274515,12.6790500092591));
#74194=CARTESIAN_POINT('Ctrl Pts',(7.81994341318432,2.20639356804157,12.6708278492515));
#74195=CARTESIAN_POINT('Ctrl Pts',(7.87692125164993,2.00445159401645,12.6626072048287));
#74196=CARTESIAN_POINT('Ctrl Pts',(7.92607896069587,1.80027843368315,12.6543865604058));
#74197=CARTESIAN_POINT('Ctrl Pts',(7.96726243329179,1.59449580794602,12.646165915983));
#74198=CARTESIAN_POINT('Ctrl Pts',(8.00844127920236,1.38873630049881,12.6379461950941));
#74199=CARTESIAN_POINT('Ctrl Pts',(8.04164761927169,1.18136797791785,12.6297264742052));
#74200=CARTESIAN_POINT('Ctrl Pts',(8.06677839825177,0.973023039808759,12.6215067533163));
#74201=CARTESIAN_POINT('Ctrl Pts',(8.0919111908656,0.764661407811974,12.6132863738124));
#74202=CARTESIAN_POINT('Ctrl Pts',(8.10896709143555,0.555323296633125,12.6050659943085));
#74203=CARTESIAN_POINT('Ctrl Pts',(8.11789476697463,0.345647385099121,12.5968456148046));
#74204=CARTESIAN_POINT('Ctrl Pts',(8.12682240947486,0.135972249517645,12.5886252657221));
#74205=CARTESIAN_POINT('Ctrl Pts',(8.1276218772276,-0.0740403889280623,
12.5804049166396));
#74206=CARTESIAN_POINT('Ctrl Pts',(8.12029393139912,-0.283749943053032,
12.5721845675571));
#74207=CARTESIAN_POINT('Ctrl Pts',(8.112964418758,-0.493504335880073,12.5639624608542));
#74208=CARTESIAN_POINT('Ctrl Pts',(8.09750403115892,-0.702955219897917,
12.5557403541513));
#74209=CARTESIAN_POINT('Ctrl Pts',(8.07396561443259,-0.911464107609391,
12.5475182474484));
#74210=CARTESIAN_POINT('Ctrl Pts',(8.06364274155181,-1.00290656813609,12.5439124075445));
#74211=CARTESIAN_POINT('Ctrl Pts',(8.05176689539146,-1.09416791368378,12.5403065676406));
#74212=CARTESIAN_POINT('Ctrl Pts',(8.03834567368995,-1.18519466450457,12.5367007277367));
#74213=CARTESIAN_POINT('Ctrl Pts',(8.00774214295416,-1.39275698844776,12.5284785677291));
#74214=CARTESIAN_POINT('Ctrl Pts',(7.96908990209952,-1.59916758506913,12.5202564077215));
#74215=CARTESIAN_POINT('Ctrl Pts',(7.92250015052607,-1.80379570002106,12.512034247714));
#74216=CARTESIAN_POINT('Ctrl Pts',(7.8759189868075,-2.00838609602195,12.5038136032911));
#74217=CARTESIAN_POINT('Ctrl Pts',(7.82140329803518,-2.21119437848746,12.4955929588683));
#74218=CARTESIAN_POINT('Ctrl Pts',(7.75911520809883,-2.41160086870723,12.4873723144455));
#74219=CARTESIAN_POINT('Ctrl Pts',(7.69683411580874,-2.6119848446112,12.4791525935565));
#74220=CARTESIAN_POINT('Ctrl Pts',(7.62678245315554,-2.80996728522362,12.4709328726676));
#74221=CARTESIAN_POINT('Ctrl Pts',(7.54917218725299,-3.00494373486524,12.4627131517786));
#74222=CARTESIAN_POINT('Ctrl Pts',(7.47155570273525,-3.19993580722762,12.4544927722747));
#74223=CARTESIAN_POINT('Ctrl Pts',(7.38637951145395,-3.39192113212285,12.4462723927708));
#74224=CARTESIAN_POINT('Ctrl Pts',(7.29390409904462,-3.58031430972758,12.438052013267));
#74225=CARTESIAN_POINT('Ctrl Pts',(7.20142902886164,-3.7687067901404,12.4298316641844));
#74226=CARTESIAN_POINT('Ctrl Pts',(7.10165492403412,-3.95350688608519,12.4216113151019));
#74227=CARTESIAN_POINT('Ctrl Pts',(6.99488892845406,-4.1341524453134,12.4133909660194));
#74228=CARTESIAN_POINT('Ctrl Pts',(6.88810010487836,-4.31483662897457,12.4051688593165));
#74229=CARTESIAN_POINT('Ctrl Pts',(6.77431655411192,-4.49136424714162,12.3969467526136));
#74230=CARTESIAN_POINT('Ctrl Pts',(6.65389015240542,-4.66319991017135,12.3887246459107));
#74231=CARTESIAN_POINT('Ctrl Pts',(6.60107664116816,-4.73855917185967,12.3851188060069));
#74232=CARTESIAN_POINT('Ctrl Pts',(6.54698607401266,-4.81301640426677,12.381512966103));
#74233=CARTESIAN_POINT('Ctrl Pts',(6.49165070897511,-4.88652828040143,12.3779071261992));
#74234=CARTESIAN_POINT('Ctrl Pts',(6.3654731088736,-5.0541525854609,12.3696849661916));
#74235=CARTESIAN_POINT('Ctrl Pts',(6.23277874502435,-5.21691479214037,12.3614628061841));
#74236=CARTESIAN_POINT('Ctrl Pts',(6.09396703571509,-5.37431421951842,12.3532406461765));
#74237=CARTESIAN_POINT('Ctrl Pts',(5.95518091346581,-5.53168463357612,12.3450200017536));
#74238=CARTESIAN_POINT('Ctrl Pts',(5.81027989142122,-5.6836940200293,12.3367993573307));
#74239=CARTESIAN_POINT('Ctrl Pts',(5.65970280709325,-5.82987578751732,12.3285787129079));
#74240=CARTESIAN_POINT('Ctrl Pts',(5.50914263908526,-5.97604113246958,12.320358992019));
#74241=CARTESIAN_POINT('Ctrl Pts',(5.35290789353397,-6.11637996000327,12.31213927113));
#74242=CARTESIAN_POINT('Ctrl Pts',(5.19147389345428,-6.25046289294502,12.3039195502411));
#74243=CARTESIAN_POINT('Ctrl Pts',(5.03002695828155,-6.38455656944272,12.2956991707372));
#74244=CARTESIAN_POINT('Ctrl Pts',(4.86338016148537,-6.5123931590959,12.2874787912333));
#74245=CARTESIAN_POINT('Ctrl Pts',(4.69204231459319,-6.63358323084643,12.2792584117294));
#74246=CARTESIAN_POINT('Ctrl Pts',(4.52070510177493,-6.75477285410607,12.2710380626468));
#74247=CARTESIAN_POINT('Ctrl Pts',(4.34467711608927,-6.86931584041031,12.2628177135642));
#74248=CARTESIAN_POINT('Ctrl Pts',(4.16449701858858,-6.97686549566973,12.2545973644817));
#74249=CARTESIAN_POINT('Ctrl Pts',(3.98427839617798,-7.08443814648103,12.2463752577787));
#74250=CARTESIAN_POINT('Ctrl Pts',(3.79990614182762,-7.1850143276905,12.2381531510758));
#74251=CARTESIAN_POINT('Ctrl Pts',(3.6119453932408,-7.27829224741262,12.2299310443729));
#74252=CARTESIAN_POINT('Ctrl Pts',(3.52951440662434,-7.3191996762776,12.2263252044691));
#74253=CARTESIAN_POINT('Ctrl Pts',(3.44639356067816,-7.35870402896952,12.2227193645654));
#74254=CARTESIAN_POINT('Ctrl Pts',(3.36263191091955,-7.39678269210104,12.2191135246617));
#74255=CARTESIAN_POINT('Ctrl Pts',(3.17163571996251,-7.4836109677596,12.2108913646541));
#74256=CARTESIAN_POINT('Ctrl Pts',(2.97724315670334,-7.56305189845629,12.2026692046466));
#74257=CARTESIAN_POINT('Ctrl Pts',(2.78004450109596,-7.6348569164344,12.194447044639));
#74258=CARTESIAN_POINT('Ctrl Pts',(2.58288219497156,-7.70664869864641,12.1862264002162));
#74259=CARTESIAN_POINT('Ctrl Pts',(2.38291510603868,-7.77080727642779,12.1780057557933));
#74260=CARTESIAN_POINT('Ctrl Pts',(2.18075181987134,-7.82713287625985,12.1697851113704));
#74261=CARTESIAN_POINT('Ctrl Pts',(1.97861124538436,-7.88345214829104,12.1615653904815));
#74262=CARTESIAN_POINT('Ctrl Pts',(1.77427525044028,-7.93194012001247,12.1533456695925));
#74263=CARTESIAN_POINT('Ctrl Pts',(1.56836665514373,-7.97244715238259,12.1451259487036));
#74264=CARTESIAN_POINT('Ctrl Pts',(1.3624415611755,-8.01295743042696,12.1369055691997));
#74265=CARTESIAN_POINT('Ctrl Pts',(1.15494390415697,-8.04548543172001,12.1286851896958));
#74266=CARTESIAN_POINT('Ctrl Pts',(0.946506799953877,-8.06993261682779,
12.1204648101919));
#74267=CARTESIAN_POINT('Ctrl Pts',(0.73807046712045,-8.09437971146312,12.1122444611094));
#74268=CARTESIAN_POINT('Ctrl Pts',(0.528694987502466,-8.11074601800417,
12.1040241120269));
#74269=CARTESIAN_POINT('Ctrl Pts',(0.319019242010997,-8.11898480634905,
12.0958037629444));
#74270=CARTESIAN_POINT('Ctrl Pts',(0.109298665043695,-8.12722535625695,
12.0875816562415));
#74271=CARTESIAN_POINT('Ctrl Pts',(-0.10072201108176,-8.12733490464745,
12.0793595495385));
#74272=CARTESIAN_POINT('Ctrl Pts',(-0.310402138129443,-8.11931881841972,
12.0711374428356));
#74273=CARTESIAN_POINT('Ctrl Pts',(-0.402358250652034,-8.11580332967253,
12.0675316029318));
#74274=CARTESIAN_POINT('Ctrl Pts',(-0.494248874407456,-8.11072571421347,
12.0639257630279));
#74275=CARTESIAN_POINT('Ctrl Pts',(-0.58602011355852,-8.10408958421641,
12.0603199231241));
#74276=CARTESIAN_POINT('Ctrl Pts',(-0.795280045368397,-8.08895765264925,
12.0520977631165));
#74277=CARTESIAN_POINT('Ctrl Pts',(-1.00398810067131,-8.06571377663445,
12.043875603109));
#74278=CARTESIAN_POINT('Ctrl Pts',(-1.21150701712862,-8.03442208935703,
12.0356534431014));
#74279=CARTESIAN_POINT('Ctrl Pts',(-1.41898768177649,-8.00313617005334,
12.0274327986786));
#74280=CARTESIAN_POINT('Ctrl Pts',(-1.62527935336111,-7.96380544422755,
12.0192121542557));
#74281=CARTESIAN_POINT('Ctrl Pts',(-1.82975203947748,-7.9165456505049,12.0109915098328));
#74282=CARTESIAN_POINT('Ctrl Pts',(-2.03420175446741,-7.86929116610114,
12.0027717889439));
#74283=CARTESIAN_POINT('Ctrl Pts',(-2.23683260451198,-7.81410945861269,
11.994552068055));
#74284=CARTESIAN_POINT('Ctrl Pts',(-2.43702608327965,-7.75116710127673,
11.9863323471661));
#74285=CARTESIAN_POINT('Ctrl Pts',(-2.63723560278937,-7.68821970060906,
11.9781119676622));
#74286=CARTESIAN_POINT('Ctrl Pts',(-2.83500707841521,-7.61751049353422,
11.9698915881583));
#74287=CARTESIAN_POINT('Ctrl Pts',(-3.02973741038233,-7.53925585098621,
11.9616712086544));
#74288=CARTESIAN_POINT('Ctrl Pts',(-3.22446702170616,-7.46100149803706,
11.9534508595718));
#74289=CARTESIAN_POINT('Ctrl Pts',(-3.41615523902162,-7.37520187800216,
11.9452305104893));
#74290=CARTESIAN_POINT('Ctrl Pts',(-3.60421868720372,-7.28212161511406,
11.9370101614068));
#74291=CARTESIAN_POINT('Ctrl Pts',(-3.79232234586194,-7.18902145042302,
11.9287880547038));
#74292=CARTESIAN_POINT('Ctrl Pts',(-3.97679942246783,-7.08863766384462,
11.9205659480009));
#74293=CARTESIAN_POINT('Ctrl Pts',(-4.15708991467862,-6.98128147289431,
11.912343841298));
#74294=CARTESIAN_POINT('Ctrl Pts',(-4.23615707770353,-6.93419995823697,
11.9087380013942));
#74295=CARTESIAN_POINT('Ctrl Pts',(-4.31441936658964,-6.88577803085844,
11.9051321614904));
#74296=CARTESIAN_POINT('Ctrl Pts',(-4.39183118215718,-6.83604464803528,
11.9015263215866));
#74297=CARTESIAN_POINT('Ctrl Pts',(-4.56834826307476,-6.72264088020296,
11.893304161579));
#74298=CARTESIAN_POINT('Ctrl Pts',(-4.74049973721233,-6.60237783486906,
11.8850820015714));
#74299=CARTESIAN_POINT('Ctrl Pts',(-4.90775669096825,-6.47561671385486,
11.8768598415638));
#74300=CARTESIAN_POINT('Ctrl Pts',(-5.07498281437133,-6.34887895862604,
11.868639197141));
#74301=CARTESIAN_POINT('Ctrl Pts',(-5.23731598296318,-6.21564569651201,
11.8604185527182));
#74302=CARTESIAN_POINT('Ctrl Pts',(-5.39425835660122,-6.07631996727771,
11.8521979082954));
#74303=CARTESIAN_POINT('Ctrl Pts',(-5.55118309882289,-5.93700989034871,
11.8439781874066));
#74304=CARTESIAN_POINT('Ctrl Pts',(-5.70271803453674,-5.79160890861574,
11.8357584665177));
#74305=CARTESIAN_POINT('Ctrl Pts',(-5.84839973057559,-5.64055920577946,
11.8275387456288));
#74306=CARTESIAN_POINT('Ctrl Pts',(-5.99409309953547,-5.48949739990415,
11.8193183661249));
#74307=CARTESIAN_POINT('Ctrl Pts',(-6.13393208485477,-5.33278617911478,
11.811097986621));
#74308=CARTESIAN_POINT('Ctrl Pts',(-6.26749060693072,-5.17090408483228,
11.8028776071171));
#74309=CARTESIAN_POINT('Ctrl Pts',(-6.40104863474234,-5.00902258963207,
11.7946572580346));
#74310=CARTESIAN_POINT('Ctrl Pts',(-6.52832606003354,-4.84197048857877,
11.7864369089521));
#74311=CARTESIAN_POINT('Ctrl Pts',(-6.64893720971182,-4.67025925873603,
11.7782165598696));
#74312=CARTESIAN_POINT('Ctrl Pts',(-6.76957414766483,-4.49851131473889,
11.7699944531667));
#74313=CARTESIAN_POINT('Ctrl Pts',(-6.8835417927768,-4.32210249333724,11.7617723464638));
#74314=CARTESIAN_POINT('Ctrl Pts',(-6.99049728778659,-4.14157400416173,
11.7535502397609));
#74315=CARTESIAN_POINT('Ctrl Pts',(-7.03740307553505,-4.06240246655126,
11.749944399857));
#74316=CARTESIAN_POINT('Ctrl Pts',(-7.08296078985721,-3.98243895250165,
11.746338559953));
#74317=CARTESIAN_POINT('Ctrl Pts',(-7.12714424291815,-3.90173070612756,
11.7427327200491));
#74318=CARTESIAN_POINT('Ctrl Pts',(-7.22789287026477,-3.71769699046193,
11.7345105600415));
#74319=CARTESIAN_POINT('Ctrl Pts',(-7.32152626643292,-3.5297285961973,11.726288400034));
#74320=CARTESIAN_POINT('Ctrl Pts',(-7.4077527879426,-3.33839575173895,11.7180662400264));
#74321=CARTESIAN_POINT('Ctrl Pts',(-7.49396341538069,-3.14709817552375,
11.7098455956036));
#74322=CARTESIAN_POINT('Ctrl Pts',(-7.57276977191474,-2.95243765582687,
11.7016249511808));
#74323=CARTESIAN_POINT('Ctrl Pts',(-7.64392751697024,-2.75500629360535,
11.693404306758));
#74324=CARTESIAN_POINT('Ctrl Pts',(-7.71507726793335,-2.55759711146489,
11.6851845858691));
#74325=CARTESIAN_POINT('Ctrl Pts',(-7.77858002285569,-2.35741798580953,
11.6769648649802));
#74326=CARTESIAN_POINT('Ctrl Pts',(-7.83424038242487,-2.15507892961798,
11.6687451440913));
#74327=CARTESIAN_POINT('Ctrl Pts',(-7.88990520184711,-1.95272366076694,
11.6605247645874));
#74328=CARTESIAN_POINT('Ctrl Pts',(-7.93772628943084,-1.74820839943263,
11.6523043850835));
#74329=CARTESIAN_POINT('Ctrl Pts',(-7.97755844159658,-1.54215721423307,
11.6440840055796));
#74330=CARTESIAN_POINT('Ctrl Pts',(-8.01739044635451,-1.33610679157212,
11.635863656497));
#74331=CARTESIAN_POINT('Ctrl Pts',(-8.04923352143823,-1.12852074670183,
11.6276433074145));
#74332=CARTESIAN_POINT('Ctrl Pts',(-8.07299370265186,-0.92003273824542,
11.619422958332));
#74333=CARTESIAN_POINT('Ctrl Pts',(-8.09675896410922,-0.711500152271334,
11.6112008516291));
#74334=CARTESIAN_POINT('Ctrl Pts',(-8.11243784560138,-0.502065510735809,
11.6029787449263));
#74335=CARTESIAN_POINT('Ctrl Pts',(-8.11998820555982,-0.292368096873512,
11.5947566382235));
#74336=CARTESIAN_POINT('Ctrl Pts',(-8.12329944806874,-0.200404403140544,
11.5911507983195));
#74337=CARTESIAN_POINT('Ctrl Pts',(-8.12504800743336,-0.10839021155237,
11.5875449584156));
#74338=CARTESIAN_POINT('Ctrl Pts',(-8.12523349038375,-0.0163795374253974,
11.5839391185116));
#74339=CARTESIAN_POINT('Ctrl Pts',(-8.12524449288903,-0.0109216345524287,
11.5837252267631));
#74340=CARTESIAN_POINT('Ctrl Pts',(-8.12524999609811,-0.00546372059166464,
11.5835113350146));
#74341=CARTESIAN_POINT('Ctrl Pts',(-8.12524999999793,-5.80569704969686E-6,
11.5832974432661));
#74342=CARTESIAN_POINT('Origin',(0.,0.,24.4167025567876));
#74343=CARTESIAN_POINT('',(4.94675954817619,6.44587135576159,14.8749382835934));
#74344=CARTESIAN_POINT('',(4.94675954817621,6.44587135576157,14.708345136374));
#74345=CARTESIAN_POINT('',(4.9467595481762,6.44587135576158,24.4167025567876));
#74346=CARTESIAN_POINT('',(-8.12518161405221,1.07740023602867E-5,13.4167025566898));
#74347=CARTESIAN_POINT('Ctrl Pts',(4.94675954817621,6.44587135576157,14.708345136374));
#74348=CARTESIAN_POINT('Ctrl Pts',(5.114411914168,6.31720978365264,14.7000673201305));
#74349=CARTESIAN_POINT('Ctrl Pts',(5.2770488708113,6.18199860132526,14.691789503887));
#74350=CARTESIAN_POINT('Ctrl Pts',(5.43416681847959,6.04065547365808,14.6835116876434));
#74351=CARTESIAN_POINT('Ctrl Pts',(5.59019297142775,5.90029452328386,14.675291393002));
#74352=CARTESIAN_POINT('Ctrl Pts',(5.74077637035415,5.75388679711431,14.6670710983606));
#74353=CARTESIAN_POINT('Ctrl Pts',(5.88545887966758,5.60188016100327,14.6588508037191));
#74354=CARTESIAN_POINT('Ctrl Pts',(6.0316600151547,5.44827802273188,14.6505442266745));
#74355=CARTESIAN_POINT('Ctrl Pts',(6.1718354600305,5.28895898314362,14.6422376496299));
#74356=CARTESIAN_POINT('Ctrl Pts',(6.30555199892502,5.12442206998533,14.6339310725854));
#74357=CARTESIAN_POINT('Ctrl Pts',(6.43926853781952,4.95988515682704,14.6256244955408));
#74358=CARTESIAN_POINT('Ctrl Pts',(6.5665259809629,4.79013061612021,14.6173179184962));
#74359=CARTESIAN_POINT('Ctrl Pts',(6.6869338165474,4.61569103121243,14.6090113414516));
#74360=CARTESIAN_POINT('Ctrl Pts',(6.80611798651609,4.4430242189905,14.600789181444));
#74361=CARTESIAN_POINT('Ctrl Pts',(6.91863046891195,4.2657101715334,14.5925670214365));
#74362=CARTESIAN_POINT('Ctrl Pts',(7.02412238836637,4.08428601297097,14.5843448614289));
#74363=CARTESIAN_POINT('Ctrl Pts',(7.12959486257268,3.90289529619058,14.5761242170061));
#74364=CARTESIAN_POINT('Ctrl Pts',(7.22804920838932,3.71739623541434,14.5679035725832));
#74365=CARTESIAN_POINT('Ctrl Pts',(7.31918134643846,3.52835258731993,14.5596829281604));
#74366=CARTESIAN_POINT('Ctrl Pts',(7.41030324640646,3.33933017700453,14.5514632072715));
#74367=CARTESIAN_POINT('Ctrl Pts',(7.49410445275709,3.14676424012889,14.5432434863826));
#74368=CARTESIAN_POINT('Ctrl Pts',(7.57032772002814,2.95124139539169,14.5350237654938));
#74369=CARTESIAN_POINT('Ctrl Pts',(7.64655709478004,2.7557028841517,14.5268033859899));
#74370=CARTESIAN_POINT('Ctrl Pts',(7.71520720747419,2.55720726565261,14.518583006486));
#74371=CARTESIAN_POINT('Ctrl Pts',(7.77606929191176,2.35636031410456,14.5103626269821));
#74372=CARTESIAN_POINT('Ctrl Pts',(7.83693115111535,2.15551410583629,14.5021422778996));
#74373=CARTESIAN_POINT('Ctrl Pts',(7.89000495667738,1.95231686515983,14.4939219288171));
#74374=CARTESIAN_POINT('Ctrl Pts',(7.93513192012207,1.74738918754804,14.4857015797346));
#74375=CARTESIAN_POINT('Ctrl Pts',(7.9802685323141,1.5424176936625,14.4774794730317));
#74376=CARTESIAN_POINT('Ctrl Pts',(8.01745484434982,1.33571531196892,14.4692573663288));
#74377=CARTESIAN_POINT('Ctrl Pts',(8.04658303441186,1.12791357506469,14.4610352596259));
#74378=CARTESIAN_POINT('Ctrl Pts',(8.05935732619011,1.03678123853476,14.4574294197219));
#74379=CARTESIAN_POINT('Ctrl Pts',(8.070582466931,0.945437573572713,14.453823579818));
#74380=CARTESIAN_POINT('Ctrl Pts',(8.08025249693006,0.853936267150792,14.4502177399141));
#74381=CARTESIAN_POINT('Ctrl Pts',(8.10230243149423,0.645291845227277,14.4419955799065));
#74382=CARTESIAN_POINT('Ctrl Pts',(8.11627041002579,0.435758492998309,14.433773419899));
#74383=CARTESIAN_POINT('Ctrl Pts',(8.12210705167606,0.225974785350209,14.4255512598914));
#74384=CARTESIAN_POINT('Ctrl Pts',(8.12794261746245,0.0162297469791537,
14.4173306154685));
#74385=CARTESIAN_POINT('Ctrl Pts',(8.12564982964777,-0.193765259826035,
14.4091099710457));
#74386=CARTESIAN_POINT('Ctrl Pts',(8.11523138570146,-0.40336970514151,14.4008893266229));
#74387=CARTESIAN_POINT('Ctrl Pts',(8.10481411219706,-0.612950602811235,
14.392669605734));
#74388=CARTESIAN_POINT('Ctrl Pts',(8.08627301967335,-0.822140731925243,
14.3844498848451));
#74389=CARTESIAN_POINT('Ctrl Pts',(8.05966286954378,-1.03030189352312,14.3762301639562));
#74390=CARTESIAN_POINT('Ctrl Pts',(8.03305058724397,-1.23847973428408,14.3680097844523));
#74391=CARTESIAN_POINT('Ctrl Pts',(7.9983679901989,-1.44562814967399,14.3597894049484));
#74392=CARTESIAN_POINT('Ctrl Pts',(7.9557215752874,-1.65111531366121,14.3515690254445));
#74393=CARTESIAN_POINT('Ctrl Pts',(7.91307531819866,-1.85660171719642,14.343348676362));
#74394=CARTESIAN_POINT('Ctrl Pts',(7.86246536478753,-2.06042659318347,14.3351283272795));
#74395=CARTESIAN_POINT('Ctrl Pts',(7.80404918960463,-2.26196901144363,14.326907978197));
#74396=CARTESIAN_POINT('Ctrl Pts',(7.74562052426347,-2.46355452216395,14.3186858714941));
#74397=CARTESIAN_POINT('Ctrl Pts',(7.6793823848452,-2.66285631665436,14.3104637647912));
#74398=CARTESIAN_POINT('Ctrl Pts',(7.6055422336979,-2.859268244488,14.3022416580883));
#74399=CARTESIAN_POINT('Ctrl Pts',(7.57315932100455,-2.94540553175171,14.2986358181844));
#74400=CARTESIAN_POINT('Ctrl Pts',(7.53931495249193,-3.03098723326055,14.2950299782805));
#74401=CARTESIAN_POINT('Ctrl Pts',(7.50402958019213,-3.11596335378026,14.2914241383766));
#74402=CARTESIAN_POINT('Ctrl Pts',(7.42357066223984,-3.30972882267504,14.283201978369));
#74403=CARTESIAN_POINT('Ctrl Pts',(7.33558947662495,-3.50040824237825,14.2749798183615));
#74404=CARTESIAN_POINT('Ctrl Pts',(7.2403481734786,-3.68741723829905,14.2667576583539));
#74405=CARTESIAN_POINT('Ctrl Pts',(7.14512442609186,-3.87439176298871,14.258537013931));
#74406=CARTESIAN_POINT('Ctrl Pts',(7.04264336601514,-4.05769695136209,14.2503163695082));
#74407=CARTESIAN_POINT('Ctrl Pts',(6.93321381006366,-4.23677162783676,14.2420957250853));
#74408=CARTESIAN_POINT('Ctrl Pts',(6.82379654778472,-4.41582618647934,14.2338760041965));
#74409=CARTESIAN_POINT('Ctrl Pts',(6.70743250191391,-4.59065093032095,14.2256562833076));
#74410=CARTESIAN_POINT('Ctrl Pts',(6.58447509278105,-4.76071163956041,14.2174365624187));
#74411=CARTESIAN_POINT('Ctrl Pts',(6.46150783153811,-4.93078597511844,14.2092161829148));
#74412=CARTESIAN_POINT('Ctrl Pts',(6.3319463221571,-5.09609527256796,14.2009958034109));
#74413=CARTESIAN_POINT('Ctrl Pts',(6.19618636624322,-5.25613566009114,14.192775423907));
#74414=CARTESIAN_POINT('Ctrl Pts',(6.06042691274,-5.41617545534837,14.1845550748245));
#74415=CARTESIAN_POINT('Ctrl Pts',(5.91846925155094,-5.5709461563389,14.176334725742));
#74416=CARTESIAN_POINT('Ctrl Pts',(5.77074873622009,-5.71997784837619,14.1681143766595));
#74417=CARTESIAN_POINT('Ctrl Pts',(5.62299663627054,-5.86904140537926,14.1598922699565));
#74418=CARTESIAN_POINT('Ctrl Pts',(5.46947942834891,-6.01236329230735,14.1516701632536));
#74419=CARTESIAN_POINT('Ctrl Pts',(5.31066929053358,-6.14951048857416,14.1434480565507));
#74420=CARTESIAN_POINT('Ctrl Pts',(5.24102242838857,-6.20965697546328,14.1398422166468));
#74421=CARTESIAN_POINT('Ctrl Pts',(5.17035803189016,-6.26861638506664,14.1362363767429));
#74422=CARTESIAN_POINT('Ctrl Pts',(5.09871797967465,-6.32635460010285,14.132630536839));
#74423=CARTESIAN_POINT('Ctrl Pts',(4.93536187181506,-6.45801126130546,14.1244083768314));
#74424=CARTESIAN_POINT('Ctrl Pts',(4.7668767188342,-6.58335911069089,14.1161862168239));
#74425=CARTESIAN_POINT('Ctrl Pts',(4.5937723033958,-6.7020104138276,14.1079640568163));
#74426=CARTESIAN_POINT('Ctrl Pts',(4.42069979616723,-6.8206398460567,14.0997434123934));
#74427=CARTESIAN_POINT('Ctrl Pts',(4.24300996921065,-6.93257502888713,14.0915227679706));
#74428=CARTESIAN_POINT('Ctrl Pts',(4.0612424853508,-7.0374709262406,14.0833021235477));
#74429=CARTESIAN_POINT('Ctrl Pts',(3.87949542184197,-7.14235503924738,14.0750824026589));
#74430=CARTESIAN_POINT('Ctrl Pts',(3.69367187151863,-7.24020129812285,14.06686268177));
#74431=CARTESIAN_POINT('Ctrl Pts',(3.50433776829408,-7.33070967698269,14.0586429608811));
#74432=CARTESIAN_POINT('Ctrl Pts',(3.31498849444716,-7.42122530793507,14.0504225813772));
#74433=CARTESIAN_POINT('Ctrl Pts',(3.12212837077274,-7.50440175431621,14.0422022018733));
#74434=CARTESIAN_POINT('Ctrl Pts',(2.92634602793832,-7.57998591603372,14.0339818223694));
#74435=CARTESIAN_POINT('Ctrl Pts',(2.73056440964105,-7.65556979803483,14.0257614732869));
#74436=CARTESIAN_POINT('Ctrl Pts',(2.53186087011539,-7.72356134776954,14.0175411242044));
#74437=CARTESIAN_POINT('Ctrl Pts',(2.3308425255473,-7.7837562065882,14.0093207751219));
#74438=CARTESIAN_POINT('Ctrl Pts',(2.12978120057295,-7.84396393587145,14.001098668419));
#74439=CARTESIAN_POINT('Ctrl Pts',(1.92640436456651,-7.89637155914005,13.9928765617161));
#74440=CARTESIAN_POINT('Ctrl Pts',(1.72133381909578,-7.94082473334711,13.9846544550132));
#74441=CARTESIAN_POINT('Ctrl Pts',(1.63139925819907,-7.96031986217509,13.9810486151093));
#74442=CARTESIAN_POINT('Ctrl Pts',(1.54113910590134,-7.9782857693441,13.9774427752054));
#74443=CARTESIAN_POINT('Ctrl Pts',(1.45060645962889,-7.99471253152876,13.9738369353015));
#74444=CARTESIAN_POINT('Ctrl Pts',(1.24417080984958,-8.03216939891287,13.9656147752939));
#74445=CARTESIAN_POINT('Ctrl Pts',(1.03624952957575,-8.06163244915906,13.9573926152864));
#74446=CARTESIAN_POINT('Ctrl Pts',(0.827475775738013,-8.08300509730551,
13.9491704552788));
#74447=CARTESIAN_POINT('Ctrl Pts',(0.618740505013095,-8.1043738058474,13.940949810856));
#74448=CARTESIAN_POINT('Ctrl Pts',(0.40915336780636,-8.11765505867199,13.9327291664331));
#74449=CARTESIAN_POINT('Ctrl Pts',(0.199353331470842,-8.12280406089741,
13.9245085220103));
#74450=CARTESIAN_POINT('Ctrl Pts',(-0.0104231352455265,-8.12795248466715,
13.9162888011214));
#74451=CARTESIAN_POINT('Ctrl Pts',(-0.22041215840231,-8.12497047454427,
13.9080690802325));
#74452=CARTESIAN_POINT('Ctrl Pts',(-0.429973235496852,-8.1138653291299,
13.8998493593436));
#74453=CARTESIAN_POINT('Ctrl Pts',(-0.639551103924294,-8.10275929390243,
13.8916289798397));
#74454=CARTESIAN_POINT('Ctrl Pts',(-0.848700662891006,-8.08352883576082,
13.8834086003358));
#74455=CARTESIAN_POINT('Ctrl Pts',(-1.05678392993916,-8.05623331886077,
13.8751882208319));
#74456=CARTESIAN_POINT('Ctrl Pts',(-1.26486642692787,-8.02893790297398,
13.8669678717494));
#74457=CARTESIAN_POINT('Ctrl Pts',(-1.4718823476019,-7.99357752906663,13.8587475226669));
#74458=CARTESIAN_POINT('Ctrl Pts',(-1.67720079620484,-7.95026320644228,
13.8505271735844));
#74459=CARTESIAN_POINT('Ctrl Pts',(-1.88256314463373,-7.90693962263736,
13.8423050668815));
#74460=CARTESIAN_POINT('Ctrl Pts',(-2.08622700705732,-7.85565875346183,
13.8340829601786));
#74461=CARTESIAN_POINT('Ctrl Pts',(-2.28757252101541,-7.79658255414481,
13.8258608534757));
#74462=CARTESIAN_POINT('Ctrl Pts',(-2.3758734534811,-7.77067443539076,13.8222550135718));
#74463=CARTESIAN_POINT('Ctrl Pts',(-2.46372867229529,-7.74326769460846,
13.8186491736679));
#74464=CARTESIAN_POINT('Ctrl Pts',(-2.55108680360823,-7.7143790212146,13.815043333764));
#74465=CARTESIAN_POINT('Ctrl Pts',(-2.75028381533406,-7.64850607583112,
13.8068211737565));
#74466=CARTESIAN_POINT('Ctrl Pts',(-2.94696092416245,-7.57490278118075,
13.7985990137489));
#74467=CARTESIAN_POINT('Ctrl Pts',(-3.14051592933454,-7.49378724411736,
13.7903768537413));
#74468=CARTESIAN_POINT('Ctrl Pts',(-3.33403525665469,-7.41268665902133,
13.7821562093185));
#74469=CARTESIAN_POINT('Ctrl Pts',(-3.52443335685868,-7.32407670925368,
13.7739355648956));
#74470=CARTESIAN_POINT('Ctrl Pts',(-3.71112770477992,-7.22822375977078,
13.7657149204728));
#74471=CARTESIAN_POINT('Ctrl Pts',(-3.89780107885027,-7.13238157872032,
13.7574951995839));
#74472=CARTESIAN_POINT('Ctrl Pts',(-4.08077126887934,-7.02929815720436,
13.749275478695));
#74473=CARTESIAN_POINT('Ctrl Pts',(-4.25947932467885,-6.91928633929348,
13.7410557578061));
#74474=CARTESIAN_POINT('Ctrl Pts',(-4.43820169967596,-6.80926570655357,
13.7328353783022));
#74475=CARTESIAN_POINT('Ctrl Pts',(-4.61266100529772,-6.69231572058388,
13.7246149987983));
#74476=CARTESIAN_POINT('Ctrl Pts',(-4.78232541394498,-6.56879373992181,
13.7163946192944));
#74477=CARTESIAN_POINT('Ctrl Pts',(-4.95198919471046,-6.44527221638096,
13.7081742702119));
#74478=CARTESIAN_POINT('Ctrl Pts',(-5.11685787696167,-6.31517892267167,
13.6999539211294));
#74479=CARTESIAN_POINT('Ctrl Pts',(-5.27643056465477,-6.17891317780699,
13.6917335720469));
#74480=CARTESIAN_POINT('Ctrl Pts',(-5.43603737111922,-6.04261829750657,
13.683511465344));
#74481=CARTESIAN_POINT('Ctrl Pts',(-5.59034569631145,-5.90014852114324,
13.6752893586411));
#74482=CARTESIAN_POINT('Ctrl Pts',(-5.73888870682318,-5.75194262603491,
13.6670672519382));
#74483=CARTESIAN_POINT('Ctrl Pts',(-5.80403287657228,-5.68694629968139,
13.6634614120343));
#74484=CARTESIAN_POINT('Ctrl Pts',(-5.86806866921949,-5.62084723634984,
13.6598555721304));
#74485=CARTESIAN_POINT('Ctrl Pts',(-5.93095895674066,-5.55368467019489,
13.6562497322265));
#74486=CARTESIAN_POINT('Ctrl Pts',(-6.07436355059454,-5.40053827984976,
13.6480275722189));
#74487=CARTESIAN_POINT('Ctrl Pts',(-6.21185692826895,-5.24180926165742,
13.6398054122113));
#74488=CARTESIAN_POINT('Ctrl Pts',(-6.34301463012504,-5.07797725128025,
13.6315832522037));
#74489=CARTESIAN_POINT('Ctrl Pts',(-6.47414815577779,-4.91417543993784,
13.6233626077809));
#74490=CARTESIAN_POINT('Ctrl Pts',(-6.59894815212011,-4.74527274406864,
13.6151419633581));
#74491=CARTESIAN_POINT('Ctrl Pts',(-6.71703052524307,-4.57178176266681,
13.6069213189352));
#74492=CARTESIAN_POINT('Ctrl Pts',(-6.83509963260764,-4.39831027180688,
13.5987015980464));
#74493=CARTESIAN_POINT('Ctrl Pts',(-6.94645245741672,-4.22025176839447,
13.5904818771575));
#74494=CARTESIAN_POINT('Ctrl Pts',(-7.05074784452481,-4.03814838699976,
13.5822621562686));
#74495=CARTESIAN_POINT('Ctrl Pts',(-7.1550515884264,-3.8560304143523,13.5740417767647));
#74496=CARTESIAN_POINT('Ctrl Pts',(-7.25229661567336,-3.66986717090157,
13.5658213972608));
#74497=CARTESIAN_POINT('Ctrl Pts',(-7.34218688518948,-3.48022690430547,
13.5576010177569));
#74498=CARTESIAN_POINT('Ctrl Pts',(-7.43207682204622,-3.2905873395163,13.5493806686744));
#74499=CARTESIAN_POINT('Ctrl Pts',(-7.51461193161352,-3.09747104516457,
13.5411603195919));
#74500=CARTESIAN_POINT('Ctrl Pts',(-7.58954340973417,-2.9014683169493,13.5329399705094));
#74501=CARTESIAN_POINT('Ctrl Pts',(-7.66449090920535,-2.70542368073367,
13.5247178638065));
#74502=CARTESIAN_POINT('Ctrl Pts',(-7.7318314238663,-2.50649165343321,13.5164957571036));
#74503=CARTESIAN_POINT('Ctrl Pts',(-7.79136493885135,-2.30528088356667,
13.5082736504007));
#74504=CARTESIAN_POINT('Ctrl Pts',(-7.81747361533904,-2.21703904369537,
13.5046678104968));
#74505=CARTESIAN_POINT('Ctrl Pts',(-7.84208141545661,-2.12835914131216,
13.5010619705928));
#74506=CARTESIAN_POINT('Ctrl Pts',(-7.86517450686973,-2.03929339208129,
13.4974561306889));
#74507=CARTESIAN_POINT('Ctrl Pts',(-7.91844463505754,-1.83384043674525,
13.4891383376975));
#74508=CARTESIAN_POINT('Ctrl Pts',(-7.96366713914132,-1.6262728969258,13.4808205447061));
#74509=CARTESIAN_POINT('Ctrl Pts',(-8.000696703205,-1.41722963059086,13.4725027517147));
#74510=CARTESIAN_POINT('Ctrl Pts',(-8.03771839720457,-1.2082307931858,13.4641867265422));
#74511=CARTESIAN_POINT('Ctrl Pts',(-8.06655057873264,-0.997757131489211,
13.4558707013697));
#74512=CARTESIAN_POINT('Ctrl Pts',(-8.08709916325463,-0.786457046625093,
13.4475546761972));
#74513=CARTESIAN_POINT('Ctrl Pts',(-8.10764404340868,-0.575195053594521,
13.4392401501847));
#74514=CARTESIAN_POINT('Ctrl Pts',(-8.11990828074441,-0.363107213867596,
13.4309256241723));
#74515=CARTESIAN_POINT('Ctrl Pts',(-8.12384961901664,-0.15084737353743,
13.4226110981598));
#74516=CARTESIAN_POINT('Ctrl Pts',(-8.12478322846949,-0.100568057299159,
13.4206415843691));
#74517=CARTESIAN_POINT('Ctrl Pts',(-8.12525006666185,-0.0502791050878931,
13.4186720705783));
#74518=CARTESIAN_POINT('Ctrl Pts',(-8.12524999999286,1.07715953333801E-5,
13.4167025567876));
#74519=CARTESIAN_POINT('Ctrl Pts',(-8.12455564661523,1.07960349659537E-5,
13.4167025557943));
#74520=CARTESIAN_POINT('Ctrl Pts',(-8.12458628377602,0.664182828634124,
13.39068921358));
#74521=CARTESIAN_POINT('Ctrl Pts',(-7.88026825892223,2.67977085846249,13.3117446708532));
#74522=CARTESIAN_POINT('Ctrl Pts',(-6.23176414069403,5.73643646235047,13.1798689276139));
#74523=CARTESIAN_POINT('Ctrl Pts',(-2.72779796832367,8.01877209027872,13.0210753260764));
#74524=CARTESIAN_POINT('Ctrl Pts',(1.39851398942074,8.34320643186221,12.8639024043266));
#74525=CARTESIAN_POINT('Ctrl Pts',(3.90815072701549,7.2432900977911,12.7596606830893));
#74526=CARTESIAN_POINT('Ctrl Pts',(4.94717300284021,6.44641043468649,12.7083501623644));
#74527=CARTESIAN_POINT('',(-8.12524999926494,-0.000109293386091071,13.5832974432338));
#74528=CARTESIAN_POINT('Ctrl Pts',(-8.12524999926495,-0.000109292839731289,
13.5832974432124));
#74529=CARTESIAN_POINT('Ctrl Pts',(-8.12525283523286,0.210727467548692,
13.5750400395771));
#74530=CARTESIAN_POINT('Ctrl Pts',(-8.11704503066721,0.421561740255473,
13.5667826359418));
#74531=CARTESIAN_POINT('Ctrl Pts',(-8.1006532199022,0.631747555110545,13.5585252323065));
#74532=CARTESIAN_POINT('Ctrl Pts',(-8.08426130399346,0.841934718182757,
13.5502677757049));
#74533=CARTESIAN_POINT('Ctrl Pts',(-8.05968530261826,1.05147312662298,13.5420103191033));
#74534=CARTESIAN_POINT('Ctrl Pts',(-8.02700379967336,1.25972122413236,13.5337528625017));
#74535=CARTESIAN_POINT('Ctrl Pts',(-7.9943137565393,1.46802374013491,13.5254932480971));
#74536=CARTESIAN_POINT('Ctrl Pts',(-7.95351402346721,1.67503498511879,13.5172336336926));
#74537=CARTESIAN_POINT('Ctrl Pts',(-7.90473466922945,1.88012163744318,13.5089740192881));
#74538=CARTESIAN_POINT('Ctrl Pts',(-7.86632418913691,2.04161366413042,13.5024701251793));
#74539=CARTESIAN_POINT('Ctrl Pts',(-7.82296696247514,2.20191247086353,13.4959662310706));
#74540=CARTESIAN_POINT('Ctrl Pts',(-7.77474855855956,2.36071438629835,13.4894623369618));
#74541=CARTESIAN_POINT('Ctrl Pts',(-7.7137913188393,2.56147023139319,13.4812401769542));
#74542=CARTESIAN_POINT('Ctrl Pts',(-7.64504413156814,2.75989692910004,13.4730180169467));
#74543=CARTESIAN_POINT('Ctrl Pts',(-7.56871023699752,2.95538710000382,13.4647958569391));
#74544=CARTESIAN_POINT('Ctrl Pts',(-7.49239041299751,3.15084123634824,13.4565752125162));
#74545=CARTESIAN_POINT('Ctrl Pts',(-7.40848678011347,3.34335965143663,13.4483545680934));
#74546=CARTESIAN_POINT('Ctrl Pts',(-7.31725130570271,3.53235344942885,13.4401339236705));
#74547=CARTESIAN_POINT('Ctrl Pts',(-7.22602608098177,3.72132601524338,13.4319142027816));
#74548=CARTESIAN_POINT('Ctrl Pts',(-7.12747078741842,3.9067744887932,13.4236944818926));
#74549=CARTESIAN_POINT('Ctrl Pts',(-7.02188443686295,4.08813239974464,13.4154747610037));
#74550=CARTESIAN_POINT('Ctrl Pts',(-6.91628962607497,4.26950484221541,13.4072543814998));
#74551=CARTESIAN_POINT('Ctrl Pts',(-6.80366277876538,4.44678581074138,13.3990340019959));
#74552=CARTESIAN_POINT('Ctrl Pts',(-6.68434807441564,4.61943485532115,13.390813622492));
#74553=CARTESIAN_POINT('Ctrl Pts',(-6.5650338116171,4.79208326097386,13.3825932734095));
#74554=CARTESIAN_POINT('Ctrl Pts',(-6.43903191128112,4.9600995356832,13.374372924327));
#74555=CARTESIAN_POINT('Ctrl Pts',(-6.3067292609164,5.12297312036682,13.3661525752444));
#74556=CARTESIAN_POINT('Ctrl Pts',(-6.17439832247844,5.28588152959763,13.3579304685415));
#74557=CARTESIAN_POINT('Ctrl Pts',(-6.03576412872503,5.44364482293004,13.3497083618386));
#74558=CARTESIAN_POINT('Ctrl Pts',(-5.89125385073188,5.59578552383281,13.3414862551357));
#74559=CARTESIAN_POINT('Ctrl Pts',(-5.82787825300201,5.66250747601956,13.3378804152319));
#74560=CARTESIAN_POINT('Ctrl Pts',(-5.76337301003238,5.728148488673,13.3342745753281));
#74561=CARTESIAN_POINT('Ctrl Pts',(-5.69777643160394,5.79267048069875,13.3306687354243));
#74562=CARTESIAN_POINT('Ctrl Pts',(-5.5482008602592,5.93979574321652,13.3224465754167));
#74563=CARTESIAN_POINT('Ctrl Pts',(-5.39289906328124,6.08114878342411,13.3142244154092));
#74564=CARTESIAN_POINT('Ctrl Pts',(-5.23234009919822,6.21629348155493,13.3060022554016));
#74565=CARTESIAN_POINT('Ctrl Pts',(-5.07181073083084,6.35141326856304,13.2977816109787));
#74566=CARTESIAN_POINT('Ctrl Pts',(-4.90602635513595,6.48032680755237,13.2895609665559));
#74567=CARTESIAN_POINT('Ctrl Pts',(-4.73548997611329,6.60263752212936,13.281340322133));
#74568=CARTESIAN_POINT('Ctrl Pts',(-4.56497275570302,6.72493449592221,13.2731206012441));
#74569=CARTESIAN_POINT('Ctrl Pts',(-4.38970483751106,6.84062995427466,13.2649008803552));
#74570=CARTESIAN_POINT('Ctrl Pts',(-4.21021980752773,6.94936952066885,13.2566811594664));
#74571=CARTESIAN_POINT('Ctrl Pts',(-4.03072039609063,7.0581177999515,13.2484607799625));
#74572=CARTESIAN_POINT('Ctrl Pts',(-3.84700344872614,7.15990891836325,13.2402404004585));
#74573=CARTESIAN_POINT('Ctrl Pts',(-3.65962976542472,7.25443295802762,13.2320200209546));
#74574=CARTESIAN_POINT('Ctrl Pts',(-3.47225677554188,7.34895664788447,13.2237996718721));
#74575=CARTESIAN_POINT('Ctrl Pts',(-3.28122734150666,7.43621318224071,13.2155793227896));
#74576=CARTESIAN_POINT('Ctrl Pts',(-3.08712546566586,7.51593932397923,13.207358973707));
#74577=CARTESIAN_POINT('Ctrl Pts',(-2.89298208825296,7.5956825122311,13.1991368670041));
#74578=CARTESIAN_POINT('Ctrl Pts',(-2.69576522968438,7.66789197904101,13.1909147603012));
#74579=CARTESIAN_POINT('Ctrl Pts',(-2.49607843871186,7.73235281077485,13.1826926535983));
#74580=CARTESIAN_POINT('Ctrl Pts',(-2.40850494627522,7.76062238300249,13.1790868136945));
#74581=CARTESIAN_POINT('Ctrl Pts',(-2.32045663554736,7.78740229881576,13.1754809737906));
#74582=CARTESIAN_POINT('Ctrl Pts',(-2.23198536645222,7.81267744671717,13.1718751338868));
#74583=CARTESIAN_POINT('Ctrl Pts',(-2.03025013971722,7.87031070715078,13.1636529738792));
#74584=CARTESIAN_POINT('Ctrl Pts',(-1.82624816262755,7.92013563528932,13.1554308138716));
#74585=CARTESIAN_POINT('Ctrl Pts',(-1.62059998012985,7.96199367413107,13.1472086538641));
#74586=CARTESIAN_POINT('Ctrl Pts',(-1.41498970461059,8.00384399731126,13.1389880094412));
#74587=CARTESIAN_POINT('Ctrl Pts',(-1.20773411838256,8.03773030334217,13.1307673650184));
#74588=CARTESIAN_POINT('Ctrl Pts',(-0.999464656104813,8.06354499979366,
13.1225467205955));
#74589=CARTESIAN_POINT('Ctrl Pts',(-0.791218591497348,8.089356796138,13.1143269997066));
#74590=CARTESIAN_POINT('Ctrl Pts',(-0.581959171024286,8.10709875695665,
13.1061072788178));
#74591=CARTESIAN_POINT('Ctrl Pts',(-0.372324494548209,8.11671497794886,
13.0978875579289));
#74592=CARTESIAN_POINT('Ctrl Pts',(-0.162673020841052,8.12633196945237,
13.089667178425));
#74593=CARTESIAN_POINT('Ctrl Pts',(0.0473534742294832,8.12782190394492,
13.0814467989211));
#74594=CARTESIAN_POINT('Ctrl Pts',(0.25711426377705,8.12118093739219,13.0732264194172));
#74595=CARTESIAN_POINT('Ctrl Pts',(0.466874277057171,8.11453999541588,13.0650060703347));
#74596=CARTESIAN_POINT('Ctrl Pts',(0.676368291869704,8.0997682245935,13.0567857212522));
#74597=CARTESIAN_POINT('Ctrl Pts',(0.88495754015993,8.0769138731705,13.0485653721696));
#74598=CARTESIAN_POINT('Ctrl Pts',(1.09359138761617,8.05405463518205,13.0403432654667));
#74599=CARTESIAN_POINT('Ctrl Pts',(1.30131978862463,8.02310939620984,13.0321211587638));
#74600=CARTESIAN_POINT('Ctrl Pts',(1.50750993027571,7.98417819018464,13.0238990520609));
#74601=CARTESIAN_POINT('Ctrl Pts',(1.5979354948449,7.96710474401501,13.020293212157));
#74602=CARTESIAN_POINT('Ctrl Pts',(1.68806531497049,7.94849602462319,13.0166873722531));
#74603=CARTESIAN_POINT('Ctrl Pts',(1.777846621314,7.92836357349878,13.0130815323492));
#74604=CARTESIAN_POINT('Ctrl Pts',(1.98256750933193,7.88245721013628,13.0048594338162));
#74605=CARTESIAN_POINT('Ctrl Pts',(2.18554318373643,7.82860978502314,12.9966373352832));
#74606=CARTESIAN_POINT('Ctrl Pts',(2.38615288333715,7.7669789480751,12.9884152367502));
#74607=CARTESIAN_POINT('Ctrl Pts',(2.58672500987442,7.70535965423466,12.9801946781698));
#74608=CARTESIAN_POINT('Ctrl Pts',(2.78493176410168,7.63595994484411,12.9719741195894));
#74609=CARTESIAN_POINT('Ctrl Pts',(2.98016721010928,7.55898742969516,12.963753561009));
#74610=CARTESIAN_POINT('Ctrl Pts',(3.17539843895926,7.48201657718093,12.9555331799957));
#74611=CARTESIAN_POINT('Ctrl Pts',(3.36765821197506,7.39747335061567,12.9473127989824));
#74612=CARTESIAN_POINT('Ctrl Pts',(3.55635930970939,7.3056140072374,12.9390924179691));
#74613=CARTESIAN_POINT('Ctrl Pts',(3.7450472715417,7.21376105839181,12.9308726091948));
#74614=CARTESIAN_POINT('Ctrl Pts',(3.93017678811928,7.114593140326,12.9226528004204));
#74615=CARTESIAN_POINT('Ctrl Pts',(4.11118349949156,7.0084133579583,12.9144329916461));
#74616=CARTESIAN_POINT('Ctrl Pts',(4.29221574062193,6.90221859965883,12.9062120235239));
#74617=CARTESIAN_POINT('Ctrl Pts',(4.46912375957649,6.78901014955914,12.8979910554018));
#74618=CARTESIAN_POINT('Ctrl Pts',(4.64136960010035,6.66913606082259,12.8897700872797));
#74619=CARTESIAN_POINT('Ctrl Pts',(4.74488681134554,6.59709350044014,12.8848294066156));
#74620=CARTESIAN_POINT('Ctrl Pts',(4.84672065219238,6.52264427544677,12.8798887259516));
#74621=CARTESIAN_POINT('Ctrl Pts',(4.94675954817619,6.44587135576158,12.8749480452876));
#74622=CARTESIAN_POINT('Ctrl Pts',(4.94675954817619,6.44587135576159,14.8749382835934));
#74623=CARTESIAN_POINT('Ctrl Pts',(5.11322618946787,6.31811974518586,14.8667184029981));
#74624=CARTESIAN_POINT('Ctrl Pts',(5.27475363759568,6.18390667886123,14.8584985224029));
#74625=CARTESIAN_POINT('Ctrl Pts',(5.4308477106004,6.04363969034938,14.8502786418076));
#74626=CARTESIAN_POINT('Ctrl Pts',(5.58695298024303,5.90336264047741,14.8420581715998));
#74627=CARTESIAN_POINT('Ctrl Pts',(5.73762387428406,5.75703099557787,14.833837701392));
#74628=CARTESIAN_POINT('Ctrl Pts',(5.88240082059063,5.6050912703019,14.8256172311841));
#74629=CARTESIAN_POINT('Ctrl Pts',(6.02717483279472,5.45315462429192,14.8173969275754));
#74630=CARTESIAN_POINT('Ctrl Pts',(6.16605493402484,5.29561034031495,14.8091766239666));
#74631=CARTESIAN_POINT('Ctrl Pts',(6.29861946790666,5.13294071278904,14.8009563203578));
#74632=CARTESIAN_POINT('Ctrl Pts',(6.43121433767825,4.97023386016418,14.7927341356258));
#74633=CARTESIAN_POINT('Ctrl Pts',(6.55749056529819,4.80239954892059,14.7845119508938));
#74634=CARTESIAN_POINT('Ctrl Pts',(6.67706701070395,4.62995288281307,14.7762897661618));
#74635=CARTESIAN_POINT('Ctrl Pts',(6.75695066281212,4.51474901104883,14.7707968938619));
#74636=CARTESIAN_POINT('Ctrl Pts',(6.8338450645536,4.39748732251782,14.7653040215619));
#74637=CARTESIAN_POINT('Ctrl Pts',(6.907647309015,4.27832867095993,14.7598111492619));
#74638=CARTESIAN_POINT('Ctrl Pts',(7.01812026919681,4.09996270031851,14.7515889892543));
#74639=CARTESIAN_POINT('Ctrl Pts',(7.1216992449118,3.9172861393959,14.7433668292467));
#74640=CARTESIAN_POINT('Ctrl Pts',(7.21806243230082,3.73085275585992,14.7351446692391));
#74641=CARTESIAN_POINT('Ctrl Pts',(7.31440785713417,3.54445373745283,14.7269240248163));
#74642=CARTESIAN_POINT('Ctrl Pts',(7.40354001284765,3.35429954060967,14.7187033803934));
#74643=CARTESIAN_POINT('Ctrl Pts',(7.48518315744339,3.16096831082278,14.7104827359706));
#74644=CARTESIAN_POINT('Ctrl Pts',(7.56681712998245,2.96765880049569,14.7022630150817));
#74645=CARTESIAN_POINT('Ctrl Pts',(7.64096365630516,2.77117324157322,14.6940432941928));
#74646=CARTESIAN_POINT('Ctrl Pts',(7.70739490466815,2.5721102904027,14.6858235733039));
#74647=CARTESIAN_POINT('Ctrl Pts',(7.77383147591471,2.37303138907409,14.6776031938));
#74648=CARTESIAN_POINT('Ctrl Pts',(7.83255143796145,2.17137496196681,14.6693828142961));
#74649=CARTESIAN_POINT('Ctrl Pts',(7.88337632879413,1.96775639272456,14.6611624347922));
#74650=CARTESIAN_POINT('Ctrl Pts',(7.93420103153772,1.76413857701921,14.6529420857097));
#74651=CARTESIAN_POINT('Ctrl Pts',(7.9771306526257,1.55855892070873,14.6447217366271));
#74652=CARTESIAN_POINT('Ctrl Pts',(8.01203738140362,1.35164513149385,14.6365013875446));
#74653=CARTESIAN_POINT('Ctrl Pts',(8.04695157370626,1.14468710134794,14.6282792808417));
#74654=CARTESIAN_POINT('Ctrl Pts',(8.07383939755248,0.936394659503291,14.6200571741388));
#74655=CARTESIAN_POINT('Ctrl Pts',(8.0926244887072,0.727403909307994,14.6118350674359));
#74656=CARTESIAN_POINT('Ctrl Pts',(8.10086277041895,0.635750125939142,14.6082292275321));
#74657=CARTESIAN_POINT('Ctrl Pts',(8.10754332577607,0.543962114232721,14.6046233876282));
#74658=CARTESIAN_POINT('Ctrl Pts',(8.11266286535577,0.452093790686792,14.6010175477244));
#74659=CARTESIAN_POINT('Ctrl Pts',(8.12433661535909,0.242612483704973,14.5927953877168));
#74660=CARTESIAN_POINT('Ctrl Pts',(8.12789426530707,0.0326442164661224,
14.5845732277093));
#74661=CARTESIAN_POINT('Ctrl Pts',(8.12331816930504,-0.17717077281155,14.5763510677017));
#74662=CARTESIAN_POINT('Ctrl Pts',(8.11874291681143,-0.386947087046077,
14.5681304232789));
#74663=CARTESIAN_POINT('Ctrl Pts',(8.10603691717088,-0.59656988478547,14.5599097788561));
#74664=CARTESIAN_POINT('Ctrl Pts',(8.08523463567595,-0.805399558334893,
14.5516891344332));
#74665=CARTESIAN_POINT('Ctrl Pts',(8.06443469117703,-1.01420577127899,14.5434694135444));
#74666=CARTESIAN_POINT('Ctrl Pts',(8.03554030994549,-1.22221874434522,14.5352496926555));
#74667=CARTESIAN_POINT('Ctrl Pts',(7.99863784151324,-1.42880378037446,14.5270299717666));
#74668=CARTESIAN_POINT('Ctrl Pts',(7.96173241622641,-1.63540536927775,14.5188095922627));
#74669=CARTESIAN_POINT('Ctrl Pts',(7.91681767085712,-1.8405785014969,14.5105892127588));
#74670=CARTESIAN_POINT('Ctrl Pts',(7.86403131061546,-2.04369741110557,14.502368833255));
#74671=CARTESIAN_POINT('Ctrl Pts',(7.81124514572172,-2.24681556902657,14.4941484841725));
#74672=CARTESIAN_POINT('Ctrl Pts',(7.75058750104723,-2.44787923456029,14.4859281350899));
#74673=CARTESIAN_POINT('Ctrl Pts',(7.68224645627633,-2.64627605278243,14.4777077860074));
#74674=CARTESIAN_POINT('Ctrl Pts',(7.61389079927753,-2.8447152908934,14.4694856793046));
#74675=CARTESIAN_POINT('Ctrl Pts',(7.53784855630371,-3.04048626342017,14.4612635726017));
#74676=CARTESIAN_POINT('Ctrl Pts',(7.45435700021095,-3.23299385645968,14.4530414658988));
#74677=CARTESIAN_POINT('Ctrl Pts',(7.4177414227828,-3.31741888107669,14.4494356259948));
#74678=CARTESIAN_POINT('Ctrl Pts',(7.37969374624601,-3.40121651364254,14.4458297860909));
#74679=CARTESIAN_POINT('Ctrl Pts',(7.34023687728884,-3.48433783491053,14.4422239461869));
#74680=CARTESIAN_POINT('Ctrl Pts',(7.25026596937137,-3.67387392683657,14.4340017861793));
#74681=CARTESIAN_POINT('Ctrl Pts',(7.15293512516094,-3.85995465363508,14.4257796261718));
#74682=CARTESIAN_POINT('Ctrl Pts',(7.04853515787065,-4.04200936302248,14.4175574661642));
#74683=CARTESIAN_POINT('Ctrl Pts',(6.9441544345498,-4.22403051439873,14.4093368217414));
#74684=CARTESIAN_POINT('Ctrl Pts',(6.83270733559829,-4.40202687361533,14.4011161773185));
#74685=CARTESIAN_POINT('Ctrl Pts',(6.71453013276911,-4.57545327357144,14.3928955328957));
#74686=CARTESIAN_POINT('Ctrl Pts',(6.59636620635165,-4.74886019024114,14.3846758120068));
#74687=CARTESIAN_POINT('Ctrl Pts',(6.47147385165479,-4.91769792882157,14.3764560911179));
#74688=CARTESIAN_POINT('Ctrl Pts',(6.34023255200054,-5.08145045720734,14.368236370229));
#74689=CARTESIAN_POINT('Ctrl Pts',(6.2089807364795,-5.24521610646116,14.3600159907251));
#74690=CARTESIAN_POINT('Ctrl Pts',(6.07137914198951,-5.40389549935813,14.3517956112212));
#74691=CARTESIAN_POINT('Ctrl Pts',(5.92784807566002,-5.55700501658886,14.3435752317173));
#74692=CARTESIAN_POINT('Ctrl Pts',(5.78431754049983,-5.71011396720306,14.3353548826348));
#74693=CARTESIAN_POINT('Ctrl Pts',(5.63485778119669,-5.85765286988468,14.3271345335523));
#74694=CARTESIAN_POINT('Ctrl Pts',(5.479926923815,-5.99917398248688,14.3189141844698));
#74695=CARTESIAN_POINT('Ctrl Pts',(5.32496294014724,-6.14072535419265,14.3106920777669));
#74696=CARTESIAN_POINT('Ctrl Pts',(5.1645257393401,-6.27625616617983,14.302469971064));
#74697=CARTESIAN_POINT('Ctrl Pts',(4.99910839666797,-6.40535735153503,14.294247864361));
#74698=CARTESIAN_POINT('Ctrl Pts',(4.92656391670038,-6.4619752260789,14.2906420244572));
#74699=CARTESIAN_POINT('Ctrl Pts',(4.85306203549236,-6.51735701344645,14.2870361845533));
#74700=CARTESIAN_POINT('Ctrl Pts',(4.77864627239451,-6.57147071558795,14.2834303446494));
#74701=CARTESIAN_POINT('Ctrl Pts',(4.60896089323568,-6.69486263798879,14.2752081846418));
#74702=CARTESIAN_POINT('Ctrl Pts',(4.43446570784709,-6.81169910659657,14.2669860246343));
#74703=CARTESIAN_POINT('Ctrl Pts',(4.25568910354683,-6.92161815014761,14.2587638646267));
#74704=CARTESIAN_POINT('Ctrl Pts',(4.07694545300695,-7.03151693240194,14.2505432202039));
#74705=CARTESIAN_POINT('Ctrl Pts',(3.8939222099668,-7.13450067998437,14.242322575781));
#74706=CARTESIAN_POINT('Ctrl Pts',(3.70717548723022,-7.23025154952298,14.2341019313582));
#74707=CARTESIAN_POINT('Ctrl Pts',(3.52044974422825,-7.32599166209726,14.2258822104693));
#74708=CARTESIAN_POINT('Ctrl Pts',(3.33000161918168,-7.41450038424945,14.2176624895804));
#74709=CARTESIAN_POINT('Ctrl Pts',(3.13641123107975,-7.49550613047957,14.2094427686915));
#74710=CARTESIAN_POINT('Ctrl Pts',(2.94280533131564,-7.57651836739233,14.2012223891876));
#74711=CARTESIAN_POINT('Ctrl Pts',(2.74605693664309,-7.65002631070526,14.1930020096837));
#74712=CARTESIAN_POINT('Ctrl Pts',(2.54676650728578,-7.71580636873861,14.1847816301798));
#74713=CARTESIAN_POINT('Ctrl Pts',(2.34747681544809,-7.78158618333789,14.1765612810973));
#74714=CARTESIAN_POINT('Ctrl Pts',(2.14564538885169,-7.83963807989123,14.1683409320148));
#74715=CARTESIAN_POINT('Ctrl Pts',(1.9418887328439,-7.88978806507208,14.1601205829323));
#74716=CARTESIAN_POINT('Ctrl Pts',(1.7380885109424,-7.9399487729894,14.1518984762294));
#74717=CARTESIAN_POINT('Ctrl Pts',(1.53236252390231,-7.98220412362127,14.1436763695265));
#74718=CARTESIAN_POINT('Ctrl Pts',(1.32533946353552,-8.01643080609415,14.1354542628236));
#74719=CARTESIAN_POINT('Ctrl Pts',(1.23454861891719,-8.03144106342824,14.1318484229197));
#74720=CARTESIAN_POINT('Ctrl Pts',(1.14350843511523,-8.04490783165832,14.1282425830158));
#74721=CARTESIAN_POINT('Ctrl Pts',(1.05227243640835,-8.05682383337722,14.1246367431119));
#74722=CARTESIAN_POINT('Ctrl Pts',(0.844232978248779,-8.083995109805,14.1164145831043));
#74723=CARTESIAN_POINT('Ctrl Pts',(0.635106222316402,-8.10310871945177,
14.1081924230968));
#74724=CARTESIAN_POINT('Ctrl Pts',(0.425529336930057,-8.11409960167558,
14.0999702630892));
#74725=CARTESIAN_POINT('Ctrl Pts',(0.215991082697217,-8.12508845795814,
14.0917496186663));
#74726=CARTESIAN_POINT('Ctrl Pts',(0.00600315920071098,-8.12795755968557,
14.0835289742435));
#74727=CARTESIAN_POINT('Ctrl Pts',(-0.203794030827732,-8.12269386075205,
14.0753083298207));
#74728=CARTESIAN_POINT('Ctrl Pts',(-0.413567651556558,-8.1174307531596,
14.0670886089318));
#74729=CARTESIAN_POINT('Ctrl Pts',(-0.623150286661849,-8.10403667637436,
14.0588688880429));
#74730=CARTESIAN_POINT('Ctrl Pts',(-0.831902584058519,-8.08255068979692,
14.050649167154));
#74731=CARTESIAN_POINT('Ctrl Pts',(-1.04067160798393,-8.06106298162899,
14.0424287876501));
#74732=CARTESIAN_POINT('Ctrl Pts',(-1.24860986738173,-8.03148209565615,
14.0342084081462));
#74733=CARTESIAN_POINT('Ctrl Pts',(-1.45508310963106,-7.99389896774824,
14.0259880286423));
#74734=CARTESIAN_POINT('Ctrl Pts',(-1.66155558777939,-7.95631597892521,
14.0177676795598));
#74735=CARTESIAN_POINT('Ctrl Pts',(-1.86656276972992,-7.91073086288741,
14.0095473304773));
#74736=CARTESIAN_POINT('Ctrl Pts',(-2.06948004250879,-7.85728578557238,
14.0013269813948));
#74737=CARTESIAN_POINT('Ctrl Pts',(-2.27244070170992,-7.80382928098623,
13.9931048746919));
#74738=CARTESIAN_POINT('Ctrl Pts',(-2.47331027355075,-7.74250953286885,
13.984882767989));
#74739=CARTESIAN_POINT('Ctrl Pts',(-2.6714776917589,-7.67351904310757,13.9766606612861));
#74740=CARTESIAN_POINT('Ctrl Pts',(-2.75838485680127,-7.64326297006462,
13.9730548213822));
#74741=CARTESIAN_POINT('Ctrl Pts',(-2.84477252316002,-7.61153222764843,
13.9694489814783));
#74742=CARTESIAN_POINT('Ctrl Pts',(-2.93059020803915,-7.57834603294446,
13.9658431415744));
#74743=CARTESIAN_POINT('Ctrl Pts',(-3.12627464089316,-7.50267373185202,
13.9576209815668));
#74744=CARTESIAN_POINT('Ctrl Pts',(-3.31905883691528,-7.41940558737523,
13.9493988215593));
#74745=CARTESIAN_POINT('Ctrl Pts',(-3.50835215499058,-7.32878930786477,
13.9411766615517));
#74746=CARTESIAN_POINT('Ctrl Pts',(-3.69761058076738,-7.23818973158665,
13.9329560171288));
#74747=CARTESIAN_POINT('Ctrl Pts',(-3.88337914679839,-7.14024485099647,
13.924735372706));
#74748=CARTESIAN_POINT('Ctrl Pts',(-4.06508925700879,-7.03524959721059,
13.9165147282832));
#74749=CARTESIAN_POINT('Ctrl Pts',(-4.24677895331354,-6.9302661389335,13.9082950073943));
#74750=CARTESIAN_POINT('Ctrl Pts',(-4.42441084860086,-6.81823403635945,
13.9000752865054));
#74751=CARTESIAN_POINT('Ctrl Pts',(-4.59744219818209,-6.6994934731571,13.8918555656165));
#74752=CARTESIAN_POINT('Ctrl Pts',(-4.77048741210823,-6.58074339572437,
13.8836351861126));
#74753=CARTESIAN_POINT('Ctrl Pts',(-4.93893109887327,-6.4552839483907,13.8754148066088));
#74754=CARTESIAN_POINT('Ctrl Pts',(-5.10225981096964,-6.32349842918175,
13.8671944271049));
#74755=CARTESIAN_POINT('Ctrl Pts',(-5.26558791863134,-6.19171339767478,
13.8589740780223));
#74756=CARTESIAN_POINT('Ctrl Pts',(-5.42380086146933,-6.05360252853669,
13.8507537289398));
#74757=CARTESIAN_POINT('Ctrl Pts',(-5.57641816675348,-5.90958949437283,
13.8425333798573));
#74758=CARTESIAN_POINT('Ctrl Pts',(-5.72906810365512,-5.76554566829952,
13.8343112731544));
#74759=CARTESIAN_POINT('Ctrl Pts',(-5.87611979807905,-5.61559735864673,
13.8260891664515));
#74760=CARTESIAN_POINT('Ctrl Pts',(-6.01712875518766,-5.46020595820284,
13.8178670597486));
#74761=CARTESIAN_POINT('Ctrl Pts',(-6.07896883373719,-5.39205839788885,
13.8142612198446));
#74762=CARTESIAN_POINT('Ctrl Pts',(-6.1396472022574,-5.32286443495135,13.8106553799407));
#74763=CARTESIAN_POINT('Ctrl Pts',(-6.19912872449189,-5.25266509685127,
13.8070495400368));
#74764=CARTESIAN_POINT('Ctrl Pts',(-6.33476053464949,-5.09259415480571,
13.7988273800293));
#74765=CARTESIAN_POINT('Ctrl Pts',(-6.46421149893803,-4.92724066084432,
13.7906052200217));
#74766=CARTESIAN_POINT('Ctrl Pts',(-6.58708147076001,-4.75710471401147,
13.7823830600141));
#74767=CARTESIAN_POINT('Ctrl Pts',(-6.70992879405006,-4.5870001282131,13.7741624155913));
#74768=CARTESIAN_POINT('Ctrl Pts',(-6.82619737328195,-4.41211508813729,
13.7659417711685));
#74769=CARTESIAN_POINT('Ctrl Pts',(-6.93552901292721,-4.2329806133911,13.7577211267457));
#74770=CARTESIAN_POINT('Ctrl Pts',(-7.0448483699003,-4.05386626319472,13.7495014058568));
#74771=CARTESIAN_POINT('Ctrl Pts',(-7.14723218944189,-3.87050368324245,
13.7412816849679));
#74772=CARTESIAN_POINT('Ctrl Pts',(-7.24236662693766,-3.68345126254165,
13.733061964079));
#74773=CARTESIAN_POINT('Ctrl Pts',(-7.33750868719447,-3.49638385404102,
13.7248415845751));
#74774=CARTESIAN_POINT('Ctrl Pts',(-7.42540006854169,-3.30562627589227,
13.7166212050712));
#74775=CARTESIAN_POINT('Ctrl Pts',(-7.50577328014737,-3.11176076032941,
13.7084008255673));
#74776=CARTESIAN_POINT('Ctrl Pts',(-7.58614619431361,-2.91789596221019,
13.7001804764848));
#74777=CARTESIAN_POINT('Ctrl Pts',(-7.65900088382745,-2.72092352334852,
13.6919601274023));
#74778=CARTESIAN_POINT('Ctrl Pts',(-7.72411813024424,-2.52144535386596,
13.6837397783198));
#74779=CARTESIAN_POINT('Ctrl Pts',(-7.78924929959781,-2.32192453328716,
13.6755176716169));
#74780=CARTESIAN_POINT('Ctrl Pts',(-7.84663962913896,-2.11989719237576,
13.667295564914));
#74781=CARTESIAN_POINT('Ctrl Pts',(-7.8961195399841,-1.91598115146818,13.6590734582111));
#74782=CARTESIAN_POINT('Ctrl Pts',(-7.91781916556865,-1.82655290346206,
13.6554676183072));
#74783=CARTESIAN_POINT('Ctrl Pts',(-7.93799803372971,-1.73676157763822,
13.6518617784032));
#74784=CARTESIAN_POINT('Ctrl Pts',(-7.95664491912623,-1.64666001149077,
13.6482559384993));
#74785=CARTESIAN_POINT('Ctrl Pts',(-8.00016030884298,-1.43639407797839,
13.6398411536524));
#74786=CARTESIAN_POINT('Ctrl Pts',(-8.03534067518961,-1.22438249265304,
13.6314263688055));
#74787=CARTESIAN_POINT('Ctrl Pts',(-8.06207098145817,-1.01128584111026,
13.6230115839586));
#74788=CARTESIAN_POINT('Ctrl Pts',(-8.08879423962124,-0.798245377763173,
13.6145990178776));
#74789=CARTESIAN_POINT('Ctrl Pts',(-8.10707185453581,-0.584120681911771,
13.6061864517965));
#74790=CARTESIAN_POINT('Ctrl Pts',(-8.11684044199827,-0.369579222415569,
13.5977738857155));
#74791=CARTESIAN_POINT('Ctrl Pts',(-8.12244374199678,-0.246517401625759,
13.5929484048883));
#74792=CARTESIAN_POINT('Ctrl Pts',(-8.1252483419671,-0.12331857197614,13.588122924061));
#74793=CARTESIAN_POINT('Ctrl Pts',(-8.12524999926494,-0.000109293386091071,
13.5832974432338));
#74794=CARTESIAN_POINT('Origin',(0.,0.,24.4167025567876));
#74795=CARTESIAN_POINT('',(4.94675954817621,6.44587135576157,16.8749477411846));
#74796=CARTESIAN_POINT('',(4.94678612080823,6.44590587665303,16.7083566551695));
#74797=CARTESIAN_POINT('',(4.9467595481762,6.44587135576158,24.4167025567876));
#74798=CARTESIAN_POINT('',(-8.12525198907861,0.000116094565966279,15.4167025568297));
#74799=CARTESIAN_POINT('Ctrl Pts',(4.94678612080823,6.44590587665303,16.7083566551695));
#74800=CARTESIAN_POINT('Ctrl Pts',(5.18341558504802,6.26470660955122,16.6966804905928));
#74801=CARTESIAN_POINT('Ctrl Pts',(6.43739680606016,5.19025029452804,16.6320731255035));
#74802=CARTESIAN_POINT('Ctrl Pts',(8.07312723790633,2.56246057378528,16.5145345599018));
#74803=CARTESIAN_POINT('Ctrl Pts',(8.31518029376954,-1.61225440732664,16.3557409583643));
#74804=CARTESIAN_POINT('Ctrl Pts',(6.53042868202404,-5.39398635712584,16.1969473568268));
#74805=CARTESIAN_POINT('Ctrl Pts',(3.15390120175042,-7.86094744934625,16.0381537552892));
#74806=CARTESIAN_POINT('Ctrl Pts',(-0.991381909914889,-8.41182200837257,
15.8793601537517));
#74807=CARTESIAN_POINT('Ctrl Pts',(-4.89501812861923,-6.91233572045668,
15.7205665522142));
#74808=CARTESIAN_POINT('Ctrl Pts',(-7.52742407670693,-3.81971705372047,
15.5663473571833));
#74809=CARTESIAN_POINT('Ctrl Pts',(-8.12495145299739,-1.23397979003354,
15.4650593626648));
#74810=CARTESIAN_POINT('Ctrl Pts',(-8.12581156037035,0.000115800672715422,
15.4167025686589));
#74811=CARTESIAN_POINT('Ctrl Pts',(-8.1252499991706,0.000116095611088758,
15.4167025567876));
#74812=CARTESIAN_POINT('Ctrl Pts',(-8.12524833125246,0.116849637214079,
15.4121281542381));
#74813=CARTESIAN_POINT('Ctrl Pts',(-8.12273074956299,0.233575803540142,
15.4075537516886));
#74814=CARTESIAN_POINT('Ctrl Pts',(-8.11769993863055,0.350193187908608,
15.4029793491391));
#74815=CARTESIAN_POINT('Ctrl Pts',(-8.10865741733798,0.559804559792054,
15.3947571891316));
#74816=CARTESIAN_POINT('Ctrl Pts',(-8.09149033708956,0.769100095999624,
15.386535029124));
#74817=CARTESIAN_POINT('Ctrl Pts',(-8.06624427927133,0.977440939199128,
15.3783128691164));
#74818=CARTESIAN_POINT('Ctrl Pts',(-8.04100287504045,1.18574337908361,15.3700922246936));
#74819=CARTESIAN_POINT('Ctrl Pts',(-8.00768550094828,1.39309118433539,15.3618715802707));
#74820=CARTESIAN_POINT('Ctrl Pts',(-7.96638953334373,1.59885126435561,15.3536509358479));
#74821=CARTESIAN_POINT('Ctrl Pts',(-7.92509820506246,1.80458822861932,15.3454312149589));
#74822=CARTESIAN_POINT('Ctrl Pts',(-7.87583013080488,2.00873753449623,15.33721149407));
#74823=CARTESIAN_POINT('Ctrl Pts',(-7.81873383394003,2.21067609488622,15.3289917731811));
#74824=CARTESIAN_POINT('Ctrl Pts',(-7.76163296216609,2.41263083584496,15.3207713936772));
#74825=CARTESIAN_POINT('Ctrl Pts',(-7.69670269216183,2.61237419261429,15.3125510141733));
#74826=CARTESIAN_POINT('Ctrl Pts',(-7.62414177180475,2.80929703056155,15.3043306346694));
#74827=CARTESIAN_POINT('Ctrl Pts',(-7.55158111997556,3.00621913975188,15.2961102855869));
#74828=CARTESIAN_POINT('Ctrl Pts',(-7.47138997883233,3.20032047498142,15.2878899365044));
#74829=CARTESIAN_POINT('Ctrl Pts',(-7.38381590253885,3.39101021524773,15.2796695874218));
#74830=CARTESIAN_POINT('Ctrl Pts',(-7.29622310173865,3.58174072752639,15.2714474807189));
#74831=CARTESIAN_POINT('Ctrl Pts',(-7.2012443353129,3.7690579192871,15.263225374016));
#74832=CARTESIAN_POINT('Ctrl Pts',(-7.09917441044576,3.9523929780036,15.2550032673131));
#74833=CARTESIAN_POINT('Ctrl Pts',(-7.05441121028773,4.03279534863327,15.2513974274093));
#74834=CARTESIAN_POINT('Ctrl Pts',(-7.00828476682951,4.11243214996698,15.2477915875055));
#74835=CARTESIAN_POINT('Ctrl Pts',(-6.96082269957941,4.19125696033064,15.2441857476017));
#74836=CARTESIAN_POINT('Ctrl Pts',(-6.8525980635358,4.37099600051744,15.2359635875941));
#74837=CARTESIAN_POINT('Ctrl Pts',(-6.73739014407924,4.5465706724238,15.2277414275865));
#74838=CARTESIAN_POINT('Ctrl Pts',(-6.61554461530079,4.71744178612357,15.219519267579));
#74839=CARTESIAN_POINT('Ctrl Pts',(-6.49372154621956,4.88828140327589,15.2112986231561));
#74840=CARTESIAN_POINT('Ctrl Pts',(-6.36526348103575,5.05441895245761,15.2030779787333));
#74841=CARTESIAN_POINT('Ctrl Pts',(-6.2305588173836,5.21534508787516,15.1948573343105));
#74842=CARTESIAN_POINT('Ctrl Pts',(-6.09586928689129,5.37625314432747,15.1866376134216));
#74843=CARTESIAN_POINT('Ctrl Pts',(-5.95493474832005,5.53195072962859,15.1784178925327));
#74844=CARTESIAN_POINT('Ctrl Pts',(-5.80818372688031,5.68196175253783,15.1701981716438));
#74845=CARTESIAN_POINT('Ctrl Pts',(-5.66142094683921,5.83198479525995,15.1619777921399));
#74846=CARTESIAN_POINT('Ctrl Pts',(-5.50884095715798,5.97632015227656,15.153757412636));
#74847=CARTESIAN_POINT('Ctrl Pts',(-5.35090971124037,6.11452801323647,15.1455370331321));
#74848=CARTESIAN_POINT('Ctrl Pts',(-5.19297904978318,6.25273536272681,15.1373166840496));
#74849=CARTESIAN_POINT('Ctrl Pts',(-5.02969739556781,6.38481506916211,15.1290963349671));
#74850=CARTESIAN_POINT('Ctrl Pts',(-4.86156479830643,6.51036675421345,15.1208759858846));
#74851=CARTESIAN_POINT('Ctrl Pts',(-4.69339625205083,6.63594528389144,15.1126538791817));
#74852=CARTESIAN_POINT('Ctrl Pts',(-4.52037492716479,6.75499282706329,15.1044317724788));
#74853=CARTESIAN_POINT('Ctrl Pts',(-4.34303183798392,6.86715093883614,15.0962096657759));
#74854=CARTESIAN_POINT('Ctrl Pts',(-4.26525727110475,6.91633835631831,15.0926038258719));
#74855=CARTESIAN_POINT('Ctrl Pts',(-4.18665187507912,6.96420129217655,15.088997985968));
#74856=CARTESIAN_POINT('Ctrl Pts',(-4.10726211279737,7.01071219629499,15.0853921460641));
#74857=CARTESIAN_POINT('Ctrl Pts',(-3.9262348498468,7.11676795749043,15.0771699860565));
#74858=CARTESIAN_POINT('Ctrl Pts',(-3.74106773711732,7.21582587228796,15.068947826049));
#74859=CARTESIAN_POINT('Ctrl Pts',(-3.55232228419872,7.3075778443808,15.0607256660414));
#74860=CARTESIAN_POINT('Ctrl Pts',(-3.36361162259147,7.39931290389971,15.0525050216186));
#74861=CARTESIAN_POINT('Ctrl Pts',(-3.17132420255942,7.48374457956918,15.0442843771957));
#74862=CARTESIAN_POINT('Ctrl Pts',(-2.97604477205769,7.56061142218062,15.0360637327729));
#74863=CARTESIAN_POINT('Ctrl Pts',(-2.7807872798827,7.63746962932082,15.027844011884));
#74864=CARTESIAN_POINT('Ctrl Pts',(-2.58253872282732,7.70676459202466,15.0196242909951));
#74865=CARTESIAN_POINT('Ctrl Pts',(-2.38190317598133,7.76828326097536,15.0114045701062));
#74866=CARTESIAN_POINT('Ctrl Pts',(-2.18125155297117,7.8298068591833,15.0031841906024));
#74867=CARTESIAN_POINT('Ctrl Pts',(-1.97821283939896,7.88355282951826,14.9949638110985));
#74868=CARTESIAN_POINT('Ctrl Pts',(-1.77340661920289,7.92935788859775,14.9867434315946));
#74869=CARTESIAN_POINT('Ctrl Pts',(-1.56860115693872,7.97516277816522,14.9785230825121));
#74870=CARTESIAN_POINT('Ctrl Pts',(-1.36202848974609,8.01302675344973,14.9703027334295));
#74871=CARTESIAN_POINT('Ctrl Pts',(-1.15431927700282,8.04283747002509,14.962082384347));
#74872=CARTESIAN_POINT('Ctrl Pts',(-0.946565653256594,8.07265456052969,
14.9538602776441));
#74873=CARTESIAN_POINT('Ctrl Pts',(-0.73767529068533,8.09441491037672,14.9456381709412));
#74874=CARTESIAN_POINT('Ctrl Pts',(-0.528285977342776,8.10805781236438,
14.9374160642383));
#74875=CARTESIAN_POINT('Ctrl Pts',(-0.436457402406439,8.1140409651219,14.9338102243344));
#74876=CARTESIAN_POINT('Ctrl Pts',(-0.344532925030685,8.11846356305347,
14.9302043844305));
#74877=CARTESIAN_POINT('Ctrl Pts',(-0.252566526273103,8.12132364287413,
14.9265985445266));
#74878=CARTESIAN_POINT('Ctrl Pts',(-0.0428615848291338,8.12784529512343,
14.918376384519));
#74879=CARTESIAN_POINT('Ctrl Pts',(0.167130694596802,8.12624133064013,14.9101542245115));
#74880=CARTESIAN_POINT('Ctrl Pts',(0.376769833492397,8.11650984445101,14.9019320645039));
#74881=CARTESIAN_POINT('Ctrl Pts',(0.58637032975894,8.10678015205961,14.8937114200811));
#74882=CARTESIAN_POINT('Ctrl Pts',(0.795617520736961,8.08892594172221,14.8854907756582));
#74883=CARTESIAN_POINT('Ctrl Pts',(1.00387283902084,8.06299738841433,14.8772701312354));
#74884=CARTESIAN_POINT('Ctrl Pts',(1.21210476122435,8.03707174800452,14.8690504103465));
#74885=CARTESIAN_POINT('Ctrl Pts',(1.41934474042965,8.00307361203196,14.8608306894576));
#74886=CARTESIAN_POINT('Ctrl Pts',(1.6249603934794,7.96110490334874,14.8526109685688));
#74887=CARTESIAN_POINT('Ctrl Pts',(1.83059252173041,7.9191328318723,14.8443905890649));
#74888=CARTESIAN_POINT('Ctrl Pts',(2.03459977403428,7.86918896794758,14.836170209561));
#74889=CARTESIAN_POINT('Ctrl Pts',(2.23635995797362,7.81142635508216,14.8279498300571));
#74890=CARTESIAN_POINT('Ctrl Pts',(2.43811939525372,7.75366395598037,14.8197294809746));
#74891=CARTESIAN_POINT('Ctrl Pts',(2.6376314977942,7.68808294961918,14.8115091318921));
#74892=CARTESIAN_POINT('Ctrl Pts',(2.83428871821796,7.61488640915164,14.8032887828095));
#74893=CARTESIAN_POINT('Ctrl Pts',(3.03098798658119,7.54167421828644,14.7950666761066));
#74894=CARTESIAN_POINT('Ctrl Pts',(3.22483087668187,7.46084334325658,14.7868445694037));
#74895=CARTESIAN_POINT('Ctrl Pts',(3.41522828601163,7.37264561178184,14.7786224627008));
#74896=CARTESIAN_POINT('Ctrl Pts',(3.49872788057658,7.33396612110172,14.7750166227969));
#74897=CARTESIAN_POINT('Ctrl Pts',(3.58156507489106,7.29387038377963,14.771410782893));
#74898=CARTESIAN_POINT('Ctrl Pts',(3.66369152747975,7.25238250190743,14.7678049429891));
#74899=CARTESIAN_POINT('Ctrl Pts',(3.8509572389557,7.15778134148305,14.7595828640634));
#74900=CARTESIAN_POINT('Ctrl Pts',(4.03458781042971,7.05590753652313,14.7513607851376));
#74901=CARTESIAN_POINT('Ctrl Pts',(4.21401992606655,6.94706582847853,14.7431387062119));
#74902=CARTESIAN_POINT('Ctrl Pts',(4.39342133299661,6.83824274802512,14.7349180344446));
#74903=CARTESIAN_POINT('Ctrl Pts',(4.56862546571034,6.72245429712697,14.7266973626773));
#74904=CARTESIAN_POINT('Ctrl Pts',(4.73909558099361,6.60005004804561,14.71847669091));
#74905=CARTESIAN_POINT('Ctrl Pts',(4.8091274599213,6.54976440391581,14.7150995060647));
#74906=CARTESIAN_POINT('Ctrl Pts',(4.87836070806544,6.49836272531081,14.7117223212193));
#74907=CARTESIAN_POINT('Ctrl Pts',(4.94675954817621,6.44587135576157,14.708345136374));
#74908=CARTESIAN_POINT('',(-8.1252499975661,0.000198877198026241,15.5832974432373));
#74909=CARTESIAN_POINT('Ctrl Pts',(-8.12524999756608,0.000198877834300525,
15.5832974432124));
#74910=CARTESIAN_POINT('Ctrl Pts',(-8.12524452136295,0.223931802217315,
15.5745316392917));
#74911=CARTESIAN_POINT('Ctrl Pts',(-8.11599380670282,0.447621544553009,
15.565765835371));
#74912=CARTESIAN_POINT('Ctrl Pts',(-8.09753449887972,0.670539038351091,
15.5570000314503));
#74913=CARTESIAN_POINT('Ctrl Pts',(-8.09527362566499,0.697841697565204,
15.5559264066167));
#74914=CARTESIAN_POINT('Ctrl Pts',(-8.09287467794545,0.725132776551766,
15.5548527817831));
#74915=CARTESIAN_POINT('Ctrl Pts',(-8.09033777663931,0.752410939834638,
15.5537791569495));
#74916=CARTESIAN_POINT('Ctrl Pts',(-8.07090938060148,0.961315779042493,
15.5455569969417));
#74917=CARTESIAN_POINT('Ctrl Pts',(-8.04338209203338,1.16950218231516,15.5373348369338));
#74918=CARTESIAN_POINT('Ctrl Pts',(-8.0078331243954,1.37633433959039,15.529112676926));
#74919=CARTESIAN_POINT('Ctrl Pts',(-7.97229070947257,1.58312837164571,15.5208920325029));
#74920=CARTESIAN_POINT('Ctrl Pts',(-7.92872961659068,1.78856836519349,15.5126713880798));
#74921=CARTESIAN_POINT('Ctrl Pts',(-7.87727850438065,1.99202683890617,15.5044507436566));
#74922=CARTESIAN_POINT('Ctrl Pts',(-7.82583317235589,2.19546245543225,15.4962310227675));
#74923=CARTESIAN_POINT('Ctrl Pts',(-7.76649966294933,2.39691671052598,15.4880113018783));
#74924=CARTESIAN_POINT('Ctrl Pts',(-7.69945722266801,2.59577465100602,15.4797915809891));
#74925=CARTESIAN_POINT('Ctrl Pts',(-7.63240941053079,2.79464852521692,15.4715712014849));
#74926=CARTESIAN_POINT('Ctrl Pts',(-7.5576515250233,2.99092538858532,15.4633508219807));
#74927=CARTESIAN_POINT('Ctrl Pts',(-7.47541228327836,3.18400671442617,15.4551304424766));
#74928=CARTESIAN_POINT('Ctrl Pts',(-7.39317334587837,3.37708732572584,15.4469100933938));
#74929=CARTESIAN_POINT('Ctrl Pts',(-7.30345322573677,3.56697215266104,15.438689744311));
#74930=CARTESIAN_POINT('Ctrl Pts',(-7.20652847781618,3.75308338049189,15.4304693952282));
#74931=CARTESIAN_POINT('Ctrl Pts',(-7.10958300609048,3.93923440138795,15.422247288525));
#74932=CARTESIAN_POINT('Ctrl Pts',(-7.00542996543054,4.12160994943329,15.4140251818218));
#74933=CARTESIAN_POINT('Ctrl Pts',(-6.89439201400549,4.2996565350871,15.4058030751186));
#74934=CARTESIAN_POINT('Ctrl Pts',(-6.84569584763828,4.37773962330011,15.4021972352164));
#74935=CARTESIAN_POINT('Ctrl Pts',(-6.79567608925784,4.4549904658639,15.3985913953142));
#74936=CARTESIAN_POINT('Ctrl Pts',(-6.7443626269528,4.53136406820974,15.394985555412));
#74937=CARTESIAN_POINT('Ctrl Pts',(-6.62735590756068,4.70551377975176,15.3867633954045));
#74938=CARTESIAN_POINT('Ctrl Pts',(-6.50358105876076,4.87515786872667,15.3785412353971));
#74939=CARTESIAN_POINT('Ctrl Pts',(-6.37341007369604,5.03977495479806,15.3703190753896));
#74940=CARTESIAN_POINT('Ctrl Pts',(-6.24326308295346,5.2043616971228,15.3620984309668));
#74941=CARTESIAN_POINT('Ctrl Pts',(-6.10672249203103,5.36392305456479,15.3538777865441));
#74942=CARTESIAN_POINT('Ctrl Pts',(-5.96420148471735,5.51796957332998,15.3456571421213));
#74943=CARTESIAN_POINT('Ctrl Pts',(-5.82169648867807,5.67199878600723,15.3374374212325));
#74944=CARTESIAN_POINT('Ctrl Pts',(-5.67321261792456,5.82051418034593,15.3292177003437));
#74945=CARTESIAN_POINT('Ctrl Pts',(-5.51920148495797,5.9630615065533,15.320997979455));
#74946=CARTESIAN_POINT('Ctrl Pts',(-5.36517801166409,6.10562025453666,15.3127775999512));
#74947=CARTESIAN_POINT('Ctrl Pts',(-5.20562660599788,6.24220977640885,15.3045572204474));
#74948=CARTESIAN_POINT('Ctrl Pts',(-5.04103446300252,6.37241391509692,15.2963368409436));
#74949=CARTESIAN_POINT('Ctrl Pts',(-4.87644292911781,6.50261757193497,15.2881164918612));
#74950=CARTESIAN_POINT('Ctrl Pts',(-4.70681092834914,6.62643571184036,15.2798961427787));
#74951=CARTESIAN_POINT('Ctrl Pts',(-4.53265775419765,6.74349325244802,15.2716757936963));
#74952=CARTESIAN_POINT('Ctrl Pts',(-4.35846734377206,6.86057582152092,15.2634536869935));
#74953=CARTESIAN_POINT('Ctrl Pts',(-4.17975407371267,6.97089473877623,15.2552315802907));
#74954=CARTESIAN_POINT('Ctrl Pts',(-3.99706608407484,7.07411833955572,15.2470094735879));
#74955=CARTESIAN_POINT('Ctrl Pts',(-3.91694748832893,7.11938748920636,15.2434036336834));
#74956=CARTESIAN_POINT('Ctrl Pts',(-3.83606478217253,7.16329257730237,15.239797793779));
#74957=CARTESIAN_POINT('Ctrl Pts',(-3.75446573782737,7.20580839226109,15.2361919538745));
#74958=CARTESIAN_POINT('Ctrl Pts',(-3.56840079405644,7.30275441391065,15.2279697938669));
#74959=CARTESIAN_POINT('Ctrl Pts',(-3.378548198833,7.3925058607378,15.2197476338593));
#74960=CARTESIAN_POINT('Ctrl Pts',(-3.18548405257249,7.47478286730166,15.2115254738518));
#74961=CARTESIAN_POINT('Ctrl Pts',(-2.99245549368421,7.55704470780534,15.2033048294289));
#74962=CARTESIAN_POINT('Ctrl Pts',(-2.79621683665351,7.63183474220884,15.195084185006));
#74963=CARTESIAN_POINT('Ctrl Pts',(-2.59736507789831,7.69892084740545,15.1868635405832));
#74964=CARTESIAN_POINT('Ctrl Pts',(-2.39853565879714,7.76599941593058,15.1786438196943));
#74965=CARTESIAN_POINT('Ctrl Pts',(-2.19709400359908,7.82537568881756,15.1704240988054));
#74966=CARTESIAN_POINT('Ctrl Pts',(-1.9936540113673,7.87686684192764,15.1622043779165));
#74967=CARTESIAN_POINT('Ctrl Pts',(-1.79019771826208,7.92836212082813,15.1539839984126));
#74968=CARTESIAN_POINT('Ctrl Pts',(-1.58474305364989,7.97197094247569,15.1457636189087));
#74969=CARTESIAN_POINT('Ctrl Pts',(-1.37791693789531,8.00756095666847,15.1375432394048));
#74970=CARTESIAN_POINT('Ctrl Pts',(-1.17109158754778,8.0431508391523,15.1293228903222));
#74971=CARTESIAN_POINT('Ctrl Pts',(-0.962895087532059,8.07072192612209,
15.1211025412397));
#74972=CARTESIAN_POINT('Ctrl Pts',(-0.753962893379013,8.09019329298797,
15.1128821921572));
#74973=CARTESIAN_POINT('Ctrl Pts',(-0.544986026733049,8.10966882309208,
15.1046600854543));
#74974=CARTESIAN_POINT('Ctrl Pts',(-0.335273445622575,8.12104114584314,
15.0964379787514));
#74975=CARTESIAN_POINT('Ctrl Pts',(-0.125465164204048,8.12428126390706,
15.0882158720484));
#74976=CARTESIAN_POINT('Ctrl Pts',(-0.0334528490363855,8.12570223148023,
15.0846100321446));
#74977=CARTESIAN_POINT('Ctrl Pts',(0.0585778449112692,8.12555980823119,
15.0810041922408));
#74978=CARTESIAN_POINT('Ctrl Pts',(0.150572905645268,8.12385471082451,15.077398352337));
#74979=CARTESIAN_POINT('Ctrl Pts',(0.360343203117682,8.11996668914849,15.0691761923294));
#74980=CARTESIAN_POINT('Ctrl Pts',(0.569997443396807,8.10794880024545,15.0609540323218));
#74981=CARTESIAN_POINT('Ctrl Pts',(0.778895841848721,8.08783091008033,15.0527318723142));
#74982=CARTESIAN_POINT('Ctrl Pts',(0.98775573421209,8.06771672823114,15.0445112278914));
#74983=CARTESIAN_POINT('Ctrl Pts',(1.19585976918339,8.03950555335458,15.0362905834685));
#74984=CARTESIAN_POINT('Ctrl Pts',(1.40257265411832,8.00327917246547,15.0280699390456));
#74985=CARTESIAN_POINT('Ctrl Pts',(1.60926231625469,7.96705686136594,15.0198502181567));
#74986=CARTESIAN_POINT('Ctrl Pts',(1.81456084977107,7.92282119287479,15.0116304972678));
#74987=CARTESIAN_POINT('Ctrl Pts',(2.01784170542331,7.87070533143976,15.0034107763789));
#74988=CARTESIAN_POINT('Ctrl Pts',(2.22113884919822,7.81858529415876,14.995190396875));
#74989=CARTESIAN_POINT('Ctrl Pts',(2.42241770549352,7.75858387296805,14.9869700173711));
#74990=CARTESIAN_POINT('Ctrl Pts',(2.6210644389143,7.69088478457186,14.9787496378672));
#74991=CARTESIAN_POINT('Ctrl Pts',(2.81971043719779,7.62318594671149,14.9705292887847));
#74992=CARTESIAN_POINT('Ctrl Pts',(3.01572405358715,7.5477895963651,14.9623089397021));
#74993=CARTESIAN_POINT('Ctrl Pts',(3.20850856123859,7.46492869188706,14.9540885906196));
#74994=CARTESIAN_POINT('Ctrl Pts',(3.40133428879183,7.38205007064129,14.9458664839167));
#74995=CARTESIAN_POINT('Ctrl Pts',(3.59092925705583,7.29170382329379,14.9376443772138));
#74996=CARTESIAN_POINT('Ctrl Pts',(3.77671757964361,7.19417068786326,14.9294222705108));
#74997=CARTESIAN_POINT('Ctrl Pts',(3.85819583959006,7.15139711602993,14.925816430607));
#74998=CARTESIAN_POINT('Ctrl Pts',(3.93894226690403,7.10724189675949,14.9222105907032));
#74999=CARTESIAN_POINT('Ctrl Pts',(4.01890977511006,7.06173150027844,14.9186047507994));
#75000=CARTESIAN_POINT('Ctrl Pts',(4.20125611213359,6.95795617601265,14.9103825151302));
#75001=CARTESIAN_POINT('Ctrl Pts',(4.37961089847017,6.8470971967438,14.9021602794609));
#75002=CARTESIAN_POINT('Ctrl Pts',(4.5534265962013,6.72948688946688,14.8939380437917));
#75003=CARTESIAN_POINT('Ctrl Pts',(4.6873097519285,6.63889645782107,14.8876047903923));
#75004=CARTESIAN_POINT('Ctrl Pts',(4.81850033447646,6.54430141354479,14.8812715369928));
#75005=CARTESIAN_POINT('Ctrl Pts',(4.94675954817619,6.44587135576159,14.8749382835934));
#75006=CARTESIAN_POINT('Ctrl Pts',(4.94675954817621,6.44587135576157,16.8749477411846));
#75007=CARTESIAN_POINT('Ctrl Pts',(5.11829741941736,6.31422792765041,16.8664777791955));
#75008=CARTESIAN_POINT('Ctrl Pts',(5.28456668674438,6.17574134722785,16.8580078172063));
#75009=CARTESIAN_POINT('Ctrl Pts',(5.44503195406664,6.03086350216064,16.8495378552172));
#75010=CARTESIAN_POINT('Ctrl Pts',(5.60549722138891,5.88598565709341,16.841067893228));
#75011=CARTESIAN_POINT('Ctrl Pts',(5.7601582403538,5.73471678322235,16.8325979312388));
#75012=CARTESIAN_POINT('Ctrl Pts',(5.90851966259262,5.57755169937997,16.8241279692497));
#75013=CARTESIAN_POINT('Ctrl Pts',(6.05254053837894,5.42498472693902,16.8159058093031));
#75014=CARTESIAN_POINT('Ctrl Pts',(6.19067275391596,5.26681133952474,16.8076836493564));
#75015=CARTESIAN_POINT('Ctrl Pts',(6.32248991924454,5.10350945757438,16.7994614894098));
#75016=CARTESIAN_POINT('Ctrl Pts',(6.45428278679872,4.94023767695626,16.7912408450487));
#75017=CARTESIAN_POINT('Ctrl Pts',(6.57976274213852,4.77183951809809,16.7830202006876));
#75018=CARTESIAN_POINT('Ctrl Pts',(6.69854362780632,4.59882602724601,16.7747995563265));
#75019=CARTESIAN_POINT('Ctrl Pts',(6.81731116923496,4.42583197330407,16.7665798354999));
#75020=CARTESIAN_POINT('Ctrl Pts',(6.92938097651304,4.24822386574383,16.7583601146733));
#75021=CARTESIAN_POINT('Ctrl Pts',(7.03440971151707,4.06654245926615,16.7501403938467));
#75022=CARTESIAN_POINT('Ctrl Pts',(7.13944686206854,3.8848464953581,16.7419200144055));
#75023=CARTESIAN_POINT('Ctrl Pts',(7.23744166298733,3.69907683455894,16.7336996349644));
#75024=CARTESIAN_POINT('Ctrl Pts',(7.32809578457087,3.50980052633404,16.7254792555233));
#75025=CARTESIAN_POINT('Ctrl Pts',(7.4187495706669,3.3205249185719,16.7172589065036));
#75026=CARTESIAN_POINT('Ctrl Pts',(7.50206260668621,3.12774295668412,16.709038557484));
#75027=CARTESIAN_POINT('Ctrl Pts',(7.57778371056895,2.93204392844579,16.7008182084644));
#75028=CARTESIAN_POINT('Ctrl Pts',(7.65352100463689,2.73630305713668,16.6925961018241));
#75029=CARTESIAN_POINT('Ctrl Pts',(7.72166301709084,2.53764414874344,16.6843739951839));
#75030=CARTESIAN_POINT('Ctrl Pts',(7.78200728077188,2.33667504041822,16.6761518885436));
#75031=CARTESIAN_POINT('Ctrl Pts',(7.80847151749335,2.24853917245015,16.6725460482664));
#75032=CARTESIAN_POINT('Ctrl Pts',(7.83343665589362,2.15995919427053,16.6689402079893));
#75033=CARTESIAN_POINT('Ctrl Pts',(7.85688865322568,2.07098726536731,16.6653343677121));
#75034=CARTESIAN_POINT('Ctrl Pts',(7.91036469779007,1.8681104371108,16.6571122076708));
#75035=CARTESIAN_POINT('Ctrl Pts',(7.95598748355096,1.66312777465361,16.6488900476294));
#75036=CARTESIAN_POINT('Ctrl Pts',(7.9936112373037,1.45666294981097,16.6406678875881));
#75037=CARTESIAN_POINT('Ctrl Pts',(8.03122805589937,1.25023618246787,16.632447243131));
#75038=CARTESIAN_POINT('Ctrl Pts',(8.06084873241069,1.04232808823558,16.624226598674));
#75039=CARTESIAN_POINT('Ctrl Pts',(8.08237867119612,0.833572179174715,16.616005954217));
#75040=CARTESIAN_POINT('Ctrl Pts',(8.10390619123909,0.624839722422922,16.6077862332935));
#75041=CARTESIAN_POINT('Ctrl Pts',(8.11734475792283,0.415259934465333,16.5995665123701));
#75042=CARTESIAN_POINT('Ctrl Pts',(8.12265158977301,0.205471929123945,16.5913467914467));
#75043=CARTESIAN_POINT('Ctrl Pts',(8.12795884683955,-0.00433288573640242,
16.5831264119081));
#75044=CARTESIAN_POINT('Ctrl Pts',(8.12513305698705,-0.214345656326267,
16.5749060323695));
#75045=CARTESIAN_POINT('Ctrl Pts',(8.11418354199454,-0.423925712035658,
16.566685652831));
#75046=CARTESIAN_POINT('Ctrl Pts',(8.10323406752314,-0.633504992147367,
16.5584653037138));
#75047=CARTESIAN_POINT('Ctrl Pts',(8.08416094611475,-0.842651265979325,
16.5502449545965));
#75048=CARTESIAN_POINT('Ctrl Pts',(8.0570255405828,-1.05072689167856,16.5420246054793));
#75049=CARTESIAN_POINT('Ctrl Pts',(8.02988433313923,-1.2588470067217,16.5338024987418));
#75050=CARTESIAN_POINT('Ctrl Pts',(7.99467743588163,-1.46589572357169,16.5255803920043));
#75051=CARTESIAN_POINT('Ctrl Pts',(7.95151786401598,-1.67124241830284,16.5173582852668));
#75052=CARTESIAN_POINT('Ctrl Pts',(7.93259005116643,-1.76129808009773,16.5137524455694));
#75053=CARTESIAN_POINT('Ctrl Pts',(7.91213336603844,-1.85102651469605,16.510146605872));
#75054=CARTESIAN_POINT('Ctrl Pts',(7.8901604319332,-1.94037520105149,16.5065407661746));
#75055=CARTESIAN_POINT('Ctrl Pts',(7.84005699004637,-2.14411115606933,16.4983186061815));
#75056=CARTESIAN_POINT('Ctrl Pts',(7.78204990350035,-2.3459390725583,16.4900964461883));
#75057=CARTESIAN_POINT('Ctrl Pts',(7.71630954770293,-2.54524154581222,16.4818742861951));
#75058=CARTESIAN_POINT('Ctrl Pts',(7.65058130977847,-2.74450728178321,16.4736536417869));
#75059=CARTESIAN_POINT('Ctrl Pts',(7.57712274004723,-2.94124822347166,16.4654329973786));
#75060=CARTESIAN_POINT('Ctrl Pts',(7.49615386213667,-3.1348628100243,16.4572123529703));
#75061=CARTESIAN_POINT('Ctrl Pts',(7.41519408053462,-3.32845564528119,16.4489926320962));
#75062=CARTESIAN_POINT('Ctrl Pts',(7.32672578903245,-3.51892255441356,16.440772911222));
#75063=CARTESIAN_POINT('Ctrl Pts',(7.23101719068251,-3.70568184691482,16.4325531903478));
#75064=CARTESIAN_POINT('Ctrl Pts',(7.13530092356684,-3.89245610372739,16.4243328108586));
#75065=CARTESIAN_POINT('Ctrl Pts',(7.03234332261003,-4.07552188640379,16.4161124313695));
#75066=CARTESIAN_POINT('Ctrl Pts',(6.9224590889106,-4.25432106508888,16.4078920518804));
#75067=CARTESIAN_POINT('Ctrl Pts',(6.81257526186324,-4.43311958208618,16.3996717028126));
#75068=CARTESIAN_POINT('Ctrl Pts',(6.69576501015939,-4.60765127662146,16.3914513537449));
#75069=CARTESIAN_POINT('Ctrl Pts',(6.57238728445004,-4.77738557641095,16.3832310046772));
#75070=CARTESIAN_POINT('Ctrl Pts',(6.44898317893375,-4.94715616766256,16.375008897989));
#75071=CARTESIAN_POINT('Ctrl Pts',(6.31900896763612,-5.11212707613925,16.3667867913007));
#75072=CARTESIAN_POINT('Ctrl Pts',(6.18286560094914,-5.27179860418622,16.3585646846125));
#75073=CARTESIAN_POINT('Ctrl Pts',(6.12315934623455,-5.34182323451699,16.3549588446207));
#75074=CARTESIAN_POINT('Ctrl Pts',(6.06226710345063,-5.4108290610488,16.3513530046289));
#75075=CARTESIAN_POINT('Ctrl Pts',(6.00022508505059,-5.47877600301651,16.3477471646371));
#75076=CARTESIAN_POINT('Ctrl Pts',(5.85875474696184,-5.63371095033383,16.3395250046254));
#75077=CARTESIAN_POINT('Ctrl Pts',(5.71125687210847,-5.78318906605329,16.3313028446137));
#75078=CARTESIAN_POINT('Ctrl Pts',(5.55817645593022,-5.92674970344142,16.323080684602));
#75079=CARTESIAN_POINT('Ctrl Pts',(5.40512425695113,-6.07028387840413,16.3148600401749));
#75080=CARTESIAN_POINT('Ctrl Pts',(5.24649178561628,-6.20790255025607,16.3066393957479));
#75081=CARTESIAN_POINT('Ctrl Pts',(5.08276005461068,-6.33918273831525,16.2984187513208));
#75082=CARTESIAN_POINT('Ctrl Pts',(4.91904671776042,-6.470448177931,16.2901990304277));
#75083=CARTESIAN_POINT('Ctrl Pts',(4.75023549510396,-6.59537637082879,16.2819793095345));
#75084=CARTESIAN_POINT('Ctrl Pts',(4.57684020039286,-6.71358483543388,16.2737595886414));
#75085=CARTESIAN_POINT('Ctrl Pts',(4.40343101217637,-6.8318027716336,16.2655392091333));
#75086=CARTESIAN_POINT('Ctrl Pts',(4.2254372603307,-6.9432997351995,16.2573188296252));
#75087=CARTESIAN_POINT('Ctrl Pts',(4.04340231766253,-7.04773617979712,16.2490984501171));
#75088=CARTESIAN_POINT('Ctrl Pts',(3.86136804865659,-7.15217223790362,16.2408781010304));
#75089=CARTESIAN_POINT('Ctrl Pts',(3.67529287607674,-7.24954768475143,16.2326577519437));
#75090=CARTESIAN_POINT('Ctrl Pts',(3.48574584508091,-7.33956834330202,16.224437402857));
#75091=CARTESIAN_POINT('Ctrl Pts',(3.29615828639918,-7.42960824947129,16.21621529615));
#75092=CARTESIAN_POINT('Ctrl Pts',(3.10309765292968,-7.51229009904726,16.2079931894429));
#75093=CARTESIAN_POINT('Ctrl Pts',(2.9071550995866,-7.58736692070758,16.1997710827358));
#75094=CARTESIAN_POINT('Ctrl Pts',(2.82122365914698,-7.62029218027385,16.1961652428571));
#75095=CARTESIAN_POINT('Ctrl Pts',(2.73473819679738,-7.65175539049154,16.1925594029783));
#75096=CARTESIAN_POINT('Ctrl Pts',(2.64774968743878,-7.68173868047904,16.1889535630996));
#75097=CARTESIAN_POINT('Ctrl Pts',(2.44939549900504,-7.75010760869606,16.180731403092));
#75098=CARTESIAN_POINT('Ctrl Pts',(2.24835907894321,-7.81080100149879,16.1725092430844));
#75099=CARTESIAN_POINT('Ctrl Pts',(2.04525157618255,-7.86362725163285,16.1642870830768));
#75100=CARTESIAN_POINT('Ctrl Pts',(1.84218151207885,-7.91644376434298,16.1560664386539));
#75101=CARTESIAN_POINT('Ctrl Pts',(1.63704141271484,-7.96139595441826,16.147845794231));
#75102=CARTESIAN_POINT('Ctrl Pts',(1.43045603417608,-7.99834252184721,16.1396251498081));
#75103=CARTESIAN_POINT('Ctrl Pts',(1.22389386411197,-8.03528493857838,16.1314054289192));
#75104=CARTESIAN_POINT('Ctrl Pts',(1.01588702944717,-8.0642234762678,16.1231857080303));
#75105=CARTESIAN_POINT('Ctrl Pts',(0.80706971379653,-8.08506809121434,16.1149659871414));
#75106=CARTESIAN_POINT('Ctrl Pts',(0.598235666406607,-8.1059143763608,16.1067456076374));
#75107=CARTESIAN_POINT('Ctrl Pts',(0.388591301695215,-8.11866541089209,
16.0985252281335));
#75108=CARTESIAN_POINT('Ctrl Pts',(0.178776218394585,-8.12328299557737,
16.0903048486295));
#75109=CARTESIAN_POINT('Ctrl Pts',(-0.0310380884386643,-8.12790056317426,
16.0820844995469));
#75110=CARTESIAN_POINT('Ctrl Pts',(-0.241022817466202,-8.12438473731043,
16.0738641504643));
#75111=CARTESIAN_POINT('Ctrl Pts',(-0.450537532377986,-8.1127494411216,
16.0656438013817));
#75112=CARTESIAN_POINT('Ctrl Pts',(-0.660097044332808,-8.10111165715111,
16.0574216946787));
#75113=CARTESIAN_POINT('Ctrl Pts',(-0.869186046652183,-8.08135095093156,
16.0491995879757));
#75114=CARTESIAN_POINT('Ctrl Pts',(-1.07716727245303,-8.05353327612521,
16.0409774812727));
#75115=CARTESIAN_POINT('Ctrl Pts',(-1.16837832459194,-8.04133371639392,
16.0373716413692));
#75116=CARTESIAN_POINT('Ctrl Pts',(-1.25937639108115,-8.02758523259906,
16.0337658014656));
#75117=CARTESIAN_POINT('Ctrl Pts',(-1.35010815957349,-8.01229651972224,
16.0301599615621));
#75118=CARTESIAN_POINT('Ctrl Pts',(-1.55699785467115,-7.97743467146244,
16.0219378015556));
#75119=CARTESIAN_POINT('Ctrl Pts',(-1.76257068892938,-7.93454947677531,
16.0137156415492));
#75120=CARTESIAN_POINT('Ctrl Pts',(-1.96619832597162,-7.88376507168031,
16.0054934815427));
#75121=CARTESIAN_POINT('Ctrl Pts',(-2.16978842848168,-7.83299002763725,
15.997272837121));
#75122=CARTESIAN_POINT('Ctrl Pts',(-2.3714337631785,-7.77431875065692,15.9890521926992));
#75123=CARTESIAN_POINT('Ctrl Pts',(-2.57051811332891,-7.70792606292691,
15.9808315482774));
#75124=CARTESIAN_POINT('Ctrl Pts',(-2.76958009769652,-7.64154083396717,
15.9726118273896));
#75125=CARTESIAN_POINT('Ctrl Pts',(-2.96608139203507,-7.56743601939258,
15.9643921065017));
#75126=CARTESIAN_POINT('Ctrl Pts',(-3.15942202355638,-7.48583596130498,
15.9561723856139));
#75127=CARTESIAN_POINT('Ctrl Pts',(-3.35277814672597,-7.40422936491558,
15.9479520061111));
#75128=CARTESIAN_POINT('Ctrl Pts',(-3.54297282806777,-7.31512643727572,
15.9397316266083));
#75129=CARTESIAN_POINT('Ctrl Pts',(-3.72942614353552,-7.21879963722597,
15.9315112471055));
#75130=CARTESIAN_POINT('Ctrl Pts',(-3.91587876898924,-7.12247319365603,
15.9232908980242));
#75131=CARTESIAN_POINT('Ctrl Pts',(-4.0985897952732,-7.01892306899367,15.9150705489428));
#75132=CARTESIAN_POINT('Ctrl Pts',(-4.27700349969413,-6.90846789281851,
15.9068501998615));
#75133=CARTESIAN_POINT('Ctrl Pts',(-4.45545535134861,-6.79798909985103,
15.8986280931597));
#75134=CARTESIAN_POINT('Ctrl Pts',(-4.62960779451056,-6.68060246121653,
15.8904059864579));
#75135=CARTESIAN_POINT('Ctrl Pts',(-4.798932782557,-6.55667077951911,15.8821838797561));
#75136=CARTESIAN_POINT('Ctrl Pts',(-4.8731909771889,-6.50232001270836,15.8785780398456));
#75137=CARTESIAN_POINT('Ctrl Pts',(-4.94652109332637,-6.44671099355055,
15.874972199935));
#75138=CARTESIAN_POINT('Ctrl Pts',(-5.01888047592989,-6.38987686351073,
15.8713663600245));
#75139=CARTESIAN_POINT('Ctrl Pts',(-5.18387682536536,-6.2602817281944,15.863144200016));
#75140=CARTESIAN_POINT('Ctrl Pts',(-5.34387820306937,-6.1242711063155,15.8549220400074));
#75141=CARTESIAN_POINT('Ctrl Pts',(-5.49839224065822,-5.9822546193195,15.8466998799989));
#75142=CARTESIAN_POINT('Ctrl Pts',(-5.652877796788,-5.84026431011826,15.8384792355751));
#75143=CARTESIAN_POINT('Ctrl Pts',(-5.80187781438076,-5.69227054495628,
15.8302585911513));
#75144=CARTESIAN_POINT('Ctrl Pts',(-5.94493481736284,-5.53872165574396,
15.8220379467275));
#75145=CARTESIAN_POINT('Ctrl Pts',(-6.08797574885572,-5.38519001671346,
15.8138182258376));
#75146=CARTESIAN_POINT('Ctrl Pts',(-6.22507479755883,-5.22610471542581,
15.8055985049477));
#75147=CARTESIAN_POINT('Ctrl Pts',(-6.35581244339621,-5.06194979695274,
15.7973787840578));
#75148=CARTESIAN_POINT('Ctrl Pts',(-6.48656056474432,-4.89778172536987,
15.789158404553));
#75149=CARTESIAN_POINT('Ctrl Pts',(-6.61094607875186,-4.72854345413192,
15.7809380250481));
#75150=CARTESIAN_POINT('Ctrl Pts',(-6.7285900911127,-4.55475168898152,15.7727176455432));
#75151=CARTESIAN_POINT('Ctrl Pts',(-6.84623366810529,-4.3809605669868,15.7644972964597));
#75152=CARTESIAN_POINT('Ctrl Pts',(-6.95713563011982,-4.20261623069591,
15.7562769473762));
#75153=CARTESIAN_POINT('Ctrl Pts',(-7.06096042411412,-4.02026435095929,
15.7480565982927));
#75154=CARTESIAN_POINT('Ctrl Pts',(-7.16480741723577,-3.83787348195579,
15.7398344915888));
#75155=CARTESIAN_POINT('Ctrl Pts',(-7.26157407320873,-3.65147361419057,
15.7316123848849));
#75156=CARTESIAN_POINT('Ctrl Pts',(-7.35097027573048,-3.46163596697096,
15.723390278181));
#75157=CARTESIAN_POINT('Ctrl Pts',(-7.39017536092233,-3.3783818586093,15.719784438283));
#75158=CARTESIAN_POINT('Ctrl Pts',(-7.42796349162727,-3.29446686553102,
15.716178598385));
#75159=CARTESIAN_POINT('Ctrl Pts',(-7.46431306717456,-3.20994049753374,
15.712572758487));
#75160=CARTESIAN_POINT('Ctrl Pts',(-7.54686890659341,-3.01796727204274,
15.7043833055124));
#75161=CARTESIAN_POINT('Ctrl Pts',(-7.62203047401269,-2.82277096174243,
15.6961938525379));
#75162=CARTESIAN_POINT('Ctrl Pts',(-7.68956225568293,-2.62494188097117,
15.6880043995633));
#75163=CARTESIAN_POINT('Ctrl Pts',(-7.75708055109871,-2.4271523071292,15.6798165820416));
#75164=CARTESIAN_POINT('Ctrl Pts',(-7.81697200482374,-2.22673129573819,
15.67162876452));
#75165=CARTESIAN_POINT('Ctrl Pts',(-7.86905023528938,-2.02428653035882,
15.6634409469983));
#75166=CARTESIAN_POINT('Ctrl Pts',(-7.92112674591894,-1.82184845053327,
15.6552533998718));
#75167=CARTESIAN_POINT('Ctrl Pts',(-7.96539047091651,-1.61738703977369,
15.6470658527453));
#75168=CARTESIAN_POINT('Ctrl Pts',(-8.0017054032708,-1.41152336210451,15.6388783056189));
#75169=CARTESIAN_POINT('Ctrl Pts',(-8.03801842105186,-1.20567053785188,
15.6306911901511));
#75170=CARTESIAN_POINT('Ctrl Pts',(-8.06638343269783,-0.99841588989253,
15.6225040746834));
#75171=CARTESIAN_POINT('Ctrl Pts',(-8.08671577975118,-0.79038943567284,
15.6143169592157));
#75172=CARTESIAN_POINT('Ctrl Pts',(-8.10705089490952,-0.58233466012534,
15.6061287291302));
#75173=CARTESIAN_POINT('Ctrl Pts',(-8.11935113195728,-0.373508166877472,
15.5979404990448));
#75174=CARTESIAN_POINT('Ctrl Pts',(-8.12358372655715,-0.164544827070897,
15.5897522689593));
#75175=CARTESIAN_POINT('Ctrl Pts',(-8.12469591890351,-0.109635852984543,
15.5876006603853));
#75176=CARTESIAN_POINT('Ctrl Pts',(-8.12525134172209,-0.0547174411157915,
15.5854490518113));
#75177=CARTESIAN_POINT('Ctrl Pts',(-8.1252499975661,0.000198877198045901,
15.5832974432373));
#75178=CARTESIAN_POINT('Origin',(0.,0.,24.4167025567876));
#75179=CARTESIAN_POINT('',(4.94710325578446,6.44631862759455,18.8749389137103));
#75180=CARTESIAN_POINT('',(4.94687992157187,6.44602802604219,18.7083406766545));
#75181=CARTESIAN_POINT('',(4.9467595481762,6.44587135576158,24.4167025567876));
#75182=CARTESIAN_POINT('',(-8.12473160140278,0.000169117238404473,19.5832974432124));
#75183=CARTESIAN_POINT('Ctrl Pts',(-8.12473160140278,0.000169117238404473,
19.5832974432124));
#75184=CARTESIAN_POINT('Ctrl Pts',(-8.12504359874105,0.508019142218013,
19.5634046939374));
#75185=CARTESIAN_POINT('Ctrl Pts',(-7.95342738081474,2.36695158764184,19.49058074415));
#75186=CARTESIAN_POINT('Ctrl Pts',(-6.5521428145264,5.36767209002086,19.3648255938499));
#75187=CARTESIAN_POINT('Ctrl Pts',(-3.18555877319028,7.84813792090891,19.2060319923125));
#75188=CARTESIAN_POINT('Ctrl Pts',(0.957454270241905,8.41576578597796,19.0472383907749));
#75189=CARTESIAN_POINT('Ctrl Pts',(3.67473557222166,7.38452740613752,18.9368740312409));
#75190=CARTESIAN_POINT('Ctrl Pts',(4.85600651503698,6.5163309368714,18.8794408722194));
#75191=CARTESIAN_POINT('Ctrl Pts',(4.94710325578446,6.44631862759455,18.8749389137103));
#75192=CARTESIAN_POINT('',(-2.10208451021638,-7.84862588447228,20.));
#75193=CARTESIAN_POINT('Ctrl Pts',(-2.10208451021637,-7.84862588447229,
20.));
#75194=CARTESIAN_POINT('Ctrl Pts',(-3.4072189357264,-7.49907388645407,19.9470687994875));
#75195=CARTESIAN_POINT('Ctrl Pts',(-5.83842156753237,-6.13666000427729,
19.8412063984625));
#75196=CARTESIAN_POINT('Ctrl Pts',(-7.7841496768604,-3.03846725289262,19.7023055461999));
#75197=CARTESIAN_POINT('Ctrl Pts',(-8.12421342723266,-0.843282838764658,
19.6163358944499));
#75198=CARTESIAN_POINT('Ctrl Pts',(-8.12473160140278,0.000169117238404473,
19.5832974432124));
#75199=CARTESIAN_POINT('',(2.10231591215296,-7.84925099980569,20.));
#75200=CARTESIAN_POINT('Origin',(0.,0.,20.));
#75201=CARTESIAN_POINT('',(-8.12506026921708,0.000206357840382317,19.4167025567876));
#75202=CARTESIAN_POINT('Ctrl Pts',(2.10231591215296,-7.84925099980569,20.));
#75203=CARTESIAN_POINT('Ctrl Pts',(0.863038871999875,-8.18056558660505,
19.9497333973966));
#75204=CARTESIAN_POINT('Ctrl Pts',(-1.84558751149673,-8.24902228982473,
19.8465355942806));
#75205=CARTESIAN_POINT('Ctrl Pts',(-5.52703238734317,-6.41823528948013,
19.6904065906521));
#75206=CARTESIAN_POINT('Ctrl Pts',(-7.70327725426576,-3.30735306071981,
19.5462407121848));
#75207=CARTESIAN_POINT('Ctrl Pts',(-8.12411843531473,-0.977581626766432,
19.45500603423));
#75208=CARTESIAN_POINT('Ctrl Pts',(-8.12506026921708,0.000206357840382317,
19.4167025567876));
#75209=CARTESIAN_POINT('Ctrl Pts',(-8.12506026921708,0.000206357840382317,
19.4167025567876));
#75210=CARTESIAN_POINT('Ctrl Pts',(-8.12541994636447,0.373614017280771,
19.4020748337174));
#75211=CARTESIAN_POINT('Ctrl Pts',(-8.00870660044479,2.09799453871542,19.3345159101348));
#75212=CARTESIAN_POINT('Ctrl Pts',(-6.81029807173662,5.03601435634795,19.2140257860396));
#75213=CARTESIAN_POINT('Ctrl Pts',(-3.57092777478972,7.68049794291721,19.0552321845021));
#75214=CARTESIAN_POINT('Ctrl Pts',(0.538848536797422,8.45288346202083,18.8964385829646));
#75215=CARTESIAN_POINT('Ctrl Pts',(3.43586812217437,7.51499625442789,18.7808080803487));
#75216=CARTESIAN_POINT('Ctrl Pts',(4.74924899934986,6.59802379651327,18.7181087782453));
#75217=CARTESIAN_POINT('Ctrl Pts',(4.94687992157187,6.44602802604219,18.7083406766545));
#75218=CARTESIAN_POINT('Origin',(0.,0.,10.));
#75219=CARTESIAN_POINT('',(-6.57226796657889,2.44190915842114,0.660259531491259));
#75220=CARTESIAN_POINT('',(-6.57226803330854,2.44190897882182,0.113027768592106));
#75221=CARTESIAN_POINT('',(-6.57226799596304,2.44190907933527,10.));
#75222=CARTESIAN_POINT('',(-5.31037376991248,4.57794244025912,0.));
#75223=CARTESIAN_POINT('Ctrl Pts',(-6.57226803330854,2.44190897882183,0.113027768592105));
#75224=CARTESIAN_POINT('Ctrl Pts',(-6.48443345352562,2.67831107485938,0.101407930745955));
#75225=CARTESIAN_POINT('Ctrl Pts',(-6.38388671904456,2.90985881189943,0.0898378038016317));
#75226=CARTESIAN_POINT('Ctrl Pts',(-6.17965164134882,3.31832780391347,0.0690489203037348));
#75227=CARTESIAN_POINT('Ctrl Pts',(-6.08030470536102,3.49704022444068,0.0598108240986432));
#75228=CARTESIAN_POINT('Ctrl Pts',(-5.77692312506962,3.99066819037698,0.0337236943739866));
#75229=CARTESIAN_POINT('Ctrl Pts',(-5.55523859827604,4.29390135003466,0.0170257482840738));
#75230=CARTESIAN_POINT('Ctrl Pts',(-5.31037376991249,4.57794244025909,4.3758399681515E-15));
#75231=CARTESIAN_POINT('',(5.30568034743329,4.58338113332943,0.));
#75232=CARTESIAN_POINT('Origin',(0.,0.,0.));
#75233=CARTESIAN_POINT('Ctrl Pts',(5.30568034743329,4.58338113332944,6.94323071259717E-15));
#75234=CARTESIAN_POINT('Ctrl Pts',(4.96791334889641,4.97437714130201,0.0236067383578522));
#75235=CARTESIAN_POINT('Ctrl Pts',(4.58795008248023,5.3268511784941,0.0475070844258374));
#75236=CARTESIAN_POINT('Ctrl Pts',(3.85055355547309,5.87295169038987,0.0891721388758242));
#75237=CARTESIAN_POINT('Ctrl Pts',(3.50853732234251,6.08346078767968,0.107069906261077));
#75238=CARTESIAN_POINT('Ctrl Pts',(3.02818103051952,6.32506641310171,0.131176288252661));
#75239=CARTESIAN_POINT('Ctrl Pts',(2.90418137948066,6.38295193387525,0.137318833587793));
#75240=CARTESIAN_POINT('Ctrl Pts',(2.67245720329945,6.482974364138,0.148721669371288));
#75241=CARTESIAN_POINT('Ctrl Pts',(2.56523174226913,6.52614506999249,0.153974771223025));
#75242=CARTESIAN_POINT('Ctrl Pts',(2.17852954815138,6.67083431627747,0.172846788730674));
#75243=CARTESIAN_POINT('Ctrl Pts',(1.89372568641637,6.75720535105471,0.186569527123648));
#75244=CARTESIAN_POINT('Ctrl Pts',(1.41195725613856,6.87044711760687,0.209290931356877));
#75245=CARTESIAN_POINT('Ctrl Pts',(1.21778600242591,6.90750793300775,0.218323788242286));
#75246=CARTESIAN_POINT('Ctrl Pts',(0.569258507063312,7.00309095687257,0.248116670311023));
#75247=CARTESIAN_POINT('Ctrl Pts',(0.110757790567507,7.02531672066892,0.268505037624363));
#75248=CARTESIAN_POINT('Ctrl Pts',(-0.507914252363528,6.99469271472608,
0.296307214694604));
#75249=CARTESIAN_POINT('Ctrl Pts',(-0.668872106733601,6.981139755992,0.303577181476585));
#75250=CARTESIAN_POINT('Ctrl Pts',(-1.01378136682171,6.94005912625189,0.319374000659245));
#75251=CARTESIAN_POINT('Ctrl Pts',(-1.19739547110362,6.91074640970429,0.327908120856951));
#75252=CARTESIAN_POINT('Ctrl Pts',(-1.62259330619564,6.82541052256908,0.347855654488837));
#75253=CARTESIAN_POINT('Ctrl Pts',(-1.86280722624768,6.76379988414577,0.359263260409735));
#75254=CARTESIAN_POINT('Ctrl Pts',(-2.19577880582656,6.65931050020424,0.375227639560647));
#75255=CARTESIAN_POINT('Ctrl Pts',(-2.29163631047198,6.62693474892065,0.379842851859015));
#75256=CARTESIAN_POINT('Ctrl Pts',(-2.60973911421866,6.51176818465846,0.39523099159136));
#75257=CARTESIAN_POINT('Ctrl Pts',(-2.82848107349163,6.41977887178156,0.405927506613424));
#75258=CARTESIAN_POINT('Ctrl Pts',(-3.27268329389293,6.20585578736824,0.428068426288916));
#75259=CARTESIAN_POINT('Ctrl Pts',(-3.49697169700823,6.08229317503956,0.439487904763073));
#75260=CARTESIAN_POINT('Ctrl Pts',(-3.77417559254421,5.90916731010841,0.454174195423844));
#75261=CARTESIAN_POINT('Ctrl Pts',(-3.83377469301685,5.87067553207248,0.457367927034044));
#75262=CARTESIAN_POINT('Ctrl Pts',(-3.99875996351912,5.76053667290316,0.466326447082652));
#75263=CARTESIAN_POINT('Ctrl Pts',(-4.10278982410944,5.68691292843994,0.472119387767559));
#75264=CARTESIAN_POINT('Ctrl Pts',(-4.42553216947801,5.44503547688161,0.49056508378768));
#75265=CARTESIAN_POINT('Ctrl Pts',(-4.6363499694602,5.26668822082289,0.503293603600562));
#75266=CARTESIAN_POINT('Ctrl Pts',(-5.01970741925679,4.90147582916418,0.527613906159142));
#75267=CARTESIAN_POINT('Ctrl Pts',(-5.19368418101213,4.71673363498409,0.539197663955715));
#75268=CARTESIAN_POINT('Ctrl Pts',(-5.53830840738503,4.30854048464011,0.563415701596132));
#75269=CARTESIAN_POINT('Ctrl Pts',(-5.70630889343921,4.08343277863767,0.576006412544775));
#75270=CARTESIAN_POINT('Ctrl Pts',(-6.00100774244055,3.63471730934702,0.600055436935681));
#75271=CARTESIAN_POINT('Ctrl Pts',(-6.12980373036217,3.413028955647,0.611501325720239));
#75272=CARTESIAN_POINT('Ctrl Pts',(-6.30993120414253,3.05975397798143,0.629456560710598));
#75273=CARTESIAN_POINT('Ctrl Pts',(-6.36991585719028,2.93283080971328,0.635864537870555));
#75274=CARTESIAN_POINT('Ctrl Pts',(-6.47815530853341,2.68479101819484,0.648274547622285));
#75275=CARTESIAN_POINT('Ctrl Pts',(-6.52691228708205,2.5639815452794,0.654267302790969));
#75276=CARTESIAN_POINT('Ctrl Pts',(-6.57226796657889,2.44190915842114,0.660259531491259));
#75277=CARTESIAN_POINT('Origin',(0.,0.,10.));
#75278=CARTESIAN_POINT('',(-6.57226793021668,2.44190925628809,2.66021763119828));
#75279=CARTESIAN_POINT('',(-6.57226800353884,2.44190905894539,2.1130822547889));
#75280=CARTESIAN_POINT('',(-6.57226799596304,2.44190907933527,10.));
#75281=CARTESIAN_POINT('Ctrl Pts',(-6.57226800353884,2.44190905894539,2.1130822547889));
#75282=CARTESIAN_POINT('Ctrl Pts',(-6.49279312640791,2.65581145229596,2.10284308653732));
#75283=CARTESIAN_POINT('Ctrl Pts',(-6.40291465001429,2.86572907629688,2.09265138196384));
#75284=CARTESIAN_POINT('Ctrl Pts',(-6.25383406080689,3.17171237278575,2.07736071604314));
#75285=CARTESIAN_POINT('Ctrl Pts',(-6.20231043424039,3.27132154565605,2.07231009358979));
#75286=CARTESIAN_POINT('Ctrl Pts',(-6.08508969571202,3.48520790432581,2.06125649921506));
#75287=CARTESIAN_POINT('Ctrl Pts',(-6.01851470692794,3.5989540390872,2.0552377909509));
#75288=CARTESIAN_POINT('Ctrl Pts',(-5.80822232179475,3.93607744699537,2.03701748118551));
#75289=CARTESIAN_POINT('Ctrl Pts',(-5.65498086469982,4.15323297416772,2.02476943204738));
#75290=CARTESIAN_POINT('Ctrl Pts',(-5.36701183334432,4.51572497144245,2.00352705492179));
#75291=CARTESIAN_POINT('Ctrl Pts',(-5.23775930831982,4.66502596046627,1.99451177070619));
#75292=CARTESIAN_POINT('Ctrl Pts',(-4.82370543706551,5.10436928212147,1.9671001200107));
#75293=CARTESIAN_POINT('Ctrl Pts',(-4.51985522445697,5.37527987021319,1.94896666566469));
#75294=CARTESIAN_POINT('Ctrl Pts',(-4.04376068101001,5.73069775673144,1.92233086230248));
#75295=CARTESIAN_POINT('Ctrl Pts',(-3.88881481972275,5.83695252404356,1.91389524311176));
#75296=CARTESIAN_POINT('Ctrl Pts',(-3.5141836513171,6.07231218219803,1.89379320727144));
#75297=CARTESIAN_POINT('Ctrl Pts',(-3.29135777375622,6.19591988878065,1.88207047139596));
#75298=CARTESIAN_POINT('Ctrl Pts',(-2.79373886227124,6.43752915577014,1.85661779779701));
#75299=CARTESIAN_POINT('Ctrl Pts',(-2.51711303562919,6.55064161661477,1.84292144775973));
#75300=CARTESIAN_POINT('Ctrl Pts',(-2.00143274165636,6.7239983977605,1.81819065650761));
#75301=CARTESIAN_POINT('Ctrl Pts',(-1.76479801681821,6.78994686428469,1.8071292352449));
#75302=CARTESIAN_POINT('Ctrl Pts',(-1.30041644677844,6.8934444387163,1.78577738801826));
#75303=CARTESIAN_POINT('Ctrl Pts',(-1.07331225438102,6.93243532046221,1.77549348767729));
#75304=CARTESIAN_POINT('Ctrl Pts',(-0.694225197395039,6.97844215541894,
1.75834063160464));
#75305=CARTESIAN_POINT('Ctrl Pts',(-0.54319809609625,6.99181941615377,1.75150790838926));
#75306=CARTESIAN_POINT('Ctrl Pts',(-0.144797896936059,7.01412067457361,
1.73334900114839));
#75307=CARTESIAN_POINT('Ctrl Pts',(0.102816355217044,7.01486149949597,1.72195436564623));
#75308=CARTESIAN_POINT('Ctrl Pts',(0.643198637537469,6.98785610048713,1.69706021019252));
#75309=CARTESIAN_POINT('Ctrl Pts',(0.935243580742794,6.95479415869257,1.68359416102377));
#75310=CARTESIAN_POINT('Ctrl Pts',(1.68928804648194,6.82106240345378,1.64878674172699));
#75311=CARTESIAN_POINT('Ctrl Pts',(2.14469936525171,6.69184982170806,1.62778302068919));
#75312=CARTESIAN_POINT('Ctrl Pts',(2.7255129671203,6.46161666541025,1.59972124012996));
#75313=CARTESIAN_POINT('Ctrl Pts',(2.86549027479619,6.40077149314128,1.59284387525232));
#75314=CARTESIAN_POINT('Ctrl Pts',(3.2293496599641,6.22827984587918,1.57452009409872));
#75315=CARTESIAN_POINT('Ctrl Pts',(3.44943235845743,6.10913931908499,1.56300295340686));
#75316=CARTESIAN_POINT('Ctrl Pts',(3.92787635503417,5.81602462338885,1.53718748372424));
#75317=CARTESIAN_POINT('Ctrl Pts',(4.18197629092144,5.63608334722262,1.52293114114716));
#75318=CARTESIAN_POINT('Ctrl Pts',(4.73019815009442,5.19031032768737,1.49085352556271));
#75319=CARTESIAN_POINT('Ctrl Pts',(5.01543714730117,4.91523052639097,1.47319127530002));
#75320=CARTESIAN_POINT('Ctrl Pts',(5.4040528509735,4.47120451168982,1.44674285207172));
#75321=CARTESIAN_POINT('Ctrl Pts',(5.52600220610544,4.31957805856301,1.43801089281206));
#75322=CARTESIAN_POINT('Ctrl Pts',(5.79602963515161,3.95365756666718,1.41735159340973));
#75323=CARTESIAN_POINT('Ctrl Pts',(5.93878852624269,3.73579385192775,1.40536673500222));
#75324=CARTESIAN_POINT('Ctrl Pts',(6.217113782653,3.25461347645448,1.37979016067684));
#75325=CARTESIAN_POINT('Ctrl Pts',(6.34879583875365,2.98961688460007,1.36623096200207));
#75326=CARTESIAN_POINT('Ctrl Pts',(6.55710077293798,2.49410679385626,1.34179868138937));
#75327=CARTESIAN_POINT('Ctrl Pts',(6.6392410051092,2.2664114793094,1.33089806488089));
#75328=CARTESIAN_POINT('Ctrl Pts',(6.79873075296536,1.74054994326668,1.30623503290395));
#75329=CARTESIAN_POINT('Ctrl Pts',(6.86854119434363,1.44062215947135,1.29253162590189));
#75330=CARTESIAN_POINT('Ctrl Pts',(6.93901190680758,1.01185320266401,1.27291463982902));
#75331=CARTESIAN_POINT('Ctrl Pts',(6.95618993896126,0.88608901596617,1.26714804521847));
#75332=CARTESIAN_POINT('Ctrl Pts',(6.99997323701482,0.48451553450993,1.24867921127313));
#75333=CARTESIAN_POINT('Ctrl Pts',(7.01365072944863,0.207565591087008,1.23589750904888));
#75334=CARTESIAN_POINT('Ctrl Pts',(7.00837627413621,-0.324770476602897,
1.21144199179764));
#75335=CARTESIAN_POINT('Ctrl Pts',(6.99190294887023,-0.579750598249626,
1.19977695961132));
#75336=CARTESIAN_POINT('Ctrl Pts',(6.92380854636316,-1.14864810171334,1.17380034313954));
#75337=CARTESIAN_POINT('Ctrl Pts',(6.86467056097649,-1.46110209823195,1.15957432486484));
#75338=CARTESIAN_POINT('Ctrl Pts',(6.72514814806198,-1.99636505123688,1.13479810361725));
#75339=CARTESIAN_POINT('Ctrl Pts',(6.6543009970792,-2.221118206933,1.12425877640029));
#75340=CARTESIAN_POINT('Ctrl Pts',(6.51576150794132,-2.59399563783087,1.10621865276002));
#75341=CARTESIAN_POINT('Ctrl Pts',(6.45397931128989,-2.74410468677476,1.09878904586431));
#75342=CARTESIAN_POINT('Ctrl Pts',(6.19887618598403,-3.30751887337305,1.0703796101476));
#75343=CARTESIAN_POINT('Ctrl Pts',(5.97058761211762,-3.703761406826,1.04937976319834));
#75344=CARTESIAN_POINT('Ctrl Pts',(5.53560492813307,-4.31278069371356,1.01546062965234));
#75345=CARTESIAN_POINT('Ctrl Pts',(5.35108519743545,-4.5397015208267,1.00236202317304));
#75346=CARTESIAN_POINT('Ctrl Pts',(4.98326101475976,-4.93835500990896,0.978065917075798));
#75347=CARTESIAN_POINT('Ctrl Pts',(4.80385596417464,-5.11304262589715,0.966879410479455));
#75348=CARTESIAN_POINT('Ctrl Pts',(4.5014235621914,-5.37752532508763,0.948668903431823));
#75349=CARTESIAN_POINT('Ctrl Pts',(4.38414420895216,-5.47356103972028,0.941738102653115));
#75350=CARTESIAN_POINT('Ctrl Pts',(4.08111497310209,-5.70570903579223,0.924213992744855));
#75351=CARTESIAN_POINT('Ctrl Pts',(3.89159880535497,-5.83661494977194,0.913603035218845));
#75352=CARTESIAN_POINT('Ctrl Pts',(3.48745112933642,-6.08732565936716,0.891767238045576));
#75353=CARTESIAN_POINT('Ctrl Pts',(3.27226412748057,-6.20565386843528,0.880564244524344));
#75354=CARTESIAN_POINT('Ctrl Pts',(2.7845335893355,-6.44141293850014,0.85601515254437));
#75355=CARTESIAN_POINT('Ctrl Pts',(2.50984486143492,-6.55332817754673,0.842735694799498));
#75356=CARTESIAN_POINT('Ctrl Pts',(1.983661245951,-6.72975609073621,0.817877494194208));
#75357=CARTESIAN_POINT('Ctrl Pts',(1.73406594405275,-6.79834832786492,0.806312481595107));
#75358=CARTESIAN_POINT('Ctrl Pts',(1.28669542541168,-6.89504636326368,0.785531617432516));
#75359=CARTESIAN_POINT('Ctrl Pts',(1.0904332236139,-6.92879518929464,0.776394530482349));
#75360=CARTESIAN_POINT('Ctrl Pts',(0.52956158706368,-7.00081852693867,0.750388408331139));
#75361=CARTESIAN_POINT('Ctrl Pts',(0.163011828899802,-7.01892666715469,
0.733544461211931));
#75362=CARTESIAN_POINT('Ctrl Pts',(-0.459091340103273,-7.00088276558127,
0.70526777664876));
#75363=CARTESIAN_POINT('Ctrl Pts',(-0.714313479005114,-6.97946157114112,
0.693746958941813));
#75364=CARTESIAN_POINT('Ctrl Pts',(-1.24394001082276,-6.90564819119305,
0.669762296487304));
#75365=CARTESIAN_POINT('Ctrl Pts',(-1.51754068417451,-6.8507248734772,0.657328439064246));
#75366=CARTESIAN_POINT('Ctrl Pts',(-1.90905962857967,-6.74751918273071,
0.639061742462014));
#75367=CARTESIAN_POINT('Ctrl Pts',(-2.03008692504151,-6.71209878603812,
0.633339548630402));
#75368=CARTESIAN_POINT('Ctrl Pts',(-2.44175009212672,-6.57946629418827,
0.61357881644767));
#75369=CARTESIAN_POINT('Ctrl Pts',(-2.72693222177506,-6.46647975880543,
0.599429740775669));
#75370=CARTESIAN_POINT('Ctrl Pts',(-3.22454520072293,-6.23053887926962,
0.574142576554722));
#75371=CARTESIAN_POINT('Ctrl Pts',(-3.43966601976377,-6.11440982550656,
0.562989124960971));
#75372=CARTESIAN_POINT('Ctrl Pts',(-3.81618798289243,-5.88498028555875,
0.543006541645807));
#75373=CARTESIAN_POINT('Ctrl Pts',(-3.97971107958816,-5.7756544989867,0.534155795878401));
#75374=CARTESIAN_POINT('Ctrl Pts',(-4.3558787901782,-5.5005923601428,0.513244021840513));
#75375=CARTESIAN_POINT('Ctrl Pts',(-4.56398686139376,-5.32918554740747,
0.501228754710601));
#75376=CARTESIAN_POINT('Ctrl Pts',(-4.85889269374257,-5.05631458197018,
0.483138362108514));
#75377=CARTESIAN_POINT('Ctrl Pts',(-4.95350243808937,-4.96366482040794,
0.477147569826183));
#75378=CARTESIAN_POINT('Ctrl Pts',(-5.13437554873011,-4.77621415676932,
0.465268085802562));
#75379=CARTESIAN_POINT('Ctrl Pts',(-5.22077473879689,-4.68161772997975,
0.459393220794168));
#75380=CARTESIAN_POINT('Ctrl Pts',(-5.58263483472045,-4.26294358824424,
0.43396165710622));
#75381=CARTESIAN_POINT('Ctrl Pts',(-5.83089024532003,-3.91653328043703,
0.414399752780401));
#75382=CARTESIAN_POINT('Ctrl Pts',(-6.09739427006168,-3.46260381604466,
0.390526191683218));
#75383=CARTESIAN_POINT('Ctrl Pts',(-6.1466760514654,-3.37434672637,0.385956771612364));
#75384=CARTESIAN_POINT('Ctrl Pts',(-6.30204945332605,-3.08138722638288,
0.371003577210365));
#75385=CARTESIAN_POINT('Ctrl Pts',(-6.39995552547464,-2.8725154476415,0.360682872803395));
#75386=CARTESIAN_POINT('Ctrl Pts',(-6.57444378949163,-2.44683317023401,
0.340073643603738));
#75387=CARTESIAN_POINT('Ctrl Pts',(-6.65101183465584,-2.23032335448553,
0.329797065975353));
#75388=CARTESIAN_POINT('Ctrl Pts',(-6.76540054318372,-1.8481563762227,0.311701115082449));
#75389=CARTESIAN_POINT('Ctrl Pts',(-6.8080794005409,-1.68415538730638,0.303940974934625));
#75390=CARTESIAN_POINT('Ctrl Pts',(-6.93962976274809,-1.09128687920283,
0.276039159265955));
#75391=CARTESIAN_POINT('Ctrl Pts',(-6.99423014699099,-0.655842069030141,
0.25589408105819));
#75392=CARTESIAN_POINT('Ctrl Pts',(-7.0109706278193,-0.118077221317558,
0.231504526978879));
#75393=CARTESIAN_POINT('Ctrl Pts',(-7.01194192434386,-0.0179459306536899,
0.226980140501383));
#75394=CARTESIAN_POINT('Ctrl Pts',(-7.00804521914173,0.314512647529299,
0.211994204451907));
#75395=CARTESIAN_POINT('Ctrl Pts',(-6.99377388525388,0.546574713582783,
0.201596821116923));
#75396=CARTESIAN_POINT('Ctrl Pts',(-6.94438043931484,0.989241965167925,
0.181643537258381));
#75397=CARTESIAN_POINT('Ctrl Pts',(-6.91111505020142,1.19979400991379,0.172098775150825));
#75398=CARTESIAN_POINT('Ctrl Pts',(-6.84595513888636,1.51753526881411,0.157393470294117));
#75399=CARTESIAN_POINT('Ctrl Pts',(-6.82100244102319,1.62601963603786,0.152312659542052));
#75400=CARTESIAN_POINT('Ctrl Pts',(-6.75160255402251,1.89793664833274,0.139444578944936));
#75401=CARTESIAN_POINT('Ctrl Pts',(-6.70379667449445,2.0604392966348,0.131635618956626));
#75402=CARTESIAN_POINT('Ctrl Pts',(-6.62541859343733,2.29511491041281,0.120224315696719));
#75403=CARTESIAN_POINT('Ctrl Pts',(-6.59945212357222,2.36874444689044,0.116624014189679));
#75404=CARTESIAN_POINT('Ctrl Pts',(-6.57226803330854,2.44190897882182,0.113027768592106));
#75405=CARTESIAN_POINT('Ctrl Pts',(-6.57226796657889,2.44190915842114,0.660259531491259));
#75406=CARTESIAN_POINT('Ctrl Pts',(-6.61936822038628,2.315141343063,0.666482247053822));
#75407=CARTESIAN_POINT('Ctrl Pts',(-6.66280048077769,2.18701158570925,0.672704323074592));
#75408=CARTESIAN_POINT('Ctrl Pts',(-6.76042717422472,1.86901087077713,0.687967745466177));
#75409=CARTESIAN_POINT('Ctrl Pts',(-6.81035720103147,1.67797906830669,0.696981790108703));
#75410=CARTESIAN_POINT('Ctrl Pts',(-6.93827667256961,1.08776383334722,0.724403037241743));
#75411=CARTESIAN_POINT('Ctrl Pts',(-6.98966943009966,0.683695560157103,
0.742546829547995));
#75412=CARTESIAN_POINT('Ctrl Pts',(-7.01318344917094,0.0899608285585705,
0.769185932077584));
#75413=CARTESIAN_POINT('Ctrl Pts',(-7.01307905937192,-0.097751731837338,
0.777614190741723));
#75414=CARTESIAN_POINT('Ctrl Pts',(-6.99508835007367,-0.539614474412561,
0.79770720508367));
#75415=CARTESIAN_POINT('Ctrl Pts',(-6.97088291521988,-0.793242383565875,
0.809428378410608));
#75416=CARTESIAN_POINT('Ctrl Pts',(-6.88843545187471,-1.34023746984631,
0.834881134791783));
#75417=CARTESIAN_POINT('Ctrl Pts',(-6.82511734801832,-1.63234732784954,
0.848579118604667));
#75418=CARTESIAN_POINT('Ctrl Pts',(-6.67614967385812,-2.15567478138416,
0.873313457990113));
#75419=CARTESIAN_POINT('Ctrl Pts',(-6.59657233599127,-2.38812575784159,
0.884376783898336));
#75420=CARTESIAN_POINT('Ctrl Pts',(-6.41922320370544,-2.8291359735642,0.905708877608907));
#75421=CARTESIAN_POINT('Ctrl Pts',(-6.32305169926817,-3.03800158252752,
0.91597138101971));
#75422=CARTESIAN_POINT('Ctrl Pts',(-6.14659171595843,-3.37640232553529,
0.933113913625399));
#75423=CARTESIAN_POINT('Ctrl Pts',(-6.07203166188136,-3.50871960366765,
0.939958145794952));
#75424=CARTESIAN_POINT('Ctrl Pts',(-5.86455968270675,-3.8504604144153,0.958151611574397));
#75425=CARTESIAN_POINT('Ctrl Pts',(-5.72473384552216,-4.05543164861286,
0.969569682469305));
#75426=CARTESIAN_POINT('Ctrl Pts',(-5.38708352780995,-4.49803064641249,
0.995182915034166));
#75427=CARTESIAN_POINT('Ctrl Pts',(-5.18380813011305,-4.73086544284331,
1.00933743455038));
#75428=CARTESIAN_POINT('Ctrl Pts',(-4.67558223594547,-5.24076520041791,
1.04202846822909));
#75429=CARTESIAN_POINT('Ctrl Pts',(-4.36026230076107,-5.50588837385504,
1.06037448841543));
#75430=CARTESIAN_POINT('Ctrl Pts',(-3.87207580808598,-5.84797885991537,
1.08710191118593));
#75431=CARTESIAN_POINT('Ctrl Pts',(-3.71648496687771,-5.9480724317828,1.09541051428432));
#75432=CARTESIAN_POINT('Ctrl Pts',(-3.33988855493214,-6.16979077412279,
1.11526821476839));
#75433=CARTESIAN_POINT('Ctrl Pts',(-3.11591821679655,-6.28587501970539,
1.12687294108092));
#75434=CARTESIAN_POINT('Ctrl Pts',(-2.61291044936449,-6.51308241471437,
1.15226926876994));
#75435=CARTESIAN_POINT('Ctrl Pts',(-2.33199250240424,-6.61886393100552,
1.16602690499378));
#75436=CARTESIAN_POINT('Ctrl Pts',(-1.81089882002314,-6.77777660847228,
1.19079253406406));
#75437=CARTESIAN_POINT('Ctrl Pts',(-1.573049494107,-6.83689465731812,1.20182917749871));
#75438=CARTESIAN_POINT('Ctrl Pts',(-1.03084935256075,-6.94186122754047,
1.22661480723018));
#75439=CARTESIAN_POINT('Ctrl Pts',(-0.725595226018135,-6.98037216848192,
1.24030642864799));
#75440=CARTESIAN_POINT('Ctrl Pts',(-0.292014700059731,-7.00631766596057,
1.25991751660996));
#75441=CARTESIAN_POINT('Ctrl Pts',(-0.165045143543451,-7.01045782870972,
1.26568962695711));
#75442=CARTESIAN_POINT('Ctrl Pts',(0.238693467207839,-7.01264802599733,
1.28415035480813));
#75443=CARTESIAN_POINT('Ctrl Pts',(0.515266268549994,-6.99776443004944,
1.29691748561911));
#75444=CARTESIAN_POINT('Ctrl Pts',(1.04346536383209,-6.93784967375325,1.32133664779025));
#75445=CARTESIAN_POINT('Ctrl Pts',(1.29494606342271,-6.89533875000542,1.33298009214175));
#75446=CARTESIAN_POINT('Ctrl Pts',(1.84866222491564,-6.77036970411805,1.35871509899302));
#75447=CARTESIAN_POINT('Ctrl Pts',(2.1488205305843,-6.68116997282315,1.37272688720449));
#75448=CARTESIAN_POINT('Ctrl Pts',(2.67319084871069,-6.48633136884539,1.39778278828183));
#75449=CARTESIAN_POINT('Ctrl Pts',(2.89966422100529,-6.38830083873669,1.40881530300481));
#75450=CARTESIAN_POINT('Ctrl Pts',(3.28135669597843,-6.19859599839696,1.42816014400196));
#75451=CARTESIAN_POINT('Ctrl Pts',(3.43908184739036,-6.11249606713499,1.43639624344593));
#75452=CARTESIAN_POINT('Ctrl Pts',(3.95447280276339,-5.80488272126014,1.46398870568754));
#75453=CARTESIAN_POINT('Ctrl Pts',(4.29550328604515,-5.55726408383358,1.48333310074313));
#75454=CARTESIAN_POINT('Ctrl Pts',(4.68765706420252,-5.21474000877471,1.50694859177633));
#75455=CARTESIAN_POINT('Ctrl Pts',(4.76161352378925,-5.14729822295721,1.51147318897595));
#75456=CARTESIAN_POINT('Ctrl Pts',(5.00185371129468,-4.91861021400595,1.52642990714244));
#75457=CARTESIAN_POINT('Ctrl Pts',(5.16159132140603,-4.7507097600355,1.5367973026684));
#75458=CARTESIAN_POINT('Ctrl Pts',(5.46258012305145,-4.40120212931766,1.55745765299244));
#75459=CARTESIAN_POINT('Ctrl Pts',(5.6037917062938,-4.21993806318362,1.56773860539465));
#75460=CARTESIAN_POINT('Ctrl Pts',(5.83129670770962,-3.89629954326537,1.5856834502393));
#75461=CARTESIAN_POINT('Ctrl Pts',(5.92188903016706,-3.75717976725567,1.5932846164083));
#75462=CARTESIAN_POINT('Ctrl Pts',(6.23839646056179,-3.23120029089253,1.62148845238909));
#75463=CARTESIAN_POINT('Ctrl Pts',(6.4320345802714,-2.82616238410946,1.64210299742816));
#75464=CARTESIAN_POINT('Ctrl Pts',(6.62010692382887,-2.31124717132462,1.66695278150905));
#75465=CARTESIAN_POINT('Ctrl Pts',(6.65248120535126,-2.21634230563035,1.671483331566));
#75466=CARTESIAN_POINT('Ctrl Pts',(6.75347201079601,-1.89810855152635,1.6865316777584));
#75467=CARTESIAN_POINT('Ctrl Pts',(6.81296227369022,-1.67204857049558,1.69698455267594));
#75468=CARTESIAN_POINT('Ctrl Pts',(6.9051213163183,-1.23399207133201,1.71703715294312));
#75469=CARTESIAN_POINT('Ctrl Pts',(6.93957093184892,-1.02263856339566,1.72662554848845));
#75470=CARTESIAN_POINT('Ctrl Pts',(6.98238237215309,-0.654570222906499,
1.74342556754275));
#75471=CARTESIAN_POINT('Ctrl Pts',(6.99525443619507,-0.498537135387838,
1.75058753721644));
#75472=CARTESIAN_POINT('Ctrl Pts',(7.010322312855,-0.190189817221909,1.76476366493551));
#75473=CARTESIAN_POINT('Ctrl Pts',(7.0127989560457,-0.0379708568626089,
1.77177198096467));
#75474=CARTESIAN_POINT('Ctrl Pts',(7.00590491700599,0.385200883853832,1.79123813732939));
#75475=CARTESIAN_POINT('Ctrl Pts',(6.9857803295653,0.655713888114175,1.80365465089155));
#75476=CARTESIAN_POINT('Ctrl Pts',(6.91653182200668,1.17636325315985,1.8275194242353));
#75477=CARTESIAN_POINT('Ctrl Pts',(6.86933868967801,1.42633519478744,1.83896357813441));
#75478=CARTESIAN_POINT('Ctrl Pts',(6.74271737357749,1.94159115104607,1.8627630149837));
#75479=CARTESIAN_POINT('Ctrl Pts',(6.66094840059031,2.20585078870684,1.87508905047707));
#75480=CARTESIAN_POINT('Ctrl Pts',(6.5190987862986,2.5836303826207,1.89328823747418));
#75481=CARTESIAN_POINT('Ctrl Pts',(6.47117247103299,2.70142944935583,1.89905634554082));
#75482=CARTESIAN_POINT('Ctrl Pts',(6.29613598649128,3.10022366737014,1.91894843544529));
#75483=CARTESIAN_POINT('Ctrl Pts',(6.15370994481535,3.37410263845989,1.93318482723096));
#75484=CARTESIAN_POINT('Ctrl Pts',(5.86655379879665,3.84723856177491,1.95859309166131));
#75485=CARTESIAN_POINT('Ctrl Pts',(5.72848814684077,4.04995369789045,1.96978083621134));
#75486=CARTESIAN_POINT('Ctrl Pts',(5.39881645172317,4.48330749652224,1.99445368730968));
#75487=CARTESIAN_POINT('Ctrl Pts',(5.20246590427389,4.7097364255845,2.00786845093655));
#75488=CARTESIAN_POINT('Ctrl Pts',(4.81460842040578,5.10305536796147,2.03261045289571));
#75489=CARTESIAN_POINT('Ctrl Pts',(4.62735880958025,5.27344050435344,2.04392482673201));
#75490=CARTESIAN_POINT('Ctrl Pts',(4.28719831610805,5.55086859526103,2.06385042962107));
#75491=CARTESIAN_POINT('Ctrl Pts',(4.13846411214626,5.66262521653732,2.07238095550425));
#75492=CARTESIAN_POINT('Ctrl Pts',(3.64863908404127,6.00105580070087,2.09975642510544));
#75493=CARTESIAN_POINT('Ctrl Pts',(3.29206724194482,6.20383301847566,2.11858113930592));
#75494=CARTESIAN_POINT('Ctrl Pts',(2.82886856279303,6.4160066621223,2.14169311823062));
#75495=CARTESIAN_POINT('Ctrl Pts',(2.73701484019737,6.45572527565513,2.14621783153879));
#75496=CARTESIAN_POINT('Ctrl Pts',(2.53837369202448,6.53661816842051,2.15589114260135));
#75497=CARTESIAN_POINT('Ctrl Pts',(2.43136442889559,6.57717153160591,2.16103457980988));
#75498=CARTESIAN_POINT('Ctrl Pts',(2.06677022413769,6.70522755816935,2.17837491338701));
#75499=CARTESIAN_POINT('Ctrl Pts',(1.80510395581976,6.78035497916357,2.19050677621098));
#75500=CARTESIAN_POINT('Ctrl Pts',(1.41217581221567,6.86880504155568,2.20864697954383));
#75501=CARTESIAN_POINT('Ctrl Pts',(1.28383841713066,6.89394528751383,2.21456589966175));
#75502=CARTESIAN_POINT('Ctrl Pts',(1.02805676988242,6.93666032647216,2.22639567796045));
#75503=CARTESIAN_POINT('Ctrl Pts',(0.900683769950669,6.9543457959294,2.23229418558519));
#75504=CARTESIAN_POINT('Ctrl Pts',(0.350565115262764,7.01536098208177,2.25773672936224));
#75505=CARTESIAN_POINT('Ctrl Pts',(-0.0751629981528878,7.02371344715437,
2.27728272193942));
#75506=CARTESIAN_POINT('Ctrl Pts',(-0.80261055115844,6.97180582807092,2.31035747959763));
#75507=CARTESIAN_POINT('Ctrl Pts',(-1.10446594334541,6.93039819291771,2.32400196811033));
#75508=CARTESIAN_POINT('Ctrl Pts',(-1.64609895777159,6.81980274987345,2.34876344590875));
#75509=CARTESIAN_POINT('Ctrl Pts',(-1.88670363915619,6.75719596037491,2.35987122714874));
#75510=CARTESIAN_POINT('Ctrl Pts',(-2.26830368167821,6.63592640849457,2.37801947398393));
#75511=CARTESIAN_POINT('Ctrl Pts',(-2.41159680567609,6.58520462257227,2.3849694346356));
#75512=CARTESIAN_POINT('Ctrl Pts',(-2.76675639064031,6.44634010168383,2.40247500024569));
#75513=CARTESIAN_POINT('Ctrl Pts',(-2.9761596105,6.35237876013932,2.41304764497562));
#75514=CARTESIAN_POINT('Ctrl Pts',(-3.39946457423003,6.13690408246136,2.43485441723145));
#75515=CARTESIAN_POINT('Ctrl Pts',(-3.61234605431573,6.01405940181746,2.44606627064762));
#75516=CARTESIAN_POINT('Ctrl Pts',(-4.06844913358781,5.71789087354352,2.47070937757767));
#75517=CARTESIAN_POINT('Ctrl Pts',(-4.30793992709884,5.53969416749828,2.48407201280389));
#75518=CARTESIAN_POINT('Ctrl Pts',(-4.73004461640136,5.18164827813524,2.50886414163479));
#75519=CARTESIAN_POINT('Ctrl Pts',(-4.91556327632237,5.00599984984363,2.52028047616279));
#75520=CARTESIAN_POINT('Ctrl Pts',(-5.22069421682454,4.68374987365058,2.54042726024354));
#75521=CARTESIAN_POINT('Ctrl Pts',(-5.34472780304034,4.5417005268804,2.54907554572099));
#75522=CARTESIAN_POINT('Ctrl Pts',(-5.71684159521833,4.0791535412962,2.57637391166004));
#75523=CARTESIAN_POINT('Ctrl Pts',(-5.94296471403411,3.74205216656131,2.59500086617898));
#75524=CARTESIAN_POINT('Ctrl Pts',(-6.23407490378244,3.21448295770506,2.62233697489158));
#75525=CARTESIAN_POINT('Ctrl Pts',(-6.32210011202131,3.03770346464745,2.63123157730135));
#75526=CARTESIAN_POINT('Ctrl Pts',(-6.46356288804325,2.72073401664894,2.64681712099078));
#75527=CARTESIAN_POINT('Ctrl Pts',(-6.52016167747087,2.5821504437946,2.65351582122961));
#75528=CARTESIAN_POINT('Ctrl Pts',(-6.57226793021667,2.4419092562881,2.66021763119828));
#75529=CARTESIAN_POINT('Origin',(0.,0.,10.));
#75530=CARTESIAN_POINT('',(-6.57226799596304,2.44190907933527,4.66030144016832));
#75531=CARTESIAN_POINT('',(-6.57269630323124,2.4420685397187,4.11322495262288));
#75532=CARTESIAN_POINT('',(-6.57226799596304,2.44190907933527,10.));
#75533=CARTESIAN_POINT('',(-7.01180849524368,2.69103457778642E-5,2.22648654173946));
#75534=CARTESIAN_POINT('Ctrl Pts',(-6.57269630323124,2.4420685397187,4.11322495262288));
#75535=CARTESIAN_POINT('Ctrl Pts',(-6.20535467906786,3.42842235222112,4.0654299812279));
#75536=CARTESIAN_POINT('Ctrl Pts',(-4.95782740744273,5.33202724196766,3.96470380932042));
#75537=CARTESIAN_POINT('Ctrl Pts',(-1.91930106773404,7.05226072421662,3.81104643690041));
#75538=CARTESIAN_POINT('Ctrl Pts',(1.68861748831434,7.11102446149387,3.65225283536289));
#75539=CARTESIAN_POINT('Ctrl Pts',(4.88493970070459,5.43649354182164,3.49345923382538));
#75540=CARTESIAN_POINT('Ctrl Pts',(6.89056992096269,2.43683074440551,3.33466563228786));
#75541=CARTESIAN_POINT('Ctrl Pts',(7.21664073544971,-1.15680353300375,3.17587203075035));
#75542=CARTESIAN_POINT('Ctrl Pts',(5.78367318632997,-4.46846980083332,3.01707842921281));
#75543=CARTESIAN_POINT('Ctrl Pts',(2.94094957949722,-6.69095759537126,2.85828482767533));
#75544=CARTESIAN_POINT('Ctrl Pts',(-0.618623231225066,-7.28254097808985,
2.69949122613779));
#75545=CARTESIAN_POINT('Ctrl Pts',(-4.02740814743654,-6.09902301034318,
2.54069762460028));
#75546=CARTESIAN_POINT('Ctrl Pts',(-6.4374277342472,-3.44768939946999,2.38302243189696));
#75547=CARTESIAN_POINT('Ctrl Pts',(-7.01160457735808,-1.14092551293614,
2.27827843970617));
#75548=CARTESIAN_POINT('Ctrl Pts',(-7.0118447620046,2.59581319030052E-5,
2.22646564802786));
#75549=CARTESIAN_POINT('Ctrl Pts',(-7.01124999987674,4.1574104656346E-5,
2.22680829755206));
#75550=CARTESIAN_POINT('Ctrl Pts',(-7.01124960066053,0.0673672487642149,
2.22375897461869));
#75551=CARTESIAN_POINT('Ctrl Pts',(-7.01027946364388,0.13468844982995,2.2206980026699));
#75552=CARTESIAN_POINT('Ctrl Pts',(-6.99921204821522,0.518698384756561,
2.20317221559078));
#75553=CARTESIAN_POINT('Ctrl Pts',(-6.96862589450747,0.834427695950238,
2.18854167333345));
#75554=CARTESIAN_POINT('Ctrl Pts',(-6.88439660075787,1.34235720129083,2.16490095114753));
#75555=CARTESIAN_POINT('Ctrl Pts',(-6.84373919639515,1.53625353620252,2.15584663781379));
#75556=CARTESIAN_POINT('Ctrl Pts',(-6.74359093682043,1.93002273684355,2.1373776599019));
#75557=CARTESIAN_POINT('Ctrl Pts',(-6.6832839369519,2.12948920324959,2.12797811415362));
#75558=CARTESIAN_POINT('Ctrl Pts',(-6.60055197415375,2.36474718119154,2.11677107083992));
#75559=CARTESIAN_POINT('Ctrl Pts',(-6.58657864775301,2.40339272323902,2.11492597067985));
#75560=CARTESIAN_POINT('Ctrl Pts',(-6.57226800353884,2.44190905894539,2.1130822547889));
#75561=CARTESIAN_POINT('',(-7.01124999997673,-1.80655468318879E-5,2.77353435691037));
#75562=CARTESIAN_POINT('Ctrl Pts',(-6.57226793021667,2.4419092562881,2.66021763119828));
#75563=CARTESIAN_POINT('Ctrl Pts',(-6.63825067143893,2.26432024352436,2.66870420947979));
#75564=CARTESIAN_POINT('Ctrl Pts',(-6.69702941724246,2.08407313392669,2.67719508029717));
#75565=CARTESIAN_POINT('Ctrl Pts',(-6.78370868773811,1.77646480852692,2.69164819243435));
#75566=CARTESIAN_POINT('Ctrl Pts',(-6.81548338591757,1.65036835490453,2.69757167026797));
#75567=CARTESIAN_POINT('Ctrl Pts',(-6.88364107724175,1.34418898412278,2.71193582834949));
#75568=CARTESIAN_POINT('Ctrl Pts',(-6.91648900616039,1.16341643458372,2.72039248230661));
#75569=CARTESIAN_POINT('Ctrl Pts',(-6.97028931756841,0.782908825344512,
2.73807246531727));
#75570=CARTESIAN_POINT('Ctrl Pts',(-6.98983768873121,0.58313790210834,2.74728572145898));
#75571=CARTESIAN_POINT('Ctrl Pts',(-7.00776269506336,0.255320933964559,
2.76228116211942));
#75572=CARTESIAN_POINT('Ctrl Pts',(-7.0112500449107,0.127671648310814,2.76809066635348));
#75573=CARTESIAN_POINT('Ctrl Pts',(-7.01124999999957,-2.4663037176062E-6,
2.7738784608769));
#75574=CARTESIAN_POINT('Ctrl Pts',(-7.01124999997673,-1.80655468318879E-5,
2.77353435691037));
#75575=CARTESIAN_POINT('Ctrl Pts',(-7.01124950890869,-0.190601875733761,
2.7821841598315));
#75576=CARTESIAN_POINT('Ctrl Pts',(-7.00347383924979,-0.381166330084032,
2.79083396275264));
#75577=CARTESIAN_POINT('Ctrl Pts',(-6.98795373149948,-0.571077235514203,
2.79948376567377));
#75578=CARTESIAN_POINT('Ctrl Pts',(-6.97242834684876,-0.761052711432532,
2.80813650956344));
#75579=CARTESIAN_POINT('Ctrl Pts',(-6.94915328487888,-0.950373907584441,
2.81678925345311));
#75580=CARTESIAN_POINT('Ctrl Pts',(-6.91821124521096,-1.13841105455658,
2.82544199734278));
#75581=CARTESIAN_POINT('Ctrl Pts',(-6.88859135868876,-1.31841337551048,
2.83372500954457));
#75582=CARTESIAN_POINT('Ctrl Pts',(-6.85194608979608,-1.49723885436048,
2.84200802174635));
#75583=CARTESIAN_POINT('Ctrl Pts',(-6.80839202835472,-1.67434302063106,
2.85029103394815));
#75584=CARTESIAN_POINT('Ctrl Pts',(-6.76353436973175,-1.8567480126883,2.85882196129273));
#75585=CARTESIAN_POINT('Ctrl Pts',(-6.71133454211413,-2.03738050321834,
2.86735288863731));
#75586=CARTESIAN_POINT('Ctrl Pts',(-6.65195766392592,-2.21564568463399,
2.8758838159819));
#75587=CARTESIAN_POINT('Ctrl Pts',(-6.59259205836282,-2.39387702263074,
2.88441312374073));
#75588=CARTESIAN_POINT('Ctrl Pts',(-6.52605221807238,-2.56974165801549,
2.89294243149957));
#75589=CARTESIAN_POINT('Ctrl Pts',(-6.45255285871369,-2.74266078252594,
2.9014717392584));
#75590=CARTESIAN_POINT('Ctrl Pts',(-6.37527539811279,-2.92446850096178,
2.91043948061067));
#75591=CARTESIAN_POINT('Ctrl Pts',(-6.29030421808319,-3.10301957578802,
2.91940722196295));
#75592=CARTESIAN_POINT('Ctrl Pts',(-6.19794623826995,-3.27766517356722,
2.92837496331522));
#75593=CARTESIAN_POINT('Ctrl Pts',(-6.11010648638776,-3.4437669658245,2.93690399542397));
#75594=CARTESIAN_POINT('Ctrl Pts',(-6.01558555232828,-3.60633597361661,
2.94543302753274));
#75595=CARTESIAN_POINT('Ctrl Pts',(-5.91469479125556,-3.76483891936884,
2.95396205964149));
#75596=CARTESIAN_POINT('Ctrl Pts',(-5.81380302100902,-3.92334345056876,
2.96249117706308));
#75597=CARTESIAN_POINT('Ctrl Pts',(-5.70654146358684,-4.07778158189161,
2.97102029448466));
#75598=CARTESIAN_POINT('Ctrl Pts',(-5.59326525020323,-4.22764833014396,
2.97954941190625));
#75599=CARTESIAN_POINT('Ctrl Pts',(-5.47996611675168,-4.3775454021152,2.9880802550913));
#75600=CARTESIAN_POINT('Ctrl Pts',(-5.3606500820174,-4.52286899986246,2.99661109827635));
#75601=CARTESIAN_POINT('Ctrl Pts',(-5.23571360583634,-4.66314589093674,
3.0051419414614));
#75602=CARTESIAN_POINT('Ctrl Pts',(-5.21646633694138,-4.6847564495565,3.00645617280282));
#75603=CARTESIAN_POINT('Ctrl Pts',(-5.19708575200059,-4.70624729866498,
3.00777040414424));
#75604=CARTESIAN_POINT('Ctrl Pts',(-5.17757338267325,-4.72761678116294,
3.00908463548566));
#75605=CARTESIAN_POINT('Ctrl Pts',(-5.05091485599362,-4.86633018514231,
3.0176155628491));
#75606=CARTESIAN_POINT('Ctrl Pts',(-4.91865699422918,-4.999974402369,3.02614649021254));
#75607=CARTESIAN_POINT('Ctrl Pts',(-4.78122936540692,-5.12810611413907,
3.03467741757598));
#75608=CARTESIAN_POINT('Ctrl Pts',(-4.64382782704249,-5.25621350026916,
3.04320672535388));
#75609=CARTESIAN_POINT('Ctrl Pts',(-4.50125870411749,-5.37881026070913,
3.05173603313178));
#75610=CARTESIAN_POINT('Ctrl Pts',(-4.35398746275093,-5.49549085493805,
3.06026534090968));
#75611=CARTESIAN_POINT('Ctrl Pts',(-4.1991460108773,-5.61816920305433,3.06923308225247));
#75612=CARTESIAN_POINT('Ctrl Pts',(-4.03910657492292,-5.73430690843164,
3.07820082359527));
#75613=CARTESIAN_POINT('Ctrl Pts',(-3.87444908981545,-5.84348105267128,
3.08716856493806));
#75614=CARTESIAN_POINT('Ctrl Pts',(-3.71784678306701,-5.94731430880328,
3.0956975970661));
#75615=CARTESIAN_POINT('Ctrl Pts',(-3.55706774152558,-6.04484886281997,
3.10422662919414));
#75616=CARTESIAN_POINT('Ctrl Pts',(-3.39264050979283,-6.13576539103416,
3.11275566132219));
#75617=CARTESIAN_POINT('Ctrl Pts',(-3.22821163335349,-6.22668282865376,
3.12128477876308));
#75618=CARTESIAN_POINT('Ctrl Pts',(-3.06013476333635,-6.31098196286659,
3.12981389620397));
#75619=CARTESIAN_POINT('Ctrl Pts',(-2.88896334838836,-6.38838925975623,
3.13834301364486));
#75620=CARTESIAN_POINT('Ctrl Pts',(-2.71775729898345,-6.46581221907227,
3.14687385684908));
#75621=CARTESIAN_POINT('Ctrl Pts',(-2.54345573344074,-6.53634043054176,
3.15540470005329));
#75622=CARTESIAN_POINT('Ctrl Pts',(-2.36663320167697,-6.59974801422147,
3.16393554325751));
#75623=CARTESIAN_POINT('Ctrl Pts',(-2.33939255355957,-6.60951636024482,
3.16524977451273));
#75624=CARTESIAN_POINT('Ctrl Pts',(-2.31209210963559,-6.6191158039643,3.16656400576795));
#75625=CARTESIAN_POINT('Ctrl Pts',(-2.28473400769913,-6.62854562302796,
3.16787823702317));
#75626=CARTESIAN_POINT('Ctrl Pts',(-2.10714731632944,-6.6897563887316,3.1764091643825));
#75627=CARTESIAN_POINT('Ctrl Pts',(-1.92706894792116,-6.74383688423355,
3.18494009174182));
#75628=CARTESIAN_POINT('Ctrl Pts',(-1.74508821395569,-6.79060333755499,
3.19347101910115));
#75629=CARTESIAN_POINT('Ctrl Pts',(-1.5631420287983,-6.83736091232546,3.20200032687489));
#75630=CARTESIAN_POINT('Ctrl Pts',(-1.37929449525701,-6.87680713975774,
3.21052963464864));
#75631=CARTESIAN_POINT('Ctrl Pts',(-1.19414837369101,-6.90880859657518,
3.21905894242239));
#75632=CARTESIAN_POINT('Ctrl Pts',(-0.99948515209662,-6.94245503014401,
3.22802668376725));
#75633=CARTESIAN_POINT('Ctrl Pts',(-0.803386677535188,-6.96787108735875,
3.23699442511211));
#75634=CARTESIAN_POINT('Ctrl Pts',(-0.606564542512081,-6.98496285017087,
3.24596216645697));
#75635=CARTESIAN_POINT('Ctrl Pts',(-0.419371106869084,-7.00121847000559,
3.25449119858084));
#75636=CARTESIAN_POINT('Ctrl Pts',(-0.23152345263966,-7.00994476319048,
3.26302023070472));
#75637=CARTESIAN_POINT('Ctrl Pts',(-0.0436384824191531,-7.01111419428839,
3.27154926282859));
#75638=CARTESIAN_POINT('Ctrl Pts',(0.144248367147679,-7.0122836370837,3.28007838026534));
#75639=CARTESIAN_POINT('Ctrl Pts',(0.332172227240165,-7.00589606808603,
3.28860749770208));
#75640=CARTESIAN_POINT('Ctrl Pts',(0.519516233522091,-6.99197607587491,
3.29713661513882));
#75641=CARTESIAN_POINT('Ctrl Pts',(0.706898146589006,-6.97805326712237,
3.30566745833892));
#75642=CARTESIAN_POINT('Ctrl Pts',(0.89369966620886,-6.95659501469585,3.31419830153901));
#75643=CARTESIAN_POINT('Ctrl Pts',(1.07930819751002,-6.9276778488385,3.32272914473911));
#75644=CARTESIAN_POINT('Ctrl Pts',(1.10790238577609,-6.92322297341414,3.32404337601297));
#75645=CARTESIAN_POINT('Ctrl Pts',(1.13646827454602,-6.9185911723922,3.32535760728684));
#75646=CARTESIAN_POINT('Ctrl Pts',(1.1650036409725,-6.91378283423922,3.3266718385607));
#75647=CARTESIAN_POINT('Ctrl Pts',(1.3502321794825,-6.88257098871993,3.33520276591883));
#75648=CARTESIAN_POINT('Ctrl Pts',(1.53423739686404,-6.84390577530438,3.34373369327696));
#75649=CARTESIAN_POINT('Ctrl Pts',(1.71641388139953,-6.79790776270457,3.35226462063509));
#75650=CARTESIAN_POINT('Ctrl Pts',(1.89855577996322,-6.75191848276841,3.36079392840761));
#75651=CARTESIAN_POINT('Ctrl Pts',(2.07886934176505,-6.698599256705,3.36932323618013));
#75652=CARTESIAN_POINT('Ctrl Pts',(2.2567614335547,-6.63812130007581,3.37785254395265));
#75653=CARTESIAN_POINT('Ctrl Pts',(2.4437977451898,-6.57453458394159,3.38682028529812));
#75654=CARTESIAN_POINT('Ctrl Pts',(2.62815673930782,-6.50303389175604,3.39578802664358));
#75655=CARTESIAN_POINT('Ctrl Pts',(2.80916861474241,-6.42387719811378,3.40475576798904));
#75656=CARTESIAN_POINT('Ctrl Pts',(2.98132524155419,-6.34859291450363,3.41328480011165));
#75657=CARTESIAN_POINT('Ctrl Pts',(3.15045410658541,-6.2663839344867,3.42181383223426));
#75658=CARTESIAN_POINT('Ctrl Pts',(3.31600031773121,-6.17752122257031,3.43034286435687));
#75659=CARTESIAN_POINT('Ctrl Pts',(3.48154818477641,-6.08865762179206,3.43887198179233));
#75660=CARTESIAN_POINT('Ctrl Pts',(3.64351305807532,-5.99314030379713,3.44740109922778));
#75661=CARTESIAN_POINT('Ctrl Pts',(3.80136501676108,-5.89128598625504,3.45593021666324));
#75662=CARTESIAN_POINT('Ctrl Pts',(3.95924891487418,-5.78941105972843,3.46446105986206));
#75663=CARTESIAN_POINT('Ctrl Pts',(4.11301797942921,-5.68119673948677,3.47299190306088));
#75664=CARTESIAN_POINT('Ctrl Pts',(4.26217088908681,-5.56700331190138,3.4815227462597));
#75665=CARTESIAN_POINT('Ctrl Pts',(4.2851488544218,-5.54941107969777,3.4828369775392));
#75666=CARTESIAN_POINT('Ctrl Pts',(4.30801732288761,-5.53167702378405,3.4841512088187));
#75667=CARTESIAN_POINT('Ctrl Pts',(4.33077452839732,-5.51380254875753,3.48546544009821));
#75668=CARTESIAN_POINT('Ctrl Pts',(4.47849591515296,-5.39777590228194,3.49399636745846));
#75669=CARTESIAN_POINT('Ctrl Pts',(4.62157716411522,-5.27578953023405,3.50252729481871));
#75670=CARTESIAN_POINT('Ctrl Pts',(4.75954433094147,-5.14823895369115,3.51105822217896));
#75671=CARTESIAN_POINT('Ctrl Pts',(4.89748530487871,-5.02071259246101,3.51958752995363));
#75672=CARTESIAN_POINT('Ctrl Pts',(5.03031390947706,-4.88762434258184,3.5281168377283));
#75673=CARTESIAN_POINT('Ctrl Pts',(5.15759121336016,-4.74940832508326,3.53664614550298));
#75674=CARTESIAN_POINT('Ctrl Pts',(5.29141097580618,-4.60408756432229,3.54561388684737));
#75675=CARTESIAN_POINT('Ctrl Pts',(5.41909343978606,-4.45309823993976,3.55458162819177));
#75676=CARTESIAN_POINT('Ctrl Pts',(5.54017385785379,-4.29698733850281,3.56354936953617));
#75677=CARTESIAN_POINT('Ctrl Pts',(5.6553309231308,-4.14851350966971,3.57207840166097));
#75678=CARTESIAN_POINT('Ctrl Pts',(5.76451625571569,-3.99540749232178,3.58060743378577));
#75679=CARTESIAN_POINT('Ctrl Pts',(5.86737222757443,-3.83817270398146,3.58913646591057));
#75680=CARTESIAN_POINT('Ctrl Pts',(5.97022922826458,-3.68093634287791,3.59766558334822));
#75681=CARTESIAN_POINT('Ctrl Pts',(6.06675657681249,-3.51957138627459,3.60619470078588));
#75682=CARTESIAN_POINT('Ctrl Pts',(6.15664046272336,-3.35460948178137,3.61472381822353));
#75683=CARTESIAN_POINT('Ctrl Pts',(6.24654253554728,-3.18961419924956,3.62325466142454));
#75684=CARTESIAN_POINT('Ctrl Pts',(6.32979831521891,-3.0210207845251,3.63178550462556));
#75685=CARTESIAN_POINT('Ctrl Pts',(6.40613994976964,-2.84938546119429,3.64031634782657));
#75686=CARTESIAN_POINT('Ctrl Pts',(6.41790086963932,-2.82294393559193,3.64163057909629));
#75687=CARTESIAN_POINT('Ctrl Pts',(6.42949778486097,-2.79643025734872,3.64294481036601));
#75688=CARTESIAN_POINT('Ctrl Pts',(6.44092981658747,-2.76984650482558,3.64425904163573));
#75689=CARTESIAN_POINT('Ctrl Pts',(6.51513732820881,-2.59728626606002,3.65278996899439));
#75690=CARTESIAN_POINT('Ctrl Pts',(6.58241890750733,-2.42171261244503,3.66132089635305));
#75691=CARTESIAN_POINT('Ctrl Pts',(6.64254760027904,-2.24369961013662,3.66985182371172));
#75692=CARTESIAN_POINT('Ctrl Pts',(6.70266487769571,-2.06572040336788,3.67838113148479));
#75693=CARTESIAN_POINT('Ctrl Pts',(6.75563188060559,-1.88530306205903,3.68691043925785));
#75694=CARTESIAN_POINT('Ctrl Pts',(6.80127086794582,-1.70303879677815,3.69543974703092));
#75695=CARTESIAN_POINT('Ctrl Pts',(6.84925584452457,-1.51140556803342,3.70440748837612));
#75696=CARTESIAN_POINT('Ctrl Pts',(6.88913949303587,-1.31773088648166,3.71337522972131));
#75697=CARTESIAN_POINT('Ctrl Pts',(6.92077540079595,-1.1227174240376,3.7223429710665));
#75698=CARTESIAN_POINT('Ctrl Pts',(6.95086365414147,-0.937244179258234,
3.73087200318967));
#75699=CARTESIAN_POINT('Ctrl Pts',(6.97349179898842,-0.750560338373692,
3.73940103531284));
#75700=CARTESIAN_POINT('Ctrl Pts',(6.98858664232417,-0.563279065142881,
3.747930067436));
#75701=CARTESIAN_POINT('Ctrl Pts',(7.00368163664823,-0.375995918604626,
3.75645918487202));
#75702=CARTESIAN_POINT('Ctrl Pts',(7.01124315752175,-0.188115633246701,
3.76498830230804));
#75703=CARTESIAN_POINT('Ctrl Pts',(7.01124999535558,-0.000255198826522087,
3.77351741974405));
#75704=CARTESIAN_POINT('Ctrl Pts',(7.01125683457296,0.187643246871896,3.78204826294344));
#75705=CARTESIAN_POINT('Ctrl Pts',(7.00370593859617,0.375521527399259,3.79057910614282));
#75706=CARTESIAN_POINT('Ctrl Pts',(6.98862821308365,0.562763060080633,3.79910994934221));
#75707=CARTESIAN_POINT('Ctrl Pts',(6.98630539246772,0.591608822785914,3.80042418061922));
#75708=CARTESIAN_POINT('Ctrl Pts',(6.98380403514938,0.620439480036657,3.80173841189623));
#75709=CARTESIAN_POINT('Ctrl Pts',(6.98112436373805,0.649252786303629,3.80305264317324));
#75710=CARTESIAN_POINT('Ctrl Pts',(6.96373010250155,0.836285485229273,3.81158357053279));
#75711=CARTESIAN_POINT('Ctrl Pts',(6.93881229331357,1.02265077585319,3.82011449789233));
#75712=CARTESIAN_POINT('Ctrl Pts',(6.90644629163563,1.20773597414851,3.82864542525188));
#75713=CARTESIAN_POINT('Ctrl Pts',(6.87408643460146,1.3927860342571,3.83717473302585));
#75714=CARTESIAN_POINT('Ctrl Pts',(6.83428125964678,1.57655618552337,3.84570404079981));
#75715=CARTESIAN_POINT('Ctrl Pts',(6.78715753996745,1.75844223395679,3.85423334857377));
#75716=CARTESIAN_POINT('Ctrl Pts',(6.73761151108847,1.9496778042745,3.86320108991852));
#75717=CARTESIAN_POINT('Ctrl Pts',(6.67997480325776,2.13883011750153,3.87216883126327));
#75718=CARTESIAN_POINT('Ctrl Pts',(6.6144550262843,2.32521209092039,3.88113657260802));
#75719=CARTESIAN_POINT('Ctrl Pts',(6.55214053023832,2.50247610618643,3.88966560473209));
#75720=CARTESIAN_POINT('Ctrl Pts',(6.48269593291204,2.67723404533696,3.89819463685616));
#75721=CARTESIAN_POINT('Ctrl Pts',(6.40635031693033,2.84891245552871,3.90672366898024));
#75722=CARTESIAN_POINT('Ctrl Pts',(6.33000393729078,3.02059258295811,3.91525278641716));
#75723=CARTESIAN_POINT('Ctrl Pts',(6.24675652844298,3.18919284141453,3.92378190385409));
#75724=CARTESIAN_POINT('Ctrl Pts',(6.15688465148839,3.35416128872282,3.93231102129102));
#75725=CARTESIAN_POINT('Ctrl Pts',(6.0669945900506,3.5191631153936,3.94084186449131));
#75726=CARTESIAN_POINT('Ctrl Pts',(5.97047753066743,3.68053139474048,3.9493727076916));
#75727=CARTESIAN_POINT('Ctrl Pts',(5.86765560344639,3.83773947550433,3.95790355089189));
#75728=CARTESIAN_POINT('Ctrl Pts',(5.85181522411612,3.86195839164787,3.95921778216485));
#75729=CARTESIAN_POINT('Ctrl Pts',(5.83582529391221,3.88607862615853,3.9605320134378));
#75730=CARTESIAN_POINT('Ctrl Pts',(5.81968708264017,3.91009831368102,3.96184624471076));
#75731=CARTESIAN_POINT('Ctrl Pts',(5.71493085677523,4.06601471413551,3.97037717206993));
#75732=CARTESIAN_POINT('Ctrl Pts',(5.60388731357084,4.217745562263,3.97890809942909));
#75733=CARTESIAN_POINT('Ctrl Pts',(5.48691575044627,4.36478889638487,3.98743902678826));
#75734=CARTESIAN_POINT('Ctrl Pts',(5.36996639422247,4.51180431451893,3.99596833456184));
#75735=CARTESIAN_POINT('Ctrl Pts',(5.24709145452818,4.65413375504888,4.00449764233543));
#75736=CARTESIAN_POINT('Ctrl Pts',(5.11869131816443,4.79130731135545,4.01302695010901));
#75737=CARTESIAN_POINT('Ctrl Pts',(4.98369100604868,4.93553202512795,4.02199469145395));
#75738=CARTESIAN_POINT('Ctrl Pts',(4.84258274711559,5.07405656068499,4.03096243279889));
#75739=CARTESIAN_POINT('Ctrl Pts',(4.69587756928842,5.20637689922213,4.03993017414383));
#75740=CARTESIAN_POINT('Ctrl Pts',(4.55634932842262,5.33222401886917,4.04845920626751));
#75741=CARTESIAN_POINT('Ctrl Pts',(4.41175893808063,5.45245924004647,4.0569882383912));
#75742=CARTESIAN_POINT('Ctrl Pts',(4.26258191820052,5.56668859854133,4.06551727051488));
#75743=CARTESIAN_POINT('Ctrl Pts',(4.1134034061561,5.68091909963155,4.07404638795142));
#75744=CARTESIAN_POINT('Ctrl Pts',(3.95963841797951,5.78914343441517,4.08257550538796));
#75745=CARTESIAN_POINT('Ctrl Pts',(3.80179387437706,5.89100924284193,4.0911046228245));
#75746=CARTESIAN_POINT('Ctrl Pts',(3.64391739284751,5.99289566257834,4.09963546602441));
#75747=CARTESIAN_POINT('Ctrl Pts',(3.48195996501132,6.08842082102823,4.10816630922431));
#75748=CARTESIAN_POINT('Ctrl Pts',(3.3164564270066,6.17727636829264,4.11669715242422));
#75749=CARTESIAN_POINT('Ctrl Pts',(3.29095954227667,6.19096513696506,4.1180113836989));
#75750=CARTESIAN_POINT('Ctrl Pts',(3.2653785451568,6.20449570123017,4.11932561497359));
#75751=CARTESIAN_POINT('Ctrl Pts',(3.23971544313659,6.2178670305823,4.12063984624828));
#75752=CARTESIAN_POINT('Ctrl Pts',(3.07313132406655,6.30466289490009,4.12917077360755));
#75753=CARTESIAN_POINT('Ctrl Pts',(2.90302863634734,6.38477528091143,4.13770170096682));
#75754=CARTESIAN_POINT('Ctrl Pts',(2.72996304149713,6.45793530120578,4.14623262832609));
#75755=CARTESIAN_POINT('Ctrl Pts',(2.55693030292749,6.53108143216437,4.15476193609977));
#75756=CARTESIAN_POINT('Ctrl Pts',(2.38093606167818,6.59727771222868,4.16329124387345));
#75757=CARTESIAN_POINT('Ctrl Pts',(2.20255672486121,6.65630306072888,4.17182055164714));
#75758=CARTESIAN_POINT('Ctrl Pts',(2.01500812229077,6.71836250003942,4.18078829299203));
#75759=CARTESIAN_POINT('Ctrl Pts',(1.82482310199486,6.77249424437683,4.18975603433691));
#75760=CARTESIAN_POINT('Ctrl Pts',(1.6326915482164,6.8185001921891,4.1987237756818));
#75761=CARTESIAN_POINT('Ctrl Pts',(1.44995922676027,6.86225549150978,4.20725280780559));
#75762=CARTESIAN_POINT('Ctrl Pts',(1.2654665940685,6.89866095640306,4.21578183992937));
#75763=CARTESIAN_POINT('Ctrl Pts',(1.07981970058149,6.92759813909093,4.22431087205316));
#75764=CARTESIAN_POINT('Ctrl Pts',(0.894170950134817,6.95653561122712,4.23283998948981));
#75765=CARTESIAN_POINT('Ctrl Pts',(0.707368218865288,6.9780046079314,4.24136910692647));
#75766=CARTESIAN_POINT('Ctrl Pts',(0.520025226413481,6.9919382381707,4.24989822436312));
#75767=CARTESIAN_POINT('Ctrl Pts',(0.33264432738187,7.0058746877109,4.25842906756313));
#75768=CARTESIAN_POINT('Ctrl Pts',(0.144723254268758,7.01227270373496,4.26695991076313));
#75769=CARTESIAN_POINT('Ctrl Pts',(-0.0431208157453261,7.01111739723059,
4.27549075396314));
#75770=CARTESIAN_POINT('Ctrl Pts',(-0.0720594031394497,7.01093941483146,
4.27680498523736));
#75771=CARTESIAN_POINT('Ctrl Pts',(-0.100996162252054,7.01058226718464,
4.27811921651158));
#75772=CARTESIAN_POINT('Ctrl Pts',(-0.129928837230052,7.01004600981734,
4.27943344778579));
#75773=CARTESIAN_POINT('Ctrl Pts',(-0.317736381753391,7.00656506035585,
4.28796437514507));
#75774=CARTESIAN_POINT('Ctrl Pts',(-0.505436103814094,6.99553178794519,
4.29649530250434));
#75775=CARTESIAN_POINT('Ctrl Pts',(-0.692411418918306,6.9769759200854,4.30502622986361));
#75776=CARTESIAN_POINT('Ctrl Pts',(-0.87935123699947,6.95842357503326,4.31355553763729));
#75777=CARTESIAN_POINT('Ctrl Pts',(-1.06556661800272,6.93235151479403,4.32208484541098));
#75778=CARTESIAN_POINT('Ctrl Pts',(-1.25044563231558,6.89884137251487,4.33061415318467));
#75779=CARTESIAN_POINT('Ctrl Pts',(-1.44482801649572,6.8636087022486,4.33958189452955));
#75780=CARTESIAN_POINT('Ctrl Pts',(-1.6377326689979,6.82015317632885,4.34854963587444));
#75781=CARTESIAN_POINT('Ctrl Pts',(-1.82845900684053,6.76863089722019,4.35751737721933));
#75782=CARTESIAN_POINT('Ctrl Pts',(-2.00985485667058,6.7196291300295,4.36604640934311));
#75783=CARTESIAN_POINT('Ctrl Pts',(-2.18928010797788,6.66333109644986,4.3745754414669));
#75784=CARTESIAN_POINT('Ctrl Pts',(-2.3661459031183,6.59992273649143,4.38310447359068));
#75785=CARTESIAN_POINT('Ctrl Pts',(-2.54301346738409,6.53651374228183,4.39163359102733));
#75786=CARTESIAN_POINT('Ctrl Pts',(-2.71732123718675,6.4659943859631,4.40016270846398));
#75787=CARTESIAN_POINT('Ctrl Pts',(-2.88849828659866,6.38859955004355,4.40869182590062));
#75788=CARTESIAN_POINT('Ctrl Pts',(-3.05970997160829,6.31118905421859,4.41722266910063));
#75789=CARTESIAN_POINT('Ctrl Pts',(-3.22778939237545,6.22690042720623,4.42575351230064));
#75790=CARTESIAN_POINT('Ctrl Pts',(-3.39218746609123,6.13601587004089,4.43428435550065));
#75791=CARTESIAN_POINT('Ctrl Pts',(-3.4175140469265,6.12201451934559,4.43559858677487));
#75792=CARTESIAN_POINT('Ctrl Pts',(-3.44275330444796,6.10785671364891,4.43691281804908));
#75793=CARTESIAN_POINT('Ctrl Pts',(-3.46790328429765,6.09354358097631,4.4382270493233));
#75794=CARTESIAN_POINT('Ctrl Pts',(-3.63115662896687,6.00063429057287,4.44675797668256));
#75795=CARTESIAN_POINT('Ctrl Pts',(-3.79070204152074,5.90114469265081,4.45528890404183));
#75796=CARTESIAN_POINT('Ctrl Pts',(-3.94601230543783,5.795395883616,4.46381983140109));
#75797=CARTESIAN_POINT('Ctrl Pts',(-4.10129308390098,5.68966715085663,4.47234913917476));
#75798=CARTESIAN_POINT('Ctrl Pts',(-4.25234006527787,5.57768175062914,4.48087844694843));
#75799=CARTESIAN_POINT('Ctrl Pts',(-4.39865495378781,5.45980413201957,4.4894077547221));
#75800=CARTESIAN_POINT('Ctrl Pts',(-4.55249089333668,5.33586722856935,4.498375496067));
#75801=CARTESIAN_POINT('Ctrl Pts',(-4.70109514525235,5.20541660954974,4.50734323741189));
#75802=CARTESIAN_POINT('Ctrl Pts',(-4.84392719318669,5.06892453185156,4.51631097875679));
#75803=CARTESIAN_POINT('Ctrl Pts',(-4.97977178083524,4.93910975792403,4.52484001088056));
#75804=CARTESIAN_POINT('Ctrl Pts',(-5.11039518872745,4.80383073256485,4.53336904300433));
#75805=CARTESIAN_POINT('Ctrl Pts',(-5.23536928461244,4.66353246115396,4.5418980751281));
#75806=CARTESIAN_POINT('Ctrl Pts',(-5.36034463056847,4.52323278638979,4.55042719256472));
#75807=CARTESIAN_POINT('Ctrl Pts',(-5.47967035035606,4.3779139960489,4.55895631000134));
#75808=CARTESIAN_POINT('Ctrl Pts',(-5.59295747354586,4.22805549414947,4.56748542743796));
#75809=CARTESIAN_POINT('Ctrl Pts',(-5.70626751901026,4.07816667020076,4.57601627063799));
#75810=CARTESIAN_POINT('Ctrl Pts',(-5.81353634358416,3.92373654488918,4.58454711383802));
#75811=CARTESIAN_POINT('Ctrl Pts',(-5.91441679640935,3.7652756234904,4.59307795703805));
#75812=CARTESIAN_POINT('Ctrl Pts',(-5.92995807913555,3.74086369916269,4.59439218831231));
#75813=CARTESIAN_POINT('Ctrl Pts',(-5.94534782835778,3.71635616560023,4.59570641958657));
#75814=CARTESIAN_POINT('Ctrl Pts',(-5.96058486758315,3.69175494837331,4.59702065086083));
#75815=CARTESIAN_POINT('Ctrl Pts',(-6.05949047898495,3.53206523470464,4.60555149768623));
#75816=CARTESIAN_POINT('Ctrl Pts',(-6.15199196890276,3.36837123830459,4.61408234451163));
#75817=CARTESIAN_POINT('Ctrl Pts',(-6.23778000506086,3.20120714277645,4.62261319133703));
#75818=CARTESIAN_POINT('Ctrl Pts',(-6.32355367648331,3.03407103795832,4.63114260971897));
#75819=CARTESIAN_POINT('Ctrl Pts',(-6.40261599694051,2.86346626546418,4.6396720281009));
#75820=CARTESIAN_POINT('Ctrl Pts',(-6.4747037524723,2.68995127841028,4.64820144648284));
#75821=CARTESIAN_POINT('Ctrl Pts',(-6.50879210205942,2.60790073468528,4.65223477771133));
#75822=CARTESIAN_POINT('Ctrl Pts',(-6.54132155604487,2.52519977118959,4.65626810893982));
#75823=CARTESIAN_POINT('Ctrl Pts',(-6.57226799596304,2.44190907933527,4.66030144016832));
#75824=CARTESIAN_POINT('Origin',(0.,0.,10.));
#75825=CARTESIAN_POINT('',(-6.57226799589878,2.4419090795082,6.65995074817407));
#75826=CARTESIAN_POINT('',(-6.57226799596303,2.44190907933528,6.1132300454328));
#75827=CARTESIAN_POINT('',(-6.57226799596304,2.44190907933527,10.));
#75828=CARTESIAN_POINT('',(-7.01124999902813,-0.000116739559371617,4.22646564308964));
#75829=CARTESIAN_POINT('Ctrl Pts',(-6.57226799596304,2.44190907933527,6.1132300454328));
#75830=CARTESIAN_POINT('Ctrl Pts',(-6.50682618162574,2.61804223089546,6.10470102768527));
#75831=CARTESIAN_POINT('Ctrl Pts',(-6.43429998856149,2.79154289620592,6.09617200993773));
#75832=CARTESIAN_POINT('Ctrl Pts',(-6.35492875623202,2.96184183671502,6.0876429921902));
#75833=CARTESIAN_POINT('Ctrl Pts',(-6.2719715608649,3.13983482062113,6.07872863656278));
#75834=CARTESIAN_POINT('Ctrl Pts',(-6.18153660119697,3.31432972798643,6.06981428093535));
#75835=CARTESIAN_POINT('Ctrl Pts',(-6.08395206666282,3.48470282994824,6.06089992530793));
#75836=CARTESIAN_POINT('Ctrl Pts',(-5.98636753212867,3.65507593191004,6.05198556968051));
#75837=CARTESIAN_POINT('Ctrl Pts',(-5.88163362047875,3.82132690206206,6.04307121405308));
#75838=CARTESIAN_POINT('Ctrl Pts',(-5.77013196163399,3.98286375712626,6.03415685842566));
#75839=CARTESIAN_POINT('Ctrl Pts',(-5.66342626222106,4.13745251642524,6.02562593106641));
#75840=CARTESIAN_POINT('Ctrl Pts',(-5.55048629613543,4.28777710796666,6.01709500370717));
#75841=CARTESIAN_POINT('Ctrl Pts',(-5.43167763524909,4.43334012108645,6.00856407634793));
#75842=CARTESIAN_POINT('Ctrl Pts',(-5.31289153003419,4.57887549925546,6.00003476857427));
#75843=CARTESIAN_POINT('Ctrl Pts',(-5.18823914698469,4.71965086587602,5.99150546080061));
#75844=CARTESIAN_POINT('Ctrl Pts',(-5.05812674162247,4.85520137874668,5.98297615302695));
#75845=CARTESIAN_POINT('Ctrl Pts',(-4.92132614443279,4.99771961948207,5.97400841168205));
#75846=CARTESIAN_POINT('Ctrl Pts',(-4.77848965503702,5.13446143820321,5.96504067033714));
#75847=CARTESIAN_POINT('Ctrl Pts',(-4.63013458967959,5.26492927245492,5.95607292899224));
#75848=CARTESIAN_POINT('Ctrl Pts',(-4.48903717512546,5.38901451383876,5.94754389686848));
#75849=CARTESIAN_POINT('Ctrl Pts',(-4.3429484747963,5.50742473733119,5.93901486474473));
#75850=CARTESIAN_POINT('Ctrl Pts',(-4.19234891787301,5.61977198054414,5.93048583262097));
#75851=CARTESIAN_POINT('Ctrl Pts',(-4.04174785455652,5.73212034752616,5.92195671518437));
#75852=CARTESIAN_POINT('Ctrl Pts',(-3.88663609185215,5.8384054325547,5.91342759774777));
#75853=CARTESIAN_POINT('Ctrl Pts',(-3.72752493483961,5.93828126840157,5.90489848031117));
#75854=CARTESIAN_POINT('Ctrl Pts',(-3.56838158361615,6.03817731291128,5.89636763711121));
#75855=CARTESIAN_POINT('Ctrl Pts',(-3.40523748165395,6.13166135606096,5.88783679391125));
#75856=CARTESIAN_POINT('Ctrl Pts',(-3.23863129465954,6.21843178781852,5.87930595071128));
#75857=CARTESIAN_POINT('Ctrl Pts',(-3.2129645397654,6.2317993310302,5.8779917194369));
#75858=CARTESIAN_POINT('Ctrl Pts',(-3.18721566557292,6.24500762616669,5.87667748816252));
#75859=CARTESIAN_POINT('Ctrl Pts',(-3.16138669235278,6.25805566801021,5.87536325688813));
#75860=CARTESIAN_POINT('Ctrl Pts',(-2.99372587146071,6.34275301110139,5.86683232952888));
#75861=CARTESIAN_POINT('Ctrl Pts',(-2.82263067900426,6.42072322259215,5.85830140216962));
#75862=CARTESIAN_POINT('Ctrl Pts',(-2.64866010892576,6.49170441331746,5.84977047481036));
#75863=CARTESIAN_POINT('Ctrl Pts',(-2.47472256693643,6.56267212835492,5.8412411670367));
#75864=CARTESIAN_POINT('Ctrl Pts',(-2.29791102008881,6.62665335488609,5.83271185926305));
#75865=CARTESIAN_POINT('Ctrl Pts',(-2.11880460600824,6.68343426720562,5.82418255148939));
#75866=CARTESIAN_POINT('Ctrl Pts',(-1.93049155208761,6.74313389917122,5.81521481014449));
#75867=CARTESIAN_POINT('Ctrl Pts',(-1.739641830731,6.79487335749993,5.80624706879959));
#75868=CARTESIAN_POINT('Ctrl Pts',(-1.54694775921635,6.83846321864463,5.7972793274547));
#75869=CARTESIAN_POINT('Ctrl Pts',(-1.36368043885101,6.87992062822809,5.78875029533093));
#75870=CARTESIAN_POINT('Ctrl Pts',(-1.17874523268746,6.91400667981452,5.78022126320716));
#75871=CARTESIAN_POINT('Ctrl Pts',(-0.992749630653989,6.94061054470977,
5.77169223108339));
#75872=CARTESIAN_POINT('Ctrl Pts',(-0.806752168172955,6.96721467571397,
5.76316311364676));
#75873=CARTESIAN_POINT('Ctrl Pts',(-0.619694592198527,6.98633643033115,
5.75463399621012));
#75874=CARTESIAN_POINT('Ctrl Pts',(-0.432191413893036,6.99791662884441,
5.74610487877349));
#75875=CARTESIAN_POINT('Ctrl Pts',(-0.244650296596127,7.00949917047024,
5.73757403557351));
#75876=CARTESIAN_POINT('Ctrl Pts',(-0.0566637025728533,7.01353709027643,
5.72904319237352));
#75877=CARTESIAN_POINT('Ctrl Pts',(0.131151052699608,7.01002324988126,5.72051234917354));
#75878=CARTESIAN_POINT('Ctrl Pts',(0.160085123971154,7.00948192016367,5.71919811789924));
#75879=CARTESIAN_POINT('Ctrl Pts',(0.189015117454169,7.008761462279,5.71788388662494));
#75880=CARTESIAN_POINT('Ctrl Pts',(0.217938778170615,7.00786196007524,5.71656965535063));
#75881=CARTESIAN_POINT('Ctrl Pts',(0.405687809380714,7.0020231186857,5.70803872799135));
#75882=CARTESIAN_POINT('Ctrl Pts',(0.593234197456993,6.98863390357214,5.69950780063207));
#75883=CARTESIAN_POINT('Ctrl Pts',(0.779961779780187,6.96773178190594,5.69097687327279));
#75884=CARTESIAN_POINT('Ctrl Pts',(0.966653912111869,6.94683362848067,5.68244756549911));
#75885=CARTESIAN_POINT('Ctrl Pts',(1.15252724473683,6.91842544891597,5.67391825772542));
#75886=CARTESIAN_POINT('Ctrl Pts',(1.33697092129266,6.8825965534904,5.66538894995174));
#75887=CARTESIAN_POINT('Ctrl Pts',(1.53089558996927,6.8449259387846,5.65642120860685));
#75888=CARTESIAN_POINT('Ctrl Pts',(1.72323939488692,6.79905167149075,5.64745346726196));
#75889=CARTESIAN_POINT('Ctrl Pts',(1.91330376836143,6.74513863849172,5.63848572591708));
#75890=CARTESIAN_POINT('Ctrl Pts',(2.09407003766044,6.69386307504092,5.62995669379328));
#75891=CARTESIAN_POINT('Ctrl Pts',(2.27277424973527,6.63531656380038,5.62142766166948));
#75892=CARTESIAN_POINT('Ctrl Pts',(2.44882992808045,6.56969242399045,5.61289862954568));
#75893=CARTESIAN_POINT('Ctrl Pts',(2.62488736744776,6.50406762776567,5.60436951210902));
#75894=CARTESIAN_POINT('Ctrl Pts',(2.7982959343672,6.43136517149171,5.59584039467236));
#75895=CARTESIAN_POINT('Ctrl Pts',(2.96848769717246,6.35182708787289,5.58731127723569));
#75896=CARTESIAN_POINT('Ctrl Pts',(3.13871389621424,6.2722729106887,5.57878043403569));
#75897=CARTESIAN_POINT('Ctrl Pts',(3.30572171411774,6.1858804741672,5.57024959083568));
#75898=CARTESIAN_POINT('Ctrl Pts',(3.46896565475864,6.09293885153995,5.56171874763568));
#75899=CARTESIAN_POINT('Ctrl Pts',(3.49411443396873,6.0786205966773,5.56040451636149));
#75900=CARTESIAN_POINT('Ctrl Pts',(3.51917393225434,6.06414699560415,5.55909028508729));
#75901=CARTESIAN_POINT('Ctrl Pts',(3.54414220957539,6.04951920079655,5.5577760538131));
#75902=CARTESIAN_POINT('Ctrl Pts',(3.70621608827091,5.95456737809983,5.54924512645385));
#75903=CARTESIAN_POINT('Ctrl Pts',(3.86449970289803,5.85308232450999,5.5407141990946));
#75904=CARTESIAN_POINT('Ctrl Pts',(4.01846991027773,5.7453917310043,5.53218327173535));
#75905=CARTESIAN_POINT('Ctrl Pts',(4.17241088661168,5.63772158241921,5.52365396396169));
#75906=CARTESIAN_POINT('Ctrl Pts',(4.32203983908092,5.5238484203919,5.51512465618802));
#75907=CARTESIAN_POINT('Ctrl Pts',(4.46686308731619,5.40414292202492,5.50659534841436));
#75908=CARTESIAN_POINT('Ctrl Pts',(4.61913071153202,5.2782841799789,5.49762760706946));
#75909=CARTESIAN_POINT('Ctrl Pts',(4.76608527243226,5.14597792645828,5.48865986572457));
#75910=CARTESIAN_POINT('Ctrl Pts',(4.90719222607484,5.00770316800534,5.47969212437967));
#75911=CARTESIAN_POINT('Ctrl Pts',(5.04139611245137,4.87619292351969,5.4711630922559));
#75912=CARTESIAN_POINT('Ctrl Pts',(5.17031061993882,4.73928441702447,5.46263406013213));
#75913=CARTESIAN_POINT('Ctrl Pts',(5.29351323765484,4.59742799457186,5.45410502800836));
#75914=CARTESIAN_POINT('Ctrl Pts',(5.41671708772249,4.45557015318029,5.44557591057174));
#75915=CARTESIAN_POINT('Ctrl Pts',(5.53420873552052,4.30876453024073,5.43704679313512));
#75916=CARTESIAN_POINT('Ctrl Pts',(5.64560526082019,4.15749537600457,5.4285176756985));
#75917=CARTESIAN_POINT('Ctrl Pts',(5.7570243258543,4.00619561429161,5.41998683249852));
#75918=CARTESIAN_POINT('Ctrl Pts',(5.86234562434225,3.85043076455449,5.41145598929854));
#75919=CARTESIAN_POINT('Ctrl Pts',(5.96122844284613,3.69071565075153,5.40292514609856));
#75920=CARTESIAN_POINT('Ctrl Pts',(5.97646197715504,3.66611051001443,5.40161091482424));
#75921=CARTESIAN_POINT('Ctrl Pts',(5.9915427894084,3.64141167027867,5.40029668354992));
#75922=CARTESIAN_POINT('Ctrl Pts',(6.0064697273841,3.61662107173511,5.3989824522756));
#75923=CARTESIAN_POINT('Ctrl Pts',(6.10336334577159,3.45570054009038,5.39045152491632));
#75924=CARTESIAN_POINT('Ctrl Pts',(6.19380294666506,3.29085637928391,5.38192059755705));
#75925=CARTESIAN_POINT('Ctrl Pts',(6.27748592118411,3.1226266302322,5.37338967019778));
#75926=CARTESIAN_POINT('Ctrl Pts',(6.36115300859805,2.95442881938204,5.36486036242409));
#75927=CARTESIAN_POINT('Ctrl Pts',(6.43806589316049,2.78284697699901,5.35633105465041));
#75928=CARTESIAN_POINT('Ctrl Pts',(6.5079684038665,2.60844279538106,5.34780174687673));
#75929=CARTESIAN_POINT('Ctrl Pts',(6.58146412614586,2.42507368364114,5.33883400553184));
#75930=CARTESIAN_POINT('Ctrl Pts',(6.64720963161899,2.23858476654406,5.32986626418695));
#75931=CARTESIAN_POINT('Ctrl Pts',(6.7049646938521,2.04965241362939,5.32089852284206));
#75932=CARTESIAN_POINT('Ctrl Pts',(6.75989433133306,1.86996278552131,5.31236949071827));
#75933=CARTESIAN_POINT('Ctrl Pts',(6.80759654130547,1.68806339422104,5.30384045859448));
#75934=CARTESIAN_POINT('Ctrl Pts',(6.84791576449454,1.50455184187423,5.29531142647069));
#75935=CARTESIAN_POINT('Ctrl Pts',(6.88823539098236,1.3210384539271,5.28678230903405));
#75936=CARTESIAN_POINT('Ctrl Pts',(6.92117182057933,1.13591317247005,5.27825319159741));
#75937=CARTESIAN_POINT('Ctrl Pts',(6.94662048035468,0.949784430498304,5.26972407416076));
#75938=CARTESIAN_POINT('Ctrl Pts',(6.97207428935737,0.76361802763528,5.26119323096075));
#75939=CARTESIAN_POINT('Ctrl Pts',(6.99003726194707,0.576448062243412,5.25266238776075));
#75940=CARTESIAN_POINT('Ctrl Pts',(7.00045651543156,0.388889621938999,5.24413154456074));
#75941=CARTESIAN_POINT('Ctrl Pts',(7.00206166845832,0.359995037639062,5.24281731328651));
#75942=CARTESIAN_POINT('Ctrl Pts',(7.00348788392251,0.33109124045191,5.24150308201229));
#75943=CARTESIAN_POINT('Ctrl Pts',(7.00473507827124,0.302180485366532,5.24018885073807));
#75944=CARTESIAN_POINT('Ctrl Pts',(7.01283085608495,0.114515227073064,5.23165792337883));
#75945=CARTESIAN_POINT('Ctrl Pts',(7.01338201380923,-0.073507683729425,
5.22312699601959));
#75946=CARTESIAN_POINT('Ctrl Pts',(7.00638023702977,-0.261271002330286,
5.21459606866036));
#75947=CARTESIAN_POINT('Ctrl Pts',(6.99937978952862,-0.448998674306648,
5.2060667608867));
#75948=CARTESIAN_POINT('Ctrl Pts',(6.98482928045914,-0.636466546575077,
5.19753745311305));
#75949=CARTESIAN_POINT('Ctrl Pts',(6.96277248923073,-0.823058822753118,
5.1890081453394));
#75950=CARTESIAN_POINT('Ctrl Pts',(6.93958190871891,-1.01924253591332,5.18004040399449));
#75951=CARTESIAN_POINT('Ctrl Pts',(6.90809305412251,-1.2144579034598,5.17107266264959));
#75952=CARTESIAN_POINT('Ctrl Pts',(6.86841857111615,-1.40799605626111,5.16210492130469));
#75953=CARTESIAN_POINT('Ctrl Pts',(6.83068499617901,-1.59206616476769,5.15357588918093));
#75954=CARTESIAN_POINT('Ctrl Pts',(6.78554761272565,-1.77461891332654,5.14504685705717));
#75955=CARTESIAN_POINT('Ctrl Pts',(6.73315573027801,-1.95505510774619,5.13651782493341));
#75956=CARTESIAN_POINT('Ctrl Pts',(6.68076332377311,-2.13549310700452,5.1279887074968));
#75957=CARTESIAN_POINT('Ctrl Pts',(6.6211163617703,-2.3138142166712,5.11945959006018));
#75958=CARTESIAN_POINT('Ctrl Pts',(6.55441410803044,-2.48943412504762,5.11093047262357));
#75959=CARTESIAN_POINT('Ctrl Pts',(6.48769835789936,-2.6650895679803,5.10239962942359));
#75960=CARTESIAN_POINT('Ctrl Pts',(6.41392457437037,-2.83804243205775,5.09386878622361));
#75961=CARTESIAN_POINT('Ctrl Pts',(6.33334059552266,-3.0077272920936,5.08533794302364));
#75962=CARTESIAN_POINT('Ctrl Pts',(6.32092611517982,-3.03386833637455,5.08402371174928));
#75963=CARTESIAN_POINT('Ctrl Pts',(6.30835009735642,-3.05993186181274,5.08270948047492));
#75964=CARTESIAN_POINT('Ctrl Pts',(6.29561354753464,-3.08591584826908,5.08139524920056));
#75965=CARTESIAN_POINT('Ctrl Pts',(6.21293815891969,-3.25458288982304,5.07286432184127));
#75966=CARTESIAN_POINT('Ctrl Pts',(6.12346653013996,-3.4199544303172,5.06433339448198));
#75967=CARTESIAN_POINT('Ctrl Pts',(6.02748666786519,-3.58148447312109,5.05580246712268));
#75968=CARTESIAN_POINT('Ctrl Pts',(5.93152502724389,-3.742983849654,5.04727315934899));
#75969=CARTESIAN_POINT('Ctrl Pts',(5.82905777520455,-3.90064292077555,5.03874385157529));
#75970=CARTESIAN_POINT('Ctrl Pts',(5.72041797044794,-4.05394188486667,5.03021454380159));
#75971=CARTESIAN_POINT('Ctrl Pts',(5.60619373389035,-4.21512090371347,5.02124680245671));
#75972=CARTESIAN_POINT('Ctrl Pts',(5.48514584979072,-4.37147945782832,5.01227906111183));
#75973=CARTESIAN_POINT('Ctrl Pts',(5.35771237882704,-4.52244896358859,5.00331131976695));
#75974=CARTESIAN_POINT('Ctrl Pts',(5.23651305720318,-4.66603291798977,4.99478228764314));
#75975=CARTESIAN_POINT('Ctrl Pts',(5.10953820610217,-4.80474224204438,4.98625325551933));
#75976=CARTESIAN_POINT('Ctrl Pts',(4.97720561001534,-4.93812220161995,4.97772422339552));
#75977=CARTESIAN_POINT('Ctrl Pts',(4.84487169025308,-5.07150349534734,4.96919510595887));
#75978=CARTESIAN_POINT('Ctrl Pts',(4.70718013637788,-5.19955510299314,4.96066598852221));
#75979=CARTESIAN_POINT('Ctrl Pts',(4.56458547879249,-5.32185925868927,4.95213687108556));
#75980=CARTESIAN_POINT('Ctrl Pts',(4.42196196890907,-5.44418816114669,4.94360602788553));
#75981=CARTESIAN_POINT('Ctrl Pts',(4.27443360685816,-5.56076709028839,4.93507518468549));
#75982=CARTESIAN_POINT('Ctrl Pts',(4.12248854157041,-5.67121810435119,4.92654434148546));
#75983=CARTESIAN_POINT('Ctrl Pts',(4.09908042679551,-5.68823379360236,4.92523011021132));
#75984=CARTESIAN_POINT('Ctrl Pts',(4.07556754898422,-5.70510412730741,4.92391587893717));
#75985=CARTESIAN_POINT('Ctrl Pts',(4.05195175756997,-5.72182781258101,4.92260164766303));
#75986=CARTESIAN_POINT('Ctrl Pts',(3.89865712438774,-5.83038446243039,4.91407072030376));
#75987=CARTESIAN_POINT('Ctrl Pts',(3.7409711977267,-5.93279572789841,4.90553979294449));
#75988=CARTESIAN_POINT('Ctrl Pts',(3.57940810442595,-6.02871994576543,4.89700886558523));
#75989=CARTESIAN_POINT('Ctrl Pts',(3.41787568367046,-6.12462595254317,4.88847955781154));
#75990=CARTESIAN_POINT('Ctrl Pts',(3.25246782836903,-6.214047213169,4.87995025003785));
#75991=CARTESIAN_POINT('Ctrl Pts',(3.08372569427774,-6.29668662114856,4.87142094226416));
#75992=CARTESIAN_POINT('Ctrl Pts',(2.90630967733171,-6.38357395776705,4.86245320091927));
#75993=CARTESIAN_POINT('Ctrl Pts',(2.7252078866279,-6.46296368691272,4.85348545957438));
#75994=CARTESIAN_POINT('Ctrl Pts',(2.54107702163888,-6.534566101326,4.8445177182295));
#75995=CARTESIAN_POINT('Ctrl Pts',(2.36595398875084,-6.60266566722391,4.83598868610571));
#75996=CARTESIAN_POINT('Ctrl Pts',(2.18809147647589,-6.66372151148867,4.82745965398192));
#75997=CARTESIAN_POINT('Ctrl Pts',(2.00807391033646,-6.71753420036892,4.81893062185814));
#75998=CARTESIAN_POINT('Ctrl Pts',(1.8280545435459,-6.77134742751818,4.8104015044215));
#75999=CARTESIAN_POINT('Ctrl Pts',(1.64588037411524,-6.81791726992009,4.80187238698487));
#76000=CARTESIAN_POINT('Ctrl Pts',(1.46215040842561,-6.85709433693608,4.79334326954823));
#76001=CARTESIAN_POINT('Ctrl Pts',(1.27838326720818,-6.89627933095591,4.78481242634824));
#76002=CARTESIAN_POINT('Ctrl Pts',(1.09306000066022,-6.9280684989995,4.77628158314825));
#76003=CARTESIAN_POINT('Ctrl Pts',(0.906790083467169,-6.95236350509851,
4.76775073994825));
#76004=CARTESIAN_POINT('Ctrl Pts',(0.878094004441076,-6.9561063070789,4.76643650867401));
#76005=CARTESIAN_POINT('Ctrl Pts',(0.849375472554175,-6.95967134686522,
4.76512227739976));
#76006=CARTESIAN_POINT('Ctrl Pts',(0.820636730396319,-6.96305837396359,
4.76380804612552));
#76007=CARTESIAN_POINT('Ctrl Pts',(0.634088041024268,-6.9850442167189,4.75527711876636));
#76008=CARTESIAN_POINT('Ctrl Pts',(0.446623371803321,-6.99953271404231,
4.7467461914072));
#76009=CARTESIAN_POINT('Ctrl Pts',(0.258857652594177,-7.00646981569131,
4.73821526404804));
#76010=CARTESIAN_POINT('Ctrl Pts',(0.0711275804650675,-7.0134056003405,
4.72968595627446));
#76011=CARTESIAN_POINT('Ctrl Pts',(-0.116903121735255,-7.01279283896199,
4.72115664850088));
#76012=CARTESIAN_POINT('Ctrl Pts',(-0.304617106574892,-7.00462953916065,
4.7126273407273));
#76013=CARTESIAN_POINT('Ctrl Pts',(-0.50198018779514,-6.99604661976286,
4.70365959938236));
#76014=CARTESIAN_POINT('Ctrl Pts',(-0.698992770735132,-6.97911647346224,
4.69469185803742));
#76015=CARTESIAN_POINT('Ctrl Pts',(-0.894939586002808,-6.95389888479155,
4.68572411669248));
#76016=CARTESIAN_POINT('Ctrl Pts',(-1.08130052324056,-6.92991496112774,
4.67719508456881));
#76017=CARTESIAN_POINT('Ctrl Pts',(-1.26669714843785,-6.8984351143025,4.66866605244514));
#76018=CARTESIAN_POINT('Ctrl Pts',(-1.45052084731942,-6.85956382243009,
4.66013702032147));
#76019=CARTESIAN_POINT('Ctrl Pts',(-1.6343463849235,-6.8206921417421,4.65160790288495));
#76020=CARTESIAN_POINT('Ctrl Pts',(-1.8165986658713,-6.77442893479044,4.64307878544843));
#76021=CARTESIAN_POINT('Ctrl Pts',(-1.99668021412985,-6.72092959976538,
4.63454966801191));
#76022=CARTESIAN_POINT('Ctrl Pts',(-2.17679819970371,-6.66741943979929,
4.62601882481201));
#76023=CARTESIAN_POINT('Ctrl Pts',(-2.35474428206376,-6.60667031551898,
4.61748798161212));
#76024=CARTESIAN_POINT('Ctrl Pts',(-2.52993621871967,-6.53888746590048,
4.60895713841222));
#76025=CARTESIAN_POINT('Ctrl Pts',(-2.55692566358928,-6.5284450818627,4.60764290713748));
#76026=CARTESIAN_POINT('Ctrl Pts',(-2.58384977831466,-6.51783585807876,
4.60632867586275));
#76027=CARTESIAN_POINT('Ctrl Pts',(-2.61070647377527,-6.50706064750344,
4.60501444458801));
#76028=CARTESIAN_POINT('Ctrl Pts',(-2.78503843687542,-6.43711668827108,
4.59648351722844));
#76029=CARTESIAN_POINT('Ctrl Pts',(-2.95658779836757,-6.36015088199461,
4.58795258986888));
#76030=CARTESIAN_POINT('Ctrl Pts',(-3.12478871300473,-6.27640996602184,
4.57942166250931));
#76031=CARTESIAN_POINT('Ctrl Pts',(-3.2929576949143,-6.19268494815441,4.57089235473535));
#76032=CARTESIAN_POINT('Ctrl Pts',(-3.45777922458243,-6.10218752384071,
4.56236304696138));
#76033=CARTESIAN_POINT('Ctrl Pts',(-3.61871023981373,-6.00521130042626,
4.55383373918742));
#76034=CARTESIAN_POINT('Ctrl Pts',(-3.78791362151685,-5.90325019042556,
4.54486599784267));
#76035=CARTESIAN_POINT('Ctrl Pts',(-3.95281566599222,-5.79412685004191,
4.53589825649793));
#76036=CARTESIAN_POINT('Ctrl Pts',(-4.1128168790768,-5.67823598326813,4.52693051515319));
#76037=CARTESIAN_POINT('Ctrl Pts',(-4.26499070232032,-5.56801459221749,
4.51840148302911));
#76038=CARTESIAN_POINT('Ctrl Pts',(-4.41273147077478,-5.45167218924061,
4.50987245090504));
#76039=CARTESIAN_POINT('Ctrl Pts',(-4.55555472963901,-5.32959169803501,
4.50134341878097));
#76040=CARTESIAN_POINT('Ctrl Pts',(-4.69837941711351,-5.20750998570166,
4.49281430134402));
#76041=CARTESIAN_POINT('Ctrl Pts',(-4.83628626606072,-5.07969027186573,
4.48428518390708));
#76042=CARTESIAN_POINT('Ctrl Pts',(-4.96882496410373,-4.94655486562108,
4.47575606647013));
#76043=CARTESIAN_POINT('Ctrl Pts',(-5.10139047974261,-4.8133925210439,4.46722522326986));
#76044=CARTESIAN_POINT('Ctrl Pts',(-5.22858545966915,-4.67491255349351,
4.45869438006958));
#76045=CARTESIAN_POINT('Ctrl Pts',(-5.34999681375759,-4.53157375039661,
4.45016353686931));
#76046=CARTESIAN_POINT('Ctrl Pts',(-5.36870101388029,-4.50949148569738,
4.44884930559637));
#76047=CARTESIAN_POINT('Ctrl Pts',(-5.38726802491544,-4.48729397047657,
4.44753507432342));
#76048=CARTESIAN_POINT('Ctrl Pts',(-5.40569642042982,-4.46498295323199,
4.44622084305048));
#76049=CARTESIAN_POINT('Ctrl Pts',(-5.52531867163167,-4.32015785940772,
4.43768991569185));
#76050=CARTESIAN_POINT('Ctrl Pts',(-5.63913799204207,-4.17049797480983,
4.42915898833322));
#76051=CARTESIAN_POINT('Ctrl Pts',(-5.7467755444098,-4.01649068275696,4.42062806097458));
#76052=CARTESIAN_POINT('Ctrl Pts',(-5.85439266192656,-3.86251262879054,
4.41209875320155));
#76053=CARTESIAN_POINT('Ctrl Pts',(-5.95583017811012,-3.70418906531192,
4.40356944542851));
#76054=CARTESIAN_POINT('Ctrl Pts',(-6.05075168607111,-3.54203763334153,
4.39504013765547));
#76055=CARTESIAN_POINT('Ctrl Pts',(-6.1505524617193,-3.37155110156666,4.38607239631026));
#76056=CARTESIAN_POINT('Ctrl Pts',(-6.24314950152146,-3.19683311190102,
4.37710465496506));
#76057=CARTESIAN_POINT('Ctrl Pts',(-6.32820521176558,-3.01851707967388,
4.36813691361985));
#76058=CARTESIAN_POINT('Ctrl Pts',(-6.40909992728024,-2.84892441320487,
4.3596078814967));
#76059=CARTESIAN_POINT('Ctrl Pts',(-6.48317339141903,-2.67607762759124,
4.35107884937354));
#76060=CARTESIAN_POINT('Ctrl Pts',(-6.55018339351676,-2.50054475540777,
4.34254981725039));
#76061=CARTESIAN_POINT('Ctrl Pts',(-6.61719406589158,-2.32501012743174,
4.33402069981438));
#76062=CARTESIAN_POINT('Ctrl Pts',(-6.67714102886938,-2.14678964641539,
4.32549158237837));
#76063=CARTESIAN_POINT('Ctrl Pts',(-6.72983089625954,-1.96646959555711,
4.31696246494236));
#76064=CARTESIAN_POINT('Ctrl Pts',(-6.78253142480478,-1.78611305912537,
4.30843162174297));
#76065=CARTESIAN_POINT('Ctrl Pts',(-6.82797183996164,-1.60365639853373,
4.29990077854357));
#76066=CARTESIAN_POINT('Ctrl Pts',(-6.86600889366736,-1.41970012135687,
4.29136993534418));
#76067=CARTESIAN_POINT('Ctrl Pts',(-6.87186874649775,-1.39136047339615,
4.29005570406711));
#76068=CARTESIAN_POINT('Ctrl Pts',(-6.87755299079739,-1.36298525616782,
4.28874147279004));
#76069=CARTESIAN_POINT('Ctrl Pts',(-6.88306121050991,-1.33457668752077,
4.28742724151297));
#76070=CARTESIAN_POINT('Ctrl Pts',(-6.91978280158916,-1.14518557833293,
4.2786656695244));
#76071=CARTESIAN_POINT('Ctrl Pts',(-6.94868659776524,-0.954261181418948,
4.26990409753583));
#76072=CARTESIAN_POINT('Ctrl Pts',(-6.96967016874586,-0.762446261315601,
4.26114252554726));
#76073=CARTESIAN_POINT('Ctrl Pts',(-6.99064763812959,-0.570687117100848,
4.25238350124613));
#76074=CARTESIAN_POINT('Ctrl Pts',(-7.00370945223445,-0.37803823423764,
4.24362447694499));
#76075=CARTESIAN_POINT('Ctrl Pts',(-7.00880493496689,-0.185148443374064,
4.23486545264386));
#76076=CARTESIAN_POINT('Ctrl Pts',(-7.0104337725736,-0.123488702421782,
4.23206551612579));
#76077=CARTESIAN_POINT('Ctrl Pts',(-7.01124897190917,-0.0618043785464321,
4.22926557960772));
#76078=CARTESIAN_POINT('Ctrl Pts',(-7.01124999902813,-0.000116739559371617,
4.22646564308964));
#76079=CARTESIAN_POINT('Ctrl Pts',(-7.01077745316898,-0.000116731691330088,
4.22646564308964));
#76080=CARTESIAN_POINT('Ctrl Pts',(-7.01035168527277,0.718306532755159,
4.19385497538491));
#76081=CARTESIAN_POINT('Ctrl Pts',(-6.88322317671624,1.55002980981697,4.15610807856266));
#76082=CARTESIAN_POINT('Ctrl Pts',(-6.6121722290669,2.33607121355468,4.11836118174041));
#76083=CARTESIAN_POINT('Ctrl Pts',(-6.57269630323124,2.4420685397187,4.11322495262288));
#76084=CARTESIAN_POINT('',(-7.01124999890438,0.000123949001866673,4.77353435691037));
#76085=CARTESIAN_POINT('Ctrl Pts',(-6.57226799596304,2.44190907933527,4.66030144016832));
#76086=CARTESIAN_POINT('Ctrl Pts',(-6.63771043057231,2.26577425834615,4.66883072547144));
#76087=CARTESIAN_POINT('Ctrl Pts',(-6.69607048136911,2.08700116691844,4.67736001077457));
#76088=CARTESIAN_POINT('Ctrl Pts',(-6.74715618316126,1.90617680253662,4.68588929607769));
#76089=CARTESIAN_POINT('Ctrl Pts',(-6.79824010009948,1.7253587558732,4.69441828338103));
#76090=CARTESIAN_POINT('Ctrl Pts',(-6.84205009466234,1.54248987476095,4.70294727068437));
#76091=CARTESIAN_POINT('Ctrl Pts',(-6.87844442865365,1.35817112486742,4.7114762579877));
#76092=CARTESIAN_POINT('Ctrl Pts',(-6.91484744362043,1.17380841025816,4.72000727967171));
#76093=CARTESIAN_POINT('Ctrl Pts',(-6.94383120347836,0.987995436261786,
4.72853830135572));
#76094=CARTESIAN_POINT('Ctrl Pts',(-6.96530514058173,0.801343160628309,
4.73706932303973));
#76095=CARTESIAN_POINT('Ctrl Pts',(-6.98103312913002,0.664634887732377,
4.74331763282593));
#76096=CARTESIAN_POINT('Ctrl Pts',(-6.99273359566149,0.52747659570593,4.74956594261214));
#76097=CARTESIAN_POINT('Ctrl Pts',(-7.00038860523991,0.390110161527862,
4.75581425239835));
#76098=CARTESIAN_POINT('Ctrl Pts',(-7.00762509928983,0.260253840199072,
4.76172095390235));
#76099=CARTESIAN_POINT('Ctrl Pts',(-7.01124769942693,0.130195277014969,
4.76762765540636));
#76100=CARTESIAN_POINT('Ctrl Pts',(-7.01124999890438,0.000123949001866673,
4.77353435691037));
#76101=CARTESIAN_POINT('Ctrl Pts',(-7.01124999909022,0.000112948703611393,
4.77329468133506));
#76102=CARTESIAN_POINT('Ctrl Pts',(-7.01125679909962,-0.421995179608593,
4.79266801673904));
#76103=CARTESIAN_POINT('Ctrl Pts',(-6.97314410821326,-0.8432534060986,4.81213169562656));
#76104=CARTESIAN_POINT('Ctrl Pts',(-6.88164419495031,-1.34472218830463,
4.83531049418384));
#76105=CARTESIAN_POINT('Ctrl Pts',(-6.86430093479642,-1.43062134470753,
4.83928390680739));
#76106=CARTESIAN_POINT('Ctrl Pts',(-6.75240376876267,-1.93582448205209,
4.86268916910286));
#76107=CARTESIAN_POINT('Ctrl Pts',(-6.62106364394987,-2.34603645146997,
4.88177993626495));
#76108=CARTESIAN_POINT('Ctrl Pts',(-6.41003474131369,-2.84273608613219,
4.9060725872766));
#76109=CARTESIAN_POINT('Ctrl Pts',(-6.3647098019935,-2.94281543766909,4.91103505537233));
#76110=CARTESIAN_POINT('Ctrl Pts',(-6.20739139014251,-3.26952732963385,
4.92752792430019));
#76111=CARTESIAN_POINT('Ctrl Pts',(-6.08549654383899,-3.49116688776528,
4.9391679889615));
#76112=CARTESIAN_POINT('Ctrl Pts',(-5.78797482262491,-3.96902597464448,
4.96506755660791));
#76113=CARTESIAN_POINT('Ctrl Pts',(-5.6067552475093,-4.22115166241315,4.97928627065715));
#76114=CARTESIAN_POINT('Ctrl Pts',(-5.15084960484008,-4.7740536520115,5.01182502581467));
#76115=CARTESIAN_POINT('Ctrl Pts',(-4.86548153778363,-5.06457642353853,
5.02996494644311));
#76116=CARTESIAN_POINT('Ctrl Pts',(-4.41388272609466,-5.45073422911981,
5.05660352002761));
#76117=CARTESIAN_POINT('Ctrl Pts',(-4.26637231559178,-5.56694978148892,
5.06503526396739));
#76118=CARTESIAN_POINT('Ctrl Pts',(-3.90823318420276,-5.82650464906067,
5.08513167971144));
#76119=CARTESIAN_POINT('Ctrl Pts',(-3.69410520199835,-5.96456428372902,
5.09685270424898));
#76120=CARTESIAN_POINT('Ctrl Pts',(-3.21358206001639,-6.23856225368875,
5.12230448629601));
#76121=CARTESIAN_POINT('Ctrl Pts',(-2.94503149337547,-6.36973808840384,
5.13600165082681));
#76122=CARTESIAN_POINT('Ctrl Pts',(-2.44196155883025,-6.57683034191199,
5.16073197124822));
#76123=CARTESIAN_POINT('Ctrl Pts',(-2.2102359956425,-6.65828306934746,5.17179214836363));
#76124=CARTESIAN_POINT('Ctrl Pts',(-1.75342406793481,-6.79237212488537,
5.19315794123468));
#76125=CARTESIAN_POINT('Ctrl Pts',(-1.5290646716379,-6.84636953226539,5.20345684828559));
#76126=CARTESIAN_POINT('Ctrl Pts',(-1.15368175683848,-6.91733830065786,
5.22061732016552));
#76127=CARTESIAN_POINT('Ctrl Pts',(-1.00404072754944,-6.94063774890685,
5.22744235307077));
#76128=CARTESIAN_POINT('Ctrl Pts',(-0.608744709303136,-6.9891339614576,
5.24556671140942));
#76129=CARTESIAN_POINT('Ctrl Pts',(-0.36231299776361,-7.0062322788189,5.25693394089039));
#76130=CARTESIAN_POINT('Ctrl Pts',(0.191738457234614,-7.01536042568755,
5.28242948160838));
#76131=CARTESIAN_POINT('Ctrl Pts',(0.498978774929529,-7.00021939269596,
5.29651798161029));
#76132=CARTESIAN_POINT('Ctrl Pts',(1.22071726182776,-6.91688113884293,5.32951377679443));
#76133=CARTESIAN_POINT('Ctrl Pts',(1.6320460236115,-6.83153174664252,5.34821330112677));
#76134=CARTESIAN_POINT('Ctrl Pts',(2.1580545733809,-6.67213793202217,5.37286078239703));
#76135=CARTESIAN_POINT('Ctrl Pts',(2.28174665464909,-6.63085633682415,5.37871746682301));
#76136=CARTESIAN_POINT('Ctrl Pts',(2.52624737793925,-6.54160356431424,5.39048317998939));
#76137=CARTESIAN_POINT('Ctrl Pts',(2.64701557281996,-6.493674639887,5.39639814990493));
#76138=CARTESIAN_POINT('Ctrl Pts',(3.02401957130557,-6.33178876439205,5.4151804945424));
#76139=CARTESIAN_POINT('Ctrl Pts',(3.27478963052073,-6.20580343161588,5.42811728053557));
#76140=CARTESIAN_POINT('Ctrl Pts',(3.68829303968288,-5.96600154655731,5.45006060240372));
#76141=CARTESIAN_POINT('Ctrl Pts',(3.85497915505517,-5.85967724610324,5.4590932145682));
#76142=CARTESIAN_POINT('Ctrl Pts',(4.3829150375993,-5.49063334076114,5.48836234204885));
#76143=CARTESIAN_POINT('Ctrl Pts',(4.72360355932173,-5.20043964978641,5.5082534046618));
#76144=CARTESIAN_POINT('Ctrl Pts',(5.15033679390985,-4.76019070077597,5.53576602263396));
#76145=CARTESIAN_POINT('Ctrl Pts',(5.26199334869462,-4.63646520330071,5.54326332769117));
#76146=CARTESIAN_POINT('Ctrl Pts',(5.5174107115067,-4.33231651263527,5.56132251036776));
#76147=CARTESIAN_POINT('Ctrl Pts',(5.65688475498112,-4.14854673141831,5.57192926731237));
#76148=CARTESIAN_POINT('Ctrl Pts',(5.9171127704807,-3.76808686898075,5.59313905822258));
#76149=CARTESIAN_POINT('Ctrl Pts',(6.03772568284979,-3.57163444464497,5.60372898481114));
#76150=CARTESIAN_POINT('Ctrl Pts',(6.19654863945421,-3.28183305172802,5.61882606002129));
#76151=CARTESIAN_POINT('Ctrl Pts',(6.24276404825244,-3.19304564660264,5.62338513109736));
#76152=CARTESIAN_POINT('Ctrl Pts',(6.47405621673876,-2.72446413139617,5.64711856109728));
#76153=CARTESIAN_POINT('Ctrl Pts',(6.62642664102905,-2.32950285230411,5.6659591119782));
#76154=CARTESIAN_POINT('Ctrl Pts',(6.79130883108704,-1.75147155130558,5.69291614749831));
#76155=CARTESIAN_POINT('Ctrl Pts',(6.8337210897994,-1.57790458700881,5.70094476091029));
#76156=CARTESIAN_POINT('Ctrl Pts',(6.91857734053677,-1.16239933069317,5.72021849451929));
#76157=CARTESIAN_POINT('Ctrl Pts',(6.95503008523638,-0.919477357552379,
5.73151644756159));
#76158=CARTESIAN_POINT('Ctrl Pts',(7.00029356200322,-0.451611455313158,
5.75314509896803));
#76159=CARTESIAN_POINT('Ctrl Pts',(7.01116692644202,-0.227162863482876,
5.76346453614652));
#76160=CARTESIAN_POINT('Ctrl Pts',(7.01128632737948,0.0974833021738531,
5.77829163797521));
#76161=CARTESIAN_POINT('Ctrl Pts',(7.00918105544768,0.197535147302001,5.78284839017917));
#76162=CARTESIAN_POINT('Ctrl Pts',(6.98775276409793,0.702071791296174,5.80577727127322));
#76163=CARTESIAN_POINT('Ctrl Pts',(6.93555523761715,1.10438764393122,5.82384990722907));
#76164=CARTESIAN_POINT('Ctrl Pts',(6.80856887317956,1.68422154293215,5.85046025067915));
#76165=CARTESIAN_POINT('Ctrl Pts',(6.76079180215199,1.86678995278535,5.8589329155193));
#76166=CARTESIAN_POINT('Ctrl Pts',(6.63113405065837,2.29148941048707,5.87910821630758));
#76167=CARTESIAN_POINT('Ctrl Pts',(6.54326422017995,2.53151202546576,5.89086742973181));
#76168=CARTESIAN_POINT('Ctrl Pts',(6.32486766552816,3.04015866555996,5.91633746879359));
#76169=CARTESIAN_POINT('Ctrl Pts',(6.1898827228241,3.30633826493007,5.93001483632165));
#76170=CARTESIAN_POINT('Ctrl Pts',(5.91352839167062,3.77467177635828,5.95473407009145));
#76171=CARTESIAN_POINT('Ctrl Pts',(5.77766201619294,3.97952128726904,5.96580241558632));
#76172=CARTESIAN_POINT('Ctrl Pts',(5.43098270746449,4.44692559060206,5.99191841812494));
#76173=CARTESIAN_POINT('Ctrl Pts',(5.21147100502431,4.70226371963072,6.0068840772248));
#76174=CARTESIAN_POINT('Ctrl Pts',(4.8754280415691,5.0405940508303,6.02847610270383));
#76175=CARTESIAN_POINT('Ctrl Pts',(4.77339167016613,5.13732589108303,6.03489417321059));
#76176=CARTESIAN_POINT('Ctrl Pts',(4.47046904835554,5.40767968635405,6.05351321583316));
#76177=CARTESIAN_POINT('Ctrl Pts',(4.26254070274911,5.57304587974599,6.06575605996636));
#76178=CARTESIAN_POINT('Ctrl Pts',(3.88452279988924,5.84012612300974,6.08699336517462));
#76179=CARTESIAN_POINT('Ctrl Pts',(3.71856830581541,5.9471709255966,6.09600876968458));
#76180=CARTESIAN_POINT('Ctrl Pts',(3.19889281292691,6.25210750204974,6.1233666735894));
#76181=CARTESIAN_POINT('Ctrl Pts',(2.83235371138637,6.42647188805495,6.14144849944093));
#76182=CARTESIAN_POINT('Ctrl Pts',(2.27620785654595,6.63415723920077,6.16806267351317));
#76183=CARTESIAN_POINT('Ctrl Pts',(2.09701923295155,6.69295697248118,6.1765297257224));
#76184=CARTESIAN_POINT('Ctrl Pts',(1.67009496807675,6.81421956123695,6.19669425328008));
#76185=CARTESIAN_POINT('Ctrl Pts',(1.42088376594601,6.87050886259863,6.20844827668929));
#76186=CARTESIAN_POINT('Ctrl Pts',(0.875137031947884,6.96280728062533,6.23391583473576));
#76187=CARTESIAN_POINT('Ctrl Pts',(0.578234595829499,6.99372575616231,6.24759589254961));
#76188=CARTESIAN_POINT('Ctrl Pts',(0.0348466737759841,7.01546422384793,
6.27231662754573));
#76189=CARTESIAN_POINT('Ctrl Pts',(-0.210919380432283,7.01237966542289,
6.28338385771086));
#76190=CARTESIAN_POINT('Ctrl Pts',(-0.68490445812741,6.98148577307377,6.30470031306995));
#76191=CARTESIAN_POINT('Ctrl Pts',(-0.912919308510342,6.95534438888378,
6.31494352266387));
#76192=CARTESIAN_POINT('Ctrl Pts',(-1.28919125067015,6.89338140761715,6.33207208481146));
#76193=CARTESIAN_POINT('Ctrl Pts',(-1.43829576788489,6.8638200709508,6.33892195019952));
#76194=CARTESIAN_POINT('Ctrl Pts',(-1.82833172178249,6.77322360981884,6.35714387876324));
#76195=CARTESIAN_POINT('Ctrl Pts',(-2.06717972324997,6.70418680535927,6.36858525574703));
#76196=CARTESIAN_POINT('Ctrl Pts',(-2.59423413122072,6.52099594917694,6.39425799756116));
#76197=CARTESIAN_POINT('Ctrl Pts',(-2.87956637883259,6.40012049589865,6.40844827520084));
#76198=CARTESIAN_POINT('Ctrl Pts',(-3.51914294893291,6.07771839486986,6.44096974458012));
#76199=CARTESIAN_POINT('Ctrl Pts',(-3.86569120837204,5.86340041979019,6.4591197941867));
#76200=CARTESIAN_POINT('Ctrl Pts',(-4.34206960367874,5.50810711352361,6.48576265428615));
#76201=CARTESIAN_POINT('Ctrl Pts',(-4.48787096327097,5.38997447936336,6.4941882725242));
#76202=CARTESIAN_POINT('Ctrl Pts',(-4.8198869149895,5.09814375303654,6.51427281140552));
#76203=CARTESIAN_POINT('Ctrl Pts',(-5.0017265330871,4.919868756499,6.52598804908439));
#76204=CARTESIAN_POINT('Ctrl Pts',(-5.37502510657105,4.5117526659675,6.55143706435205));
#76205=CARTESIAN_POINT('Ctrl Pts',(-5.5622990345381,4.27874299650751,6.56513722909619));
#76206=CARTESIAN_POINT('Ctrl Pts',(-5.87537128270766,3.8337803959583,6.58986923763532));
#76207=CARTESIAN_POINT('Ctrl Pts',(-6.0059615065987,3.62578118502098,6.60092818467359));
#76208=CARTESIAN_POINT('Ctrl Pts',(-6.23777964980658,3.20953274361292,6.62231029130177));
#76209=CARTESIAN_POINT('Ctrl Pts',(-6.34013794114365,3.00227343359751,6.63262653190011));
#76210=CARTESIAN_POINT('Ctrl Pts',(-6.48191316875309,2.67546416034317,6.64862854258803));
#76211=CARTESIAN_POINT('Ctrl Pts',(-6.52865946284866,2.55927911941613,6.65426924392862));
#76212=CARTESIAN_POINT('Ctrl Pts',(-6.57226799589878,2.4419090795082,6.65995074817407));
#76213=CARTESIAN_POINT('Origin',(0.,0.,10.));
#76214=CARTESIAN_POINT('',(-6.57226798695174,2.4419091035887,8.66059774113391));
#76215=CARTESIAN_POINT('',(-6.57226800401825,2.44190905765509,8.11350492783088));
#76216=CARTESIAN_POINT('',(-6.57226799596304,2.44190907933527,10.));
#76217=CARTESIAN_POINT('',(-7.01124999771048,0.000179177963096134,6.22646564308964));
#76218=CARTESIAN_POINT('Ctrl Pts',(-6.57226800401825,2.44190905765509,8.11350492783088));
#76219=CARTESIAN_POINT('Ctrl Pts',(-6.55743799171866,2.48182324488917,8.11158964032659));
#76220=CARTESIAN_POINT('Ctrl Pts',(-6.5422430036516,2.52160602315529,8.10967167924349));
#76221=CARTESIAN_POINT('Ctrl Pts',(-6.4803660331804,2.67928337028087,8.10202931630123));
#76222=CARTESIAN_POINT('Ctrl Pts',(-6.43085534038898,2.79603327768028,8.0962737171796));
#76223=CARTESIAN_POINT('Ctrl Pts',(-6.2501010499617,3.1920274850446,8.07638364749166));
#76224=CARTESIAN_POINT('Ctrl Pts',(-6.10361224707174,3.46391684443965,8.06214069269033));
#76225=CARTESIAN_POINT('Ctrl Pts',(-5.81073924316456,3.93088299834635,8.03684019739495));
#76226=CARTESIAN_POINT('Ctrl Pts',(-5.67119309610008,4.12966147061864,8.02576427414835));
#76227=CARTESIAN_POINT('Ctrl Pts',(-5.45957965384424,4.40008531075991,8.01020713756199));
#76228=CARTESIAN_POINT('Ctrl Pts',(-5.39584023614814,4.47802066956506,8.00566073656017));
#76229=CARTESIAN_POINT('Ctrl Pts',(-5.17382484179504,4.73785729996587,7.9902641067623));
#76230=CARTESIAN_POINT('Ctrl Pts',(-5.00785430304868,4.91295751313342,7.97948278038044));
#76231=CARTESIAN_POINT('Ctrl Pts',(-4.68900500442983,5.21636601734565,7.95976237792332));
#76232=CARTESIAN_POINT('Ctrl Pts',(-4.53904117168727,5.34736809059905,7.95083737907751));
#76233=CARTESIAN_POINT('Ctrl Pts',(-4.25854004546789,5.57208997865151,7.93453846180782));
#76234=CARTESIAN_POINT('Ctrl Pts',(-4.12996819005442,5.66804295151848,7.92719677564156));
#76235=CARTESIAN_POINT('Ctrl Pts',(-3.6324499729222,6.01341807435682,7.8993789797547));
#76236=CARTESIAN_POINT('Ctrl Pts',(-3.24331000222098,6.2319215416855,7.87887419765568));
#76237=CARTESIAN_POINT('Ctrl Pts',(-2.55366060353697,6.53695715410225,7.84466811319653));
#76238=CARTESIAN_POINT('Ctrl Pts',(-2.26329460062408,6.64307857538963,7.83082448585817));
#76239=CARTESIAN_POINT('Ctrl Pts',(-1.72998530629469,6.79894760719639,7.8059372115454));
#76240=CARTESIAN_POINT('Ctrl Pts',(-1.48960655813323,6.8556259112,7.79490207189863));
#76241=CARTESIAN_POINT('Ctrl Pts',(-1.09776743482913,6.92643141625173,7.77685522302357));
#76242=CARTESIAN_POINT('Ctrl Pts',(-0.947960251614167,6.94851891099159,
7.76993219269087));
#76243=CARTESIAN_POINT('Ctrl Pts',(-0.568394476943045,6.99197819336942,
7.75239508717265));
#76244=CARTESIAN_POINT('Ctrl Pts',(-0.338074809094541,7.00689211214926,
7.74176312764431));
#76245=CARTESIAN_POINT('Ctrl Pts',(0.137981144539973,7.01418799745145,7.71990514651528));
#76246=CARTESIAN_POINT('Ctrl Pts',(0.383433248609888,7.00505919989913,7.70870081730449));
#76247=CARTESIAN_POINT('Ctrl Pts',(0.925277745823956,6.9563376951143,7.68404864538288));
#76248=CARTESIAN_POINT('Ctrl Pts',(1.22064235856468,6.91063012757235,7.67066995300729));
#76249=CARTESIAN_POINT('Ctrl Pts',(1.76078477099419,6.79132354169578,7.64589328183402));
#76250=CARTESIAN_POINT('Ctrl Pts',(2.00619572181711,6.72291700716577,7.6345083647682));
#76251=CARTESIAN_POINT('Ctrl Pts',(2.425141450439,6.58115109824151,7.61443049309929));
#76252=CARTESIAN_POINT('Ctrl Pts',(2.60045505571314,6.51386922787786,7.60581926436072));
#76253=CARTESIAN_POINT('Ctrl Pts',(3.1461899633329,6.27888022055778,7.57849719911343));
#76254=CARTESIAN_POINT('Ctrl Pts',(3.50484782594696,6.08595945740171,7.55980860075223));
#76255=CARTESIAN_POINT('Ctrl Pts',(4.10429799392953,5.6928625669429,7.52728829737601));
#76256=CARTESIAN_POINT('Ctrl Pts',(4.35224237910438,5.50562772812465,7.51337495393488));
#76257=CARTESIAN_POINT('Ctrl Pts',(4.77412475970954,5.1406807790236,7.48838878419116));
#76258=CARTESIAN_POINT('Ctrl Pts',(4.95257714444692,4.96898805618932,7.47732426678287));
#76259=CARTESIAN_POINT('Ctrl Pts',(5.22512418692035,4.67746654960826,7.45923645188895));
#76260=CARTESIAN_POINT('Ctrl Pts',(5.32505063162602,4.5633814271053,7.45230257026397));
#76261=CARTESIAN_POINT('Ctrl Pts',(5.56718418754557,4.26814753012032,7.43477520138407));
#76262=CARTESIAN_POINT('Ctrl Pts',(5.70431522031333,4.08306395911104,7.42416415263037));
#76263=CARTESIAN_POINT('Ctrl Pts',(5.9683466003706,3.68737396183035,7.40232538388935));
#76264=CARTESIAN_POINT('Ctrl Pts',(6.09378402112142,3.47615988872294,7.39111954873523));
#76265=CARTESIAN_POINT('Ctrl Pts',(6.34662788481562,2.9945022179251,7.36646920714207));
#76266=CARTESIAN_POINT('Ctrl Pts',(6.4683505287011,2.72161238445936,7.35309374409657));
#76267=CARTESIAN_POINT('Ctrl Pts',(6.66102318643904,2.20301642554055,7.32831396595407));
#76268=CARTESIAN_POINT('Ctrl Pts',(6.73665588446388,1.95958532626026,7.31692273169131));
#76269=CARTESIAN_POINT('Ctrl Pts',(6.84476244024639,1.53040771121768,7.29683105917654));
#76270=CARTESIAN_POINT('Ctrl Pts',(6.88330997576356,1.34646291639651,7.28821243578745));
#76271=CARTESIAN_POINT('Ctrl Pts',(6.98169930849974,0.760596471026311,7.26089514120011));
#76272=CARTESIAN_POINT('Ctrl Pts',(7.01403534692144,0.354898640283086,7.24221888701904));
#76273=CARTESIAN_POINT('Ctrl Pts',(7.0103298676516,-0.151373695439597,7.21925066148355));
#76274=CARTESIAN_POINT('Ctrl Pts',(7.00745561476455,-0.251405832416107,
7.21472571493635));
#76275=CARTESIAN_POINT('Ctrl Pts',(6.99672086768851,-0.465354874216318,
7.20506380305275));
#76276=CARTESIAN_POINT('Ctrl Pts',(6.98821673433173,-0.579210838011116,
7.1999319245512));
#76277=CARTESIAN_POINT('Ctrl Pts',(6.95009629580528,-0.963102972505531,
7.18262007458876));
#76278=CARTESIAN_POINT('Ctrl Pts',(6.90757179907468,-1.23160704678244,7.17050530862667));
#76279=CARTESIAN_POINT('Ctrl Pts',(6.82156504401769,-1.62514358855543,7.15236410297419));
#76280=CARTESIAN_POINT('Ctrl Pts',(6.78995984234394,-1.752508536021,7.1464257570538));
#76281=CARTESIAN_POINT('Ctrl Pts',(6.72057170037631,-2.00196290508527,7.13461531624808));
#76282=CARTESIAN_POINT('Ctrl Pts',(6.68298837135976,-2.12405399667506,7.12875634265293));
#76283=CARTESIAN_POINT('Ctrl Pts',(6.50651377443913,-2.64616301204923,7.10342390529694));
#76284=CARTESIAN_POINT('Ctrl Pts',(6.33487610871482,-3.03418177473879,7.08394471886494));
#76285=CARTESIAN_POINT('Ctrl Pts',(5.98020890095359,-3.67273545297891,7.05081139597953));
#76286=CARTESIAN_POINT('Ctrl Pts',(5.81366792564436,-3.93104992642798,7.0370469422111));
#76287=CARTESIAN_POINT('Ctrl Pts',(5.48211435815663,-4.37792873893386,7.01212261396588));
#76288=CARTESIAN_POINT('Ctrl Pts',(5.32291652827791,-4.57016345622703,7.00097162699666));
#76289=CARTESIAN_POINT('Ctrl Pts',(5.05055109649184,-4.86546605050667,6.98276295231262));
#76290=CARTESIAN_POINT('Ctrl Pts',(4.94366555649898,-4.97403209793866,6.97579686226693));
#76291=CARTESIAN_POINT('Ctrl Pts',(4.48971091255839,-5.40602676156326,6.9470295041862));
#76292=CARTESIAN_POINT('Ctrl Pts',(4.11378047428365,-5.69732039118457,6.92517891382745));
#76293=CARTESIAN_POINT('Ctrl Pts',(3.45902305259344,-6.10583499038029,6.89020694535978));
#76294=CARTESIAN_POINT('Ctrl Pts',(3.19696155546038,-6.24703943541135,6.87688058968884));
#76295=CARTESIAN_POINT('Ctrl Pts',(2.69327891564335,-6.47841586711455,6.85205354450293));
#76296=CARTESIAN_POINT('Ctrl Pts',(2.45411924910366,-6.57274052199594,6.84056625555677));
#76297=CARTESIAN_POINT('Ctrl Pts',(2.02967220752053,-6.71373930813828,6.82026128866536));
#76298=CARTESIAN_POINT('Ctrl Pts',(1.84664925498781,-6.76636898724402,6.81152672305988));
#76299=CARTESIAN_POINT('Ctrl Pts',(1.27106942842937,-6.90678617362863,6.78428161912001));
#76300=CARTESIAN_POINT('Ctrl Pts',(0.87294010245506,-6.96830686883063,6.76579619228501));
#76301=CARTESIAN_POINT('Ctrl Pts',(0.161859247530876,-7.01625876510001,
6.73346188776163));
#76302=CARTESIAN_POINT('Ctrl Pts',(-0.149063728130618,-7.01654257392534,
6.7195377353665));
#76303=CARTESIAN_POINT('Ctrl Pts',(-0.707083092720185,-6.97993401271807,
6.6944891229262));
#76304=CARTESIAN_POINT('Ctrl Pts',(-0.954138696093317,-6.9504720131852,
6.68337298133156));
#76305=CARTESIAN_POINT('Ctrl Pts',(-1.34889721563537,-6.88194866636739,
6.66521305977248));
#76306=CARTESIAN_POINT('Ctrl Pts',(-1.49780368827869,-6.8510819173672,6.65825999598243));
#76307=CARTESIAN_POINT('Ctrl Pts',(-1.86832894631033,-6.76161818534322,
6.6407621070194));
#76308=CARTESIAN_POINT('Ctrl Pts',(-2.08830171764772,-6.69694928891135,
6.63020036457347));
#76309=CARTESIAN_POINT('Ctrl Pts',(-2.53673320352266,-6.54086893825623,
6.60840144941294));
#76310=CARTESIAN_POINT('Ctrl Pts',(-2.76435195785374,-6.4479720427829,6.59718667471982));
#76311=CARTESIAN_POINT('Ctrl Pts',(-3.25629743072108,-6.2163491577006,6.57254707004008));
#76312=CARTESIAN_POINT('Ctrl Pts',(-3.51759857248614,-6.07231204571228,
6.55919065236748));
#76313=CARTESIAN_POINT('Ctrl Pts',(-3.98444287679584,-5.77469968391117,
6.53439254664884));
#76314=CARTESIAN_POINT('Ctrl Pts',(-4.19226868448282,-5.62563957349027,
6.52296405691939));
#76315=CARTESIAN_POINT('Ctrl Pts',(-4.53868033199722,-5.34730396741956,
6.50279043877826));
#76316=CARTESIAN_POINT('Ctrl Pts',(-4.68103265499013,-5.22314178804768,
6.49412764123343));
#76317=CARTESIAN_POINT('Ctrl Pts',(-5.11214575074516,-4.81532127200719,
6.46683842532445));
#76318=CARTESIAN_POINT('Ctrl Pts',(-5.3814778365187,-4.51232334275096,6.4482354747848));
#76319=CARTESIAN_POINT('Ctrl Pts',(-5.74107478481165,-4.02947288138569,
6.42092249097817));
#76320=CARTESIAN_POINT('Ctrl Pts',(-5.85224059235256,-3.86624792410868,
6.41202772809416));
#76321=CARTESIAN_POINT('Ctrl Pts',(-6.1352284528919,-3.4105067316652,6.38793998648474));
#76322=CARTESIAN_POINT('Ctrl Pts',(-6.29295321481477,-3.10987437749404,
6.37285457546544));
#76323=CARTESIAN_POINT('Ctrl Pts',(-6.48033931322618,-2.67951797885644,
6.35162781671172));
#76324=CARTESIAN_POINT('Ctrl Pts',(-6.529028545093,-2.55859320303073,6.34568988560134));
#76325=CARTESIAN_POINT('Ctrl Pts',(-6.73087075116901,-2.01394377636797,
6.31909105740829));
#76326=CARTESIAN_POINT('Ctrl Pts',(-6.84634643856867,-1.57738522833334,
6.29827911901619));
#76327=CARTESIAN_POINT('Ctrl Pts',(-6.94246099196424,-0.990304786190284,
6.27121013842236));
#76328=CARTESIAN_POINT('Ctrl Pts',(-6.9613798781732,-0.847147631325589,
6.26467194045431));
#76329=CARTESIAN_POINT('Ctrl Pts',(-6.99944632495622,-0.469686896284264,
6.24755607764817));
#76330=CARTESIAN_POINT('Ctrl Pts',(-7.0112560665116,-0.234827899798161,
6.23703396468846));
#76331=CARTESIAN_POINT('Ctrl Pts',(-7.01124999766219,0.000181057866101147,
6.2265076133824));
#76332=CARTESIAN_POINT('Ctrl Pts',(-7.01124999771049,0.000179177963096134,
6.22646564308964));
#76333=CARTESIAN_POINT('Ctrl Pts',(-7.01124490821585,0.199331566167948,
6.21742360468036));
#76334=CARTESIAN_POINT('Ctrl Pts',(-7.00275018852882,0.39844265281681,6.20838156627109));
#76335=CARTESIAN_POINT('Ctrl Pts',(-6.98580233730263,0.596818453666757,
6.19933952786181));
#76336=CARTESIAN_POINT('Ctrl Pts',(-6.98181057617832,0.643542300794496,
6.19720983856227));
#76337=CARTESIAN_POINT('Ctrl Pts',(-6.97735010198673,0.69022537353174,6.19508014926272));
#76338=CARTESIAN_POINT('Ctrl Pts',(-6.97242181091054,0.73685863857258,6.19295045996318));
#76339=CARTESIAN_POINT('Ctrl Pts',(-6.95268047751938,0.923658244776018,
6.1844195299041));
#76340=CARTESIAN_POINT('Ctrl Pts',(-6.92542456469802,1.1096960269454,6.17588859984501));
#76341=CARTESIAN_POINT('Ctrl Pts',(-6.89073711509391,1.29436029495933,6.16735766978593));
#76342=CARTESIAN_POINT('Ctrl Pts',(-6.85605668170207,1.47898721102849,6.1588284652736));
#76343=CARTESIAN_POINT('Ctrl Pts',(-6.81394776824682,1.66224086665267,6.15029926076127));
#76344=CARTESIAN_POINT('Ctrl Pts',(-6.76454471919494,1.84351872909168,6.14177005624894));
#76345=CARTESIAN_POINT('Ctrl Pts',(-6.71514635696827,2.02477939385422,6.13324166089499));
#76346=CARTESIAN_POINT('Ctrl Pts',(-6.65845532044975,2.20406434413078,6.12471326554103));
#76347=CARTESIAN_POINT('Ctrl Pts',(-6.59465630396905,2.38078449151143,6.11618487018707));
#76348=CARTESIAN_POINT('Ctrl Pts',(-6.58728817646199,2.40119384342299,6.11519992860232));
#76349=CARTESIAN_POINT('Ctrl Pts',(-6.57982529813203,2.42156900377658,6.11421498701756));
#76350=CARTESIAN_POINT('Ctrl Pts',(-6.57226799596304,2.44190907933527,6.1132300454328));
#76351=CARTESIAN_POINT('Ctrl Pts',(-6.57226799589878,2.4419090795082,6.65995074817407));
#76352=CARTESIAN_POINT('Ctrl Pts',(-6.58131771308462,2.41755224856329,6.66112978362918));
#76353=CARTESIAN_POINT('Ctrl Pts',(-6.59023229898885,2.39314438829913,6.66231065902376));
#76354=CARTESIAN_POINT('Ctrl Pts',(-6.68221482357477,2.13688688044955,6.67470135157294));
#76355=CARTESIAN_POINT('Ctrl Pts',(-6.75314634805076,1.90086630247217,6.68604193313713));
#76356=CARTESIAN_POINT('Ctrl Pts',(-6.88314653638676,1.36794965318498,6.71128068282838));
#76357=CARTESIAN_POINT('Ctrl Pts',(-6.93571747621243,1.06996312059661,6.72514149733374));
#76358=CARTESIAN_POINT('Ctrl Pts',(-6.99711562074584,0.513926255681263,
6.75055596579651));
#76359=CARTESIAN_POINT('Ctrl Pts',(-7.01125611619881,0.256978822438064,
6.76212942280701));
#76360=CARTESIAN_POINT('Ctrl Pts',(-7.011243385311,-0.278097192768184,6.78612673913558));
#76361=CARTESIAN_POINT('Ctrl Pts',(-6.99471080565663,-0.555778604460915,
6.79852182034323));
#76362=CARTESIAN_POINT('Ctrl Pts',(-6.94670341357092,-0.95760418852317,
6.81678288974097));
#76363=CARTESIAN_POINT('Ctrl Pts',(-6.92825614545814,-1.08303280228687,
6.82253801863334));
#76364=CARTESIAN_POINT('Ctrl Pts',(-6.88098492762266,-1.35331757087629,
6.8350771712644));
#76365=CARTESIAN_POINT('Ctrl Pts',(-6.8509641279571,-1.49790252529874,6.84186181752672));
#76366=CARTESIAN_POINT('Ctrl Pts',(-6.73191371868191,-1.99228551530236,
6.86525578795537));
#76367=CARTESIAN_POINT('Ctrl Pts',(-6.62046125839425,-2.33610047252772,
6.88183668462479));
#76368=CARTESIAN_POINT('Ctrl Pts',(-6.38270144433937,-2.91344748834885,
6.91019572887894));
#76369=CARTESIAN_POINT('Ctrl Pts',(-6.26871147363916,-3.15124004571073,
6.92204860411966));
#76370=CARTESIAN_POINT('Ctrl Pts',(-5.98440861800993,-3.66751690392067,
6.94847414748757));
#76371=CARTESIAN_POINT('Ctrl Pts',(-5.80750188670883,-3.94166734281123,
6.96298892029673));
#76372=CARTESIAN_POINT('Ctrl Pts',(-5.50457485250056,-4.34620613502314,
6.98592598315164));
#76373=CARTESIAN_POINT('Ctrl Pts',(-5.39149719422794,-4.48571154734406,
6.99415664389733));
#76374=CARTESIAN_POINT('Ctrl Pts',(-4.99586713817197,-4.93720677967955,
7.02175348051643));
#76375=CARTESIAN_POINT('Ctrl Pts',(-4.69060481405529,-5.22809140792073,
7.04110785646335));
#76376=CARTESIAN_POINT('Ctrl Pts',(-4.1191372564352,-5.68206207282254,7.07420965234174));
#76377=CARTESIAN_POINT('Ctrl Pts',(-3.86472648733112,-5.85807258089696,
7.0880609931667));
#76378=CARTESIAN_POINT('Ctrl Pts',(-3.37583837714098,-6.15055204011379,
7.11357863093797));
#76379=CARTESIAN_POINT('Ctrl Pts',(-3.14485841685916,-6.27179689551686,
7.12523247441315));
#76380=CARTESIAN_POINT('Ctrl Pts',(-2.73016450371685,-6.46079569246422,
7.14592460237187));
#76381=CARTESIAN_POINT('Ctrl Pts',(-2.54936288906152,-6.53425022622116,
7.1548778221625));
#76382=CARTESIAN_POINT('Ctrl Pts',(-1.9942397389208,-6.73322925932852,7.18199947573059));
#76383=CARTESIAN_POINT('Ctrl Pts',(-1.61215418065476,-6.83478887391636,
7.20013825169232));
#76384=CARTESIAN_POINT('Ctrl Pts',(-0.916971275615275,-6.9579979662812,
7.23217303126062));
#76385=CARTESIAN_POINT('Ctrl Pts',(-0.607107129938149,-6.99185220284239,
7.24613318124684));
#76386=CARTESIAN_POINT('Ctrl Pts',(-0.0462832116005817,-7.01555150281003,
7.2712762249153));
#76387=CARTESIAN_POINT('Ctrl Pts',(0.203833041020188,-7.01274223104484,
7.28245086030312));
#76388=CARTESIAN_POINT('Ctrl Pts',(0.605446245084778,-6.98672450007237,
7.30069266450485));
#76389=CARTESIAN_POINT('Ctrl Pts',(0.757267235247652,-6.97190281822153,
7.30766763574173));
#76390=CARTESIAN_POINT('Ctrl Pts',(1.3773468909258,-6.89087305560463,7.33637564536627));
#76391=CARTESIAN_POINT('Ctrl Pts',(1.83882822546788,-6.78232603573567,7.35815762439493));
#76392=CARTESIAN_POINT('Ctrl Pts',(2.56456417919663,-6.53204021135923,7.39294790552744));
#76393=CARTESIAN_POINT('Ctrl Pts',(2.83692688928799,-6.41844124762686,7.40616154980519));
#76394=CARTESIAN_POINT('Ctrl Pts',(3.33620385675422,-6.17219206857562,7.43109711662841));
#76395=CARTESIAN_POINT('Ctrl Pts',(3.56439790951083,-6.04328339588388,7.4428046961773));
#76396=CARTESIAN_POINT('Ctrl Pts',(3.9504264567158,-5.79572703475529,7.46362718872269));
#76397=CARTESIAN_POINT('Ctrl Pts',(4.11146756786985,-5.68261853786531,7.47265650678087));
#76398=CARTESIAN_POINT('Ctrl Pts',(4.57865974646798,-5.32421495768197,7.4997388599903));
#76399=CARTESIAN_POINT('Ctrl Pts',(4.86921806764402,-5.05985344130576,7.51776080969534));
#76400=CARTESIAN_POINT('Ctrl Pts',(5.35568038768731,-4.53633367375472,7.55018824509851));
#76401=CARTESIAN_POINT('Ctrl Pts',(5.55864972726014,-4.28521333430483,7.56464027532156));
#76402=CARTESIAN_POINT('Ctrl Pts',(5.88852487292474,-3.81401976693936,7.59040346364981));
#76403=CARTESIAN_POINT('Ctrl Pts',(6.02213921942784,-3.59934815944039,7.60170416789714));
#76404=CARTESIAN_POINT('Ctrl Pts',(6.23331121314428,-3.21526362284056,7.62160056012623));
#76405=CARTESIAN_POINT('Ctrl Pts',(6.31625313436411,-3.04910366744836,7.63011574732553));
#76406=CARTESIAN_POINT('Ctrl Pts',(6.56089479887711,-2.50606439460331,7.65750165480046));
#76407=CARTESIAN_POINT('Ctrl Pts',(6.69618263606603,-2.118218691752,7.67635253919336));
#76408=CARTESIAN_POINT('Ctrl Pts',(6.84524754917262,-1.5294347366303,7.70390446373839));
#76409=CARTESIAN_POINT('Ctrl Pts',(6.88558914207132,-1.33613186397445,7.71279771792521));
#76410=CARTESIAN_POINT('Ctrl Pts',(6.9610115280969,-0.879010034295987,7.73359977736443));
#76411=CARTESIAN_POINT('Ctrl Pts',(6.98933947644396,-0.61438809336215,7.74546272815319));
#76412=CARTESIAN_POINT('Ctrl Pts',(7.00952034532501,-0.209232550461513,
7.76370591127279));
#76413=CARTESIAN_POINT('Ctrl Pts',(7.01229805977016,-0.0694924325936259,
7.77001672636569));
#76414=CARTESIAN_POINT('Ctrl Pts',(7.01029982261131,0.129962593846073,7.77910349082552));
#76415=CARTESIAN_POINT('Ctrl Pts',(7.00893834569618,0.189676226231698,7.78183244713181));
#76416=CARTESIAN_POINT('Ctrl Pts',(7.00042140818598,0.428990637080506,7.79279647660735));
#76417=CARTESIAN_POINT('Ctrl Pts',(6.98712381965537,0.608303410428246,7.80107123281553));
#76418=CARTESIAN_POINT('Ctrl Pts',(6.93365284225106,1.08171419301939,7.82299107288664));
#76419=CARTESIAN_POINT('Ctrl Pts',(6.88167545139285,1.37411626381108,7.83659514747978));
#76420=CARTESIAN_POINT('Ctrl Pts',(6.75117296819582,1.9088391551483,7.86160471530203));
#76421=CARTESIAN_POINT('Ctrl Pts',(6.67767890774314,2.15188543722486,7.87302814017459));
#76422=CARTESIAN_POINT('Ctrl Pts',(6.49703095281132,2.64999206931696,7.89679526319872));
#76423=CARTESIAN_POINT('Ctrl Pts',(6.38763928098552,2.90377877040218,7.90910964409462));
#76424=CARTESIAN_POINT('Ctrl Pts',(6.20637761806247,3.2641542419812,7.92730094855199));
#76425=CARTESIAN_POINT('Ctrl Pts',(6.14610252911692,3.37627739555295,7.93307379655572));
#76426=CARTESIAN_POINT('Ctrl Pts',(5.92886033544775,3.75527286890485,7.95302480427029));
#76427=CARTESIAN_POINT('Ctrl Pts',(5.75729366458968,4.01335625066513,7.96731717573306));
#76428=CARTESIAN_POINT('Ctrl Pts',(5.42040930044206,4.45385306682423,7.99277546588871));
#76429=CARTESIAN_POINT('Ctrl Pts',(5.26148481795813,4.6405199072907,8.00395806909183));
#76430=CARTESIAN_POINT('Ctrl Pts',(4.88717717047649,5.0361610307667,8.02863737452834));
#76431=CARTESIAN_POINT('Ctrl Pts',(4.66749604956386,5.24041055144013,8.0420633623407));
#76432=CARTESIAN_POINT('Ctrl Pts',(4.23987599336553,5.58970738788746,8.06679456450268));
#76433=CARTESIAN_POINT('Ctrl Pts',(4.03584946575664,5.73875354140848,8.0780869697612));
#76434=CARTESIAN_POINT('Ctrl Pts',(3.66880549544993,5.97761502678099,8.09796571718949));
#76435=CARTESIAN_POINT('Ctrl Pts',(3.5094283338005,6.07255514015831,8.10647168292543));
#76436=CARTESIAN_POINT('Ctrl Pts',(2.98592573999628,6.35690374683526,8.13386390638225));
#76437=CARTESIAN_POINT('Ctrl Pts',(2.60886892619951,6.52072033891968,8.15273056674295));
#76438=CARTESIAN_POINT('Ctrl Pts',(2.03242699627514,6.71310843254059,8.18029770391176));
#76439=CARTESIAN_POINT('Ctrl Pts',(1.84264530607353,6.76766164683866,8.1891908756156));
#76440=CARTESIAN_POINT('Ctrl Pts',(1.39233669253338,6.87675479006558,8.20999433195249));
#76441=CARTESIAN_POINT('Ctrl Pts',(1.13050781126064,6.92461615575911,8.22185875462551));
#76442=CARTESIAN_POINT('Ctrl Pts',(0.727986095596016,6.9747525724049,8.24010091576521));
#76443=CARTESIAN_POINT('Ctrl Pts',(0.588894825797756,6.98787089403302,8.24640913248971));
#76444=CARTESIAN_POINT('Ctrl Pts',(0.389876360918287,7.00065661448197,8.25549430367158));
#76445=CARTESIAN_POINT('Ctrl Pts',(0.330203171120092,7.00372489481785,8.25822432272138));
#76446=CARTESIAN_POINT('Ctrl Pts',(0.0907604269257031,7.01296962793811,
8.26919552532952));
#76447=CARTESIAN_POINT('Ctrl Pts',(-0.0891772435494388,7.01298989936746,
8.27747641923897));
#76448=CARTESIAN_POINT('Ctrl Pts',(-0.565150720725934,6.99472057798788,
8.29939175734012));
#76449=CARTESIAN_POINT('Ctrl Pts',(-0.860371252053511,6.96457305164982,
8.31298521294926));
#76450=CARTESIAN_POINT('Ctrl Pts',(-1.40306090347226,6.87411216238591,8.33798388463364));
#76451=CARTESIAN_POINT('Ctrl Pts',(-1.65087661835399,6.81884209186505,8.34940683779166));
#76452=CARTESIAN_POINT('Ctrl Pts',(-2.16098979917076,6.67562648324292,8.37317322354868));
#76453=CARTESIAN_POINT('Ctrl Pts',(-2.42218295046466,6.58535444555105,8.38548733732131));
#76454=CARTESIAN_POINT('Ctrl Pts',(-2.79500325541901,6.43131274398579,8.40367846873569));
#76455=CARTESIAN_POINT('Ctrl Pts',(-2.91128953968702,6.37951560245342,8.40945143295155));
#76456=CARTESIAN_POINT('Ctrl Pts',(-3.30537631453778,6.19095821204386,8.4294037898352));
#76457=CARTESIAN_POINT('Ctrl Pts',(-3.5754929362007,6.03898385200246,8.44369743533632));
#76458=CARTESIAN_POINT('Ctrl Pts',(-4.03977230878579,5.73566757881892,8.46915686226971));
#76459=CARTESIAN_POINT('Ctrl Pts',(-4.23770488292853,5.59101990526327,8.48033934681214));
#76460=CARTESIAN_POINT('Ctrl Pts',(-4.66000845447045,5.24706998311381,8.50501880401818));
#76461=CARTESIAN_POINT('Ctrl Pts',(-4.87998564735673,5.04313055372814,8.51844505361271));
#76462=CARTESIAN_POINT('Ctrl Pts',(-5.26001709833127,4.64258456003735,8.54317600423241));
#76463=CARTESIAN_POINT('Ctrl Pts',(-5.42377063276552,4.45017745640206,8.55446789742397));
#76464=CARTESIAN_POINT('Ctrl Pts',(-5.68917123286956,4.10187046636537,8.57434555749507));
#76465=CARTESIAN_POINT('Ctrl Pts',(-5.79565890491001,3.94998056782896,8.58285095563357));
#76466=CARTESIAN_POINT('Ctrl Pts',(-6.1146255396035,3.45430278126104,8.60995325151693));
#76467=CARTESIAN_POINT('Ctrl Pts',(-6.303482117885,3.09628465607241,8.62853280010782));
#76468=CARTESIAN_POINT('Ctrl Pts',(-6.49976039695399,2.63077489275526,8.65145887612565));
#76469=CARTESIAN_POINT('Ctrl Pts',(-6.53703987495371,2.53672368632034,8.65603465619411));
#76470=CARTESIAN_POINT('Ctrl Pts',(-6.57226798695174,2.4419091035887,8.66059774113391));
#76471=CARTESIAN_POINT('Origin',(0.,0.,10.));
#76472=CARTESIAN_POINT('',(-6.57243166141306,2.44196984210433,10.6603064506077));
#76473=CARTESIAN_POINT('',(-6.5722680052526,2.44190905433291,10.1130597871067));
#76474=CARTESIAN_POINT('',(-6.57226799596304,2.44190907933527,10.));
#76475=CARTESIAN_POINT('Ctrl Pts',(-6.5722680052526,2.44190905433291,10.1130597871067));
#76476=CARTESIAN_POINT('Ctrl Pts',(-6.52306249854838,2.57434305175004,10.1065737603578));
#76477=CARTESIAN_POINT('Ctrl Pts',(-6.46985951358318,2.70527517963783,10.1001055101174));
#76478=CARTESIAN_POINT('Ctrl Pts',(-6.32488472488106,3.03326103144295,10.0837545771268));
#76479=CARTESIAN_POINT('Ctrl Pts',(-6.22784833295103,3.22780835883114,10.0739189085502));
#76480=CARTESIAN_POINT('Ctrl Pts',(-5.9748362847281,3.68103613936886,10.0505463449007));
#76481=CARTESIAN_POINT('Ctrl Pts',(-5.81088110802064,3.93476256014785,10.03708876919));
#76482=CARTESIAN_POINT('Ctrl Pts',(-5.53767751847233,4.30306143336315,10.016498894731));
#76483=CARTESIAN_POINT('Ctrl Pts',(-5.44006918617429,4.42581704400765,10.0094359335946));
#76484=CARTESIAN_POINT('Ctrl Pts',(-5.19933764260226,4.70856117751045,9.9925424234154));
#76485=CARTESIAN_POINT('Ctrl Pts',(-5.05282373972641,4.86545277012714,9.98267705736606));
#76486=CARTESIAN_POINT('Ctrl Pts',(-4.73235369833136,5.17850889803249,9.96206347538926));
#76487=CARTESIAN_POINT('Ctrl Pts',(-4.55731367266609,5.33319977309406,9.95132800918116));
#76488=CARTESIAN_POINT('Ctrl Pts',(-4.29653885739566,5.54142866301973,9.93607606030169));
#76489=CARTESIAN_POINT('Ctrl Pts',(-4.21686177588699,5.60229906250303,9.93150689483303));
#76490=CARTESIAN_POINT('Ctrl Pts',(-3.77470075403087,5.92531520321396,9.90662465693136));
#76491=CARTESIAN_POINT('Ctrl Pts',(-3.38907093348138,6.15401727778345,9.88669807223162));
#76492=CARTESIAN_POINT('Ctrl Pts',(-2.83386247311823,6.41517605053325,9.85916513346686));
#76493=CARTESIAN_POINT('Ctrl Pts',(-2.68097131019242,6.48055955191551,9.85168435875302));
#76494=CARTESIAN_POINT('Ctrl Pts',(-2.31131340663199,6.62332043371386,9.83366594610008));
#76495=CARTESIAN_POINT('Ctrl Pts',(-2.09277764516773,6.69558233159228,9.82308374159923));
#76496=CARTESIAN_POINT('Ctrl Pts',(-1.64838554617929,6.81864000392244,9.80186601458179));
#76497=CARTESIAN_POINT('Ctrl Pts',(-1.42276758996983,6.86926201646625,9.79124371790561));
#76498=CARTESIAN_POINT('Ctrl Pts',(-1.0964457643642,6.92570929457335,9.77611496619395));
#76499=CARTESIAN_POINT('Ctrl Pts',(-0.997475895118887,6.9406544812964,9.77155613742358));
#76500=CARTESIAN_POINT('Ctrl Pts',(-0.480303663538549,7.00746051789475,
9.74787252662963));
#76501=CARTESIAN_POINT('Ctrl Pts',(-0.0583710251337542,7.02365946094005,
9.72907936535576));
#76502=CARTESIAN_POINT('Ctrl Pts',(0.541417106205394,6.99261079667883,9.70214524135545));
#76503=CARTESIAN_POINT('Ctrl Pts',(0.719951963275518,6.97648951629683,9.69409064615829));
#76504=CARTESIAN_POINT('Ctrl Pts',(1.14176797158952,6.92203503604771,9.67476117077906));
#76505=CARTESIAN_POINT('Ctrl Pts',(1.38403433580727,6.87769216829246,9.66343315709252));
#76506=CARTESIAN_POINT('Ctrl Pts',(1.84176431974649,6.76874329954472,9.64178304383793));
#76507=CARTESIAN_POINT('Ctrl Pts',(2.05744675854432,6.70633255035689,9.63147209869686));
#76508=CARTESIAN_POINT('Ctrl Pts',(2.36443991445152,6.60129252397757,9.61665346488913));
#76509=CARTESIAN_POINT('Ctrl Pts',(2.45841029581005,6.56687582930091,9.61209676286884));
#76510=CARTESIAN_POINT('Ctrl Pts',(2.92769925970198,6.38351300008897,9.58922060570921));
#76511=CARTESIAN_POINT('Ctrl Pts',(3.29039064335857,6.20435295804079,9.5711984704639));
#76512=CARTESIAN_POINT('Ctrl Pts',(3.79754115590281,5.89679217765715,9.54460903757734));
#76513=CARTESIAN_POINT('Ctrl Pts',(3.9553922990875,5.79209346990283,9.53610539920755));
#76514=CARTESIAN_POINT('Ctrl Pts',(4.31626357768206,5.53109788925574,9.51587089656991));
#76515=CARTESIAN_POINT('Ctrl Pts',(4.51534124354985,5.36981059708608,9.50408330018529));
#76516=CARTESIAN_POINT('Ctrl Pts',(4.9259522138198,4.99813192077069,9.47859969769539));
#76517=CARTESIAN_POINT('Ctrl Pts',(5.13379949899486,4.78439502432016,9.46493704518687));
#76518=CARTESIAN_POINT('Ctrl Pts',(5.48720921341611,4.37133488637111,9.44022600139232));
#76519=CARTESIAN_POINT('Ctrl Pts',(5.63706364942304,4.17630818388459,9.42915153440589));
#76520=CARTESIAN_POINT('Ctrl Pts',(5.90602258953739,3.78534718926906,9.40785548819564));
#76521=CARTESIAN_POINT('Ctrl Pts',(6.02637480900709,3.59064929418081,9.39763956176396));
#76522=CARTESIAN_POINT('Ctrl Pts',(6.21056442729317,3.25724776568287,9.38053113053101));
#76523=CARTESIAN_POINT('Ctrl Pts',(6.27977959979397,3.12172084876334,9.37367368227847));
#76524=CARTESIAN_POINT('Ctrl Pts',(6.45048108308314,2.75878414798111,9.35542208953705));
#76525=CARTESIAN_POINT('Ctrl Pts',(6.54435752457093,2.52803847623592,9.34395820172231));
#76526=CARTESIAN_POINT('Ctrl Pts',(6.72735503274035,1.99920825489445,9.31821125602443));
#76527=CARTESIAN_POINT('Ctrl Pts',(6.80932402937067,1.69919149110987,9.30396990429992));
#76528=CARTESIAN_POINT('Ctrl Pts',(6.9508579923896,1.00192342681966,9.27166721102043));
#76529=CARTESIAN_POINT('Ctrl Pts',(6.99676109633989,0.603006297637533,9.25377487970263));
#76530=CARTESIAN_POINT('Ctrl Pts',(7.01384654298695,0.0112696508311266,
9.22723807018616));
#76531=CARTESIAN_POINT('Ctrl Pts',(7.01154643762042,-0.179958336348825,
9.2186537642296));
#76532=CARTESIAN_POINT('Ctrl Pts',(6.98781153254607,-0.628059652340506,
9.19826715697476));
#76533=CARTESIAN_POINT('Ctrl Pts',(6.96002468049761,-0.884320427785898,
9.18640778524028));
#76534=CARTESIAN_POINT('Ctrl Pts',(6.86997095384255,-1.43155621023386,9.16088988512966));
#76535=CARTESIAN_POINT('Ctrl Pts',(6.8031628425897,-1.72128862521069,9.14726442991084));
#76536=CARTESIAN_POINT('Ctrl Pts',(6.58252384264637,-2.460250458762,9.11220892700226));
#76537=CARTESIAN_POINT('Ctrl Pts',(6.40112923711657,-2.8996551433947,9.09111831115912));
#76538=CARTESIAN_POINT('Ctrl Pts',(6.10470015985463,-3.45158941117204,9.06297879121011));
#76539=CARTESIAN_POINT('Ctrl Pts',(6.02826775626454,-3.58340909283533,9.05611263840986));
#76540=CARTESIAN_POINT('Ctrl Pts',(5.81548979845143,-3.9242771284782,9.03782709248574));
#76541=CARTESIAN_POINT('Ctrl Pts',(5.67217631503019,-4.12871483491063,9.02633746418278));
#76542=CARTESIAN_POINT('Ctrl Pts',(5.3265045558147,-4.56975016447565,9.00055562000652));
#76543=CARTESIAN_POINT('Ctrl Pts',(5.11867186270924,-4.80140310835969,8.9863052672367));
#76544=CARTESIAN_POINT('Ctrl Pts',(4.61111094785965,-5.29658982754405,8.95411204565464));
#76545=CARTESIAN_POINT('Ctrl Pts',(4.30289684196993,-5.5498911523295,8.93633320629322));
#76546=CARTESIAN_POINT('Ctrl Pts',(3.81603612646447,-5.88495211316567,8.90984107205694));
#76547=CARTESIAN_POINT('Ctrl Pts',(3.65278628473325,-5.98764924688596,8.90118498275196));
#76548=CARTESIAN_POINT('Ctrl Pts',(3.26088112457885,-6.21219008742089,8.88066544492403));
#76549=CARTESIAN_POINT('Ctrl Pts',(3.02929355460453,-6.32835121935764,8.86874470152901));
#76550=CARTESIAN_POINT('Ctrl Pts',(2.51997388677688,-6.54944131925157,8.84319749054508));
#76551=CARTESIAN_POINT('Ctrl Pts',(2.24091891656945,-6.65009304239442,8.82960383781908));
#76552=CARTESIAN_POINT('Ctrl Pts',(1.50138084998935,-6.86497899366382,8.79459775666959));
#76553=CARTESIAN_POINT('Ctrl Pts',(1.03420446707213,-6.95071975838244,8.77352440681931));
#76554=CARTESIAN_POINT('Ctrl Pts',(0.410061592315048,-7.00090695148839,
8.74540036509224));
#76555=CARTESIAN_POINT('Ctrl Pts',(0.257809106965031,-7.0081654146418,8.73853201614708));
#76556=CARTESIAN_POINT('Ctrl Pts',(-0.144162428614273,-7.01421124997964,
8.72023791696903));
#76557=CARTESIAN_POINT('Ctrl Pts',(-0.393785461806843,-7.00463225536466,
8.70874180757832));
#76558=CARTESIAN_POINT('Ctrl Pts',(-0.949724728195507,-6.95348264739962,
8.68305525776462));
#76559=CARTESIAN_POINT('Ctrl Pts',(-1.25488927211388,-6.90493713606302,
8.66890556627461));
#76560=CARTESIAN_POINT('Ctrl Pts',(-1.95229047918078,-6.74621986211733,
8.63642989490286));
#76561=CARTESIAN_POINT('Ctrl Pts',(-2.34011993582507,-6.62168892721861,
8.6182856313818));
#76562=CARTESIAN_POINT('Ctrl Pts',(-2.88798771241883,-6.39158579860027,
8.59164522398319));
#76563=CARTESIAN_POINT('Ctrl Pts',(-3.05801587784929,-6.31200278752193,
8.58321611055528));
#76564=CARTESIAN_POINT('Ctrl Pts',(-3.45066283957357,-6.1086284815956,8.56312478075359));
#76565=CARTESIAN_POINT('Ctrl Pts',(-3.67013647425846,-5.97934039092137,
8.55140622656641));
#76566=CARTESIAN_POINT('Ctrl Pts',(-4.13073579231001,-5.67307736553466,
8.52595562911345));
#76567=CARTESIAN_POINT('Ctrl Pts',(-4.368569225362,-5.49202995873933,8.5122571872988));
#76568=CARTESIAN_POINT('Ctrl Pts',(-4.77954508892193,-5.13554440964608,
8.48752615733592));
#76569=CARTESIAN_POINT('Ctrl Pts',(-4.95638245587944,-4.96509250449275,
8.47646651286933));
#76570=CARTESIAN_POINT('Ctrl Pts',(-5.28145399943499,-4.61704846891906,
8.45509367418528));
#76571=CARTESIAN_POINT('Ctrl Pts',(-5.43056447597842,-4.44070511060848,
8.44478727944677));
#76572=CARTESIAN_POINT('Ctrl Pts',(-5.66258984337376,-4.13710052436134,
8.42762300383097));
#76573=CARTESIAN_POINT('Ctrl Pts',(-5.75055568861366,-4.01392988718079,
8.42080180513171));
#76574=CARTESIAN_POINT('Ctrl Pts',(-5.97122053793642,-3.68279332144224,
8.40269256413441));
#76575=CARTESIAN_POINT('Ctrl Pts',(-6.09704987474239,-3.47050745435505,
8.39133683572029));
#76576=CARTESIAN_POINT('Ctrl Pts',(-6.35313379357093,-2.98138391713033,
8.36593423935645));
#76577=CARTESIAN_POINT('Ctrl Pts',(-6.47699679207328,-2.70175448959318,
8.35192629616431));
#76578=CARTESIAN_POINT('Ctrl Pts',(-6.73998857089557,-1.98493568398216,
8.3172457257361));
#76579=CARTESIAN_POINT('Ctrl Pts',(-6.8552346756514,-1.54051160563081,8.29686619026766));
#76580=CARTESIAN_POINT('Ctrl Pts',(-6.9502696003491,-0.935526679806157,
8.26936414495472));
#76581=CARTESIAN_POINT('Ctrl Pts',(-6.96918215409512,-0.782276873447443,
8.26240806471864));
#76582=CARTESIAN_POINT('Ctrl Pts',(-7.00182587171905,-0.419600882761046,
8.24583967508274));
#76583=CARTESIAN_POINT('Ctrl Pts',(-7.01124487977592,-0.209937821647998,
8.23619565108158));
#76584=CARTESIAN_POINT('Ctrl Pts',(-7.01125830046331,0.34010878522083,8.2108872257868));
#76585=CARTESIAN_POINT('Ctrl Pts',(-6.98649416202547,0.679943913064139,
8.19526116620574));
#76586=CARTESIAN_POINT('Ctrl Pts',(-6.89996407488868,1.27039215559498,8.16814954332841));
#76587=CARTESIAN_POINT('Ctrl Pts',(-6.84888113152541,1.52191686087706,8.15660574827463));
#76588=CARTESIAN_POINT('Ctrl Pts',(-6.72480522780128,1.99745896547295,8.13456370998852));
#76589=CARTESIAN_POINT('Ctrl Pts',(-6.65409201294924,2.22168410121299,8.12407245122135));
#76590=CARTESIAN_POINT('Ctrl Pts',(-6.57226800401825,2.44190905765509,8.11350492783088));
#76591=CARTESIAN_POINT('',(-7.01100200678231,0.000169534895841095,8.77353435691038));
#76592=CARTESIAN_POINT('Ctrl Pts',(-6.57226798695174,2.4419091035887,8.66059774113391));
#76593=CARTESIAN_POINT('Ctrl Pts',(-6.60582227508257,2.35159952843576,8.66494401625771));
#76594=CARTESIAN_POINT('Ctrl Pts',(-6.63751550112601,2.26059739590921,8.66927879456213));
#76595=CARTESIAN_POINT('Ctrl Pts',(-6.78113365131024,1.8191190086922,8.6901281620384));
#76596=CARTESIAN_POINT('Ctrl Pts',(-6.8672279976668,1.4608691468603,8.70647653024955));
#76597=CARTESIAN_POINT('Ctrl Pts',(-6.93320891013727,1.04456516083428,8.72558511308945));
#76598=CARTESIAN_POINT('Ctrl Pts',(-6.94099522164981,0.991507640171676,
8.72802374985079));
#76599=CARTESIAN_POINT('Ctrl Pts',(-6.99016893737213,0.62739884410733,8.74477747392914));
#76600=CARTESIAN_POINT('Ctrl Pts',(-7.01124211628482,0.313964344255776,
8.75926542393631));
#76601=CARTESIAN_POINT('Ctrl Pts',(-7.01124999778838,0.000176103450165235,
8.77367723833414));
#76602=CARTESIAN_POINT('Ctrl Pts',(-7.01100200678231,0.000169534895841095,
8.77353435691038));
#76603=CARTESIAN_POINT('Ctrl Pts',(-7.01026859459823,-0.814242395437865,
8.81050553539818));
#76604=CARTESIAN_POINT('Ctrl Pts',(-6.66540157732887,-2.79524324339015,
8.90040791439849));
#76605=CARTESIAN_POINT('Ctrl Pts',(-4.83841745661552,-5.47793893682926,
9.0432414939113));
#76606=CARTESIAN_POINT('Ctrl Pts',(-1.62793640627636,-7.12516115868475,
9.20203509544883));
#76607=CARTESIAN_POINT('Ctrl Pts',(1.97935012394701,-7.03564293913092,9.36082869698635));
#76608=CARTESIAN_POINT('Ctrl Pts',(5.10417494819451,-5.23120412317588,9.51962229852384));
#76609=CARTESIAN_POINT('Ctrl Pts',(6.98486973030968,-2.15167221730337,9.67841590006139));
#76610=CARTESIAN_POINT('Ctrl Pts',(7.16301976032167,1.45232447936148,9.83720950159888));
#76611=CARTESIAN_POINT('Ctrl Pts',(5.59520140824282,4.70232066976576,9.99600310313642));
#76612=CARTESIAN_POINT('Ctrl Pts',(2.66356652666938,6.80613780628324,10.1547967046739));
#76613=CARTESIAN_POINT('Ctrl Pts',(-0.917306119809289,7.25097565591498,
10.3135903062114));
#76614=CARTESIAN_POINT('Ctrl Pts',(-4.27458766428332,5.92840609105567,10.472383907749));
#76615=CARTESIAN_POINT('Ctrl Pts',(-5.95973776688883,3.91410797347048,10.5879559558811));
#76616=CARTESIAN_POINT('Ctrl Pts',(-6.49815987240321,2.64250790562492,10.6505968035006));
#76617=CARTESIAN_POINT('Ctrl Pts',(-6.57243166141306,2.44196984210433,10.6603064506077));
#76618=CARTESIAN_POINT('Origin',(0.,0.,10.));
#76619=CARTESIAN_POINT('',(-6.57226799596304,2.44190907933527,12.6602932967));
#76620=CARTESIAN_POINT('',(-6.57226802086842,2.44190901230376,12.1131304899038));
#76621=CARTESIAN_POINT('',(-6.57226799596304,2.44190907933527,10.));
#76622=CARTESIAN_POINT('',(-7.01124982808863,8.84455196530982E-5,10.2261740575975));
#76623=CARTESIAN_POINT('Ctrl Pts',(-6.57226802086842,2.44190901230376,12.1131304899038));
#76624=CARTESIAN_POINT('Ctrl Pts',(-6.54688037716058,2.510238502889,12.1098623793163));
#76625=CARTESIAN_POINT('Ctrl Pts',(-6.52042381490871,2.57818101884485,12.1065967925351));
#76626=CARTESIAN_POINT('Ctrl Pts',(-6.39754489276982,2.87974127567772,12.0920113248996));
#76627=CARTESIAN_POINT('Ctrl Pts',(-6.28960118708034,3.10844066455065,12.0807090018542));
#76628=CARTESIAN_POINT('Ctrl Pts',(-6.08133977191838,3.49419657965324,12.0608091758205));
#76629=CARTESIAN_POINT('Ctrl Pts',(-5.98667559978145,3.65401373965553,12.0522921980193));
#76630=CARTESIAN_POINT('Ctrl Pts',(-5.66304324527052,4.15398440660527,12.0249075181839));
#76631=CARTESIAN_POINT('Ctrl Pts',(-5.41055224263107,4.47789936037004,12.0060596981926));
#76632=CARTESIAN_POINT('Ctrl Pts',(-4.99670412879478,4.92235030328896,11.9785107312699));
#76633=CARTESIAN_POINT('Ctrl Pts',(-4.85615757561548,5.06105916070442,11.969617463602));
#76634=CARTESIAN_POINT('Ctrl Pts',(-4.51296656268245,5.37228717321997,11.9488156792853));
#76635=CARTESIAN_POINT('Ctrl Pts',(-4.30598638440878,5.53956828976701,11.9369530156526));
#76636=CARTESIAN_POINT('Ctrl Pts',(-3.97649833014791,5.7762113863267,11.9187096344546));
#76637=CARTESIAN_POINT('Ctrl Pts',(-3.860579971078,5.85432137669194,11.9123983137699));
#76638=CARTESIAN_POINT('Ctrl Pts',(-3.69190062837516,5.96079383079722,11.9033112408894));
#76639=CARTESIAN_POINT('Ctrl Pts',(-3.64099253422944,5.99202525316997,11.9005824929819));
#76640=CARTESIAN_POINT('Ctrl Pts',(-3.43531952709893,6.11461391166622,11.8896198684564));
#76641=CARTESIAN_POINT('Ctrl Pts',(-3.27746717410528,6.20065576499953,11.8813463141605));
#76642=CARTESIAN_POINT('Ctrl Pts',(-2.85068187444628,6.41243220611299,11.8594255952862));
#76643=CARTESIAN_POINT('Ctrl Pts',(-2.57677013962033,6.52732217601357,11.8458194439498));
#76644=CARTESIAN_POINT('Ctrl Pts',(-2.05666919306168,6.70761628081339,11.8208077533866));
#76645=CARTESIAN_POINT('Ctrl Pts',(-1.8126002273792,6.7776461931263,11.8093842442754));
#76646=CARTESIAN_POINT('Ctrl Pts',(-1.29611754215166,6.89593714449807,11.7856169877211));
#76647=CARTESIAN_POINT('Ctrl Pts',(-1.0235606759597,6.9416273948252,11.7733025572706));
#76648=CARTESIAN_POINT('Ctrl Pts',(-0.622475285271074,6.98472264459883,
11.7551112226141));
#76649=CARTESIAN_POINT('Ctrl Pts',(-0.495583421257757,6.99487114048289,
11.7493383980851));
#76650=CARTESIAN_POINT('Ctrl Pts',(-0.0593498600627373,7.01782969787626,
11.7293876408584));
#76651=CARTESIAN_POINT('Ctrl Pts',(0.250523006141232,7.0136077617466,11.715095503905));
#76652=CARTESIAN_POINT('Ctrl Pts',(0.803304932241008,6.96938630858188,11.6896374249949));
#76653=CARTESIAN_POINT('Ctrl Pts',(1.04632136718118,6.93706417033835,11.6784548019303));
#76654=CARTESIAN_POINT('Ctrl Pts',(1.58170857792281,6.83707654822773,11.6537755424015));
#76655=CARTESIAN_POINT('Ctrl Pts',(1.87243985733845,6.76323814672692,11.6403496183861));
#76656=CARTESIAN_POINT('Ctrl Pts',(2.39779553592898,6.59332655335917,11.6156183615674));
#76657=CARTESIAN_POINT('Ctrl Pts',(2.63365842278843,6.50270849579327,11.604325838146));
#76658=CARTESIAN_POINT('Ctrl Pts',(3.03338002602547,6.32381385964298,11.5844468525831));
#76659=CARTESIAN_POINT('Ctrl Pts',(3.19957102729586,6.24137479594769,11.5759407688705));
#76660=CARTESIAN_POINT('Ctrl Pts',(3.72233968819918,5.95568311434478,11.548548631502));
#76661=CARTESIAN_POINT('Ctrl Pts',(4.06442595428536,5.72768965777138,11.5296821782738));
#76662=CARTESIAN_POINT('Ctrl Pts',(4.53862858620379,5.34765695030548,11.5021152436343));
#76663=CARTESIAN_POINT('Ctrl Pts',(4.68736831651953,5.21777386773328,11.4932220736018));
#76664=CARTESIAN_POINT('Ctrl Pts',(5.02319521206397,4.89855769729015,11.4724186402161));
#76665=CARTESIAN_POINT('Ctrl Pts',(5.20537674174289,4.70450948948079,11.4605542387343));
#76666=CARTESIAN_POINT('Ctrl Pts',(5.46575576958667,4.39347826842278,11.4423120647569));
#76667=CARTESIAN_POINT('Ctrl Pts',(5.55219576982442,4.28372024148265,11.4360038125229));
#76668=CARTESIAN_POINT('Ctrl Pts',(5.67084927962669,4.12342879355375,11.4269186217153));
#76669=CARTESIAN_POINT('Ctrl Pts',(5.70578267369711,4.07495283090559,11.4241886193547));
#76670=CARTESIAN_POINT('Ctrl Pts',(5.84337779263442,3.87877760274942,11.4132175281794));
#76671=CARTESIAN_POINT('Ctrl Pts',(5.9409581141614,3.72759920816807,11.4049367294474));
#76672=CARTESIAN_POINT('Ctrl Pts',(6.1836870029801,3.31775954576857,11.3830213258525));
#76673=CARTESIAN_POINT('Ctrl Pts',(6.31842947375525,3.05335348781755,11.3694277098683));
#76674=CARTESIAN_POINT('Ctrl Pts',(6.53667426233892,2.54831071221083,11.3444288829191));
#76675=CARTESIAN_POINT('Ctrl Pts',(6.6246024980283,2.31011748703655,11.3330059317448));
#76676=CARTESIAN_POINT('Ctrl Pts',(6.78085586132641,1.80384579524083,11.3092395472092));
#76677=CARTESIAN_POINT('Ctrl Pts',(6.84662738764625,1.53543376379101,11.2969254326983));
#76678=CARTESIAN_POINT('Ctrl Pts',(6.9193424539647,1.1386513077578,11.2787343027459));
#76679=CARTESIAN_POINT('Ctrl Pts',(6.93887204987628,1.01285772368272,11.2729613408046));
#76680=CARTESIAN_POINT('Ctrl Pts',(6.99411650599425,0.579491538137023,11.2530089878428));
#76681=CARTESIAN_POINT('Ctrl Pts',(7.01288154990812,0.270125983085059,11.2387153439766));
#76682=CARTESIAN_POINT('Ctrl Pts',(7.00976000242406,-0.284442560050966,
11.2132559204942));
#76683=CARTESIAN_POINT('Ctrl Pts',(6.99554223374986,-0.529183419687476,
11.2020734377709));
#76684=CARTESIAN_POINT('Ctrl Pts',(6.93551887943285,-1.07051382935617,11.177393998748));
#76685=CARTESIAN_POINT('Ctrl Pts',(6.88343461022993,-1.36592585795191,11.1639677651249));
#76686=CARTESIAN_POINT('Ctrl Pts',(6.7529364207787,-1.90242509710265,11.1392368058035));
#76687=CARTESIAN_POINT('Ctrl Pts',(6.68005675044703,-2.1443435737848,11.1279448879996));
#76688=CARTESIAN_POINT('Ctrl Pts',(6.53129745292929,-2.55620115303456,11.1080671884675));
#76689=CARTESIAN_POINT('Ctrl Pts',(6.46141185244808,-2.72803328700361,11.0995617760702));
#76690=CARTESIAN_POINT('Ctrl Pts',(6.21526106737558,-3.27055412443705,11.0721691776359));
#76691=CARTESIAN_POINT('Ctrl Pts',(6.01324377531958,-3.6286232593302,11.0533015746088));
#76692=CARTESIAN_POINT('Ctrl Pts',(5.6693958452331,-4.12971367414453,11.0257335311834));
#76693=CARTESIAN_POINT('Ctrl Pts',(5.55089638603365,-4.28767246413541,11.0168403670962));
#76694=CARTESIAN_POINT('Ctrl Pts',(5.25745219872648,-4.6462409890206,10.9960368316422));
#76695=CARTESIAN_POINT('Ctrl Pts',(5.07744145015366,-4.84230793918049,10.9841723226927));
#76696=CARTESIAN_POINT('Ctrl Pts',(4.78656922893734,-5.12502597446008,10.9659302231568));
#76697=CARTESIAN_POINT('Ctrl Pts',(4.68352425510897,-5.21936167744688,10.9596221604644));
#76698=CARTESIAN_POINT('Ctrl Pts',(4.53247185432463,-5.3495696702889,10.950537085712));
#76699=CARTESIAN_POINT('Ctrl Pts',(4.48671765610269,-5.38800161170629,10.947807005657));
#76700=CARTESIAN_POINT('Ctrl Pts',(4.30127349055091,-5.53976800604108,10.9368353899342));
#76701=CARTESIAN_POINT('Ctrl Pts',(4.15773684077934,-5.64829239824263,10.9285541423525));
#76702=CARTESIAN_POINT('Ctrl Pts',(3.76702328059213,-5.92072960200588,10.9066390675196));
#76703=CARTESIAN_POINT('Ctrl Pts',(3.513347622996,-6.07469316738086,10.8930462276176));
#76704=CARTESIAN_POINT('Ctrl Pts',(3.02588949854575,-6.32977015746142,10.8680481966715));
#76705=CARTESIAN_POINT('Ctrl Pts',(2.79487091834758,-6.43511439030879,10.8566252796366));
#76706=CARTESIAN_POINT('Ctrl Pts',(2.30157723395587,-6.62846949614994,10.8328589484629));
#76707=CARTESIAN_POINT('Ctrl Pts',(2.03878015831692,-6.71395849365647,10.8205448532881));
#76708=CARTESIAN_POINT('Ctrl Pts',(1.64848046451444,-6.81588871745719,10.8023537358482));
#76709=CARTESIAN_POINT('Ctrl Pts',(1.52448064134744,-6.84469027216798,10.7965807654815));
#76710=CARTESIAN_POINT('Ctrl Pts',(1.09640033669328,-6.93191053547969,10.7766283148612));
#76711=CARTESIAN_POINT('Ctrl Pts',(0.789275225705136,-6.97355874183667,
10.7623345787885));
#76712=CARTESIAN_POINT('Ctrl Pts',(0.235999473876122,-7.01155810215142,
10.7368750730369));
#76713=CARTESIAN_POINT('Ctrl Pts',(-0.00912176680378921,-7.01552299826439,
10.7256925989047));
#76714=CARTESIAN_POINT('Ctrl Pts',(-0.553412606382337,-6.99579564682385,
10.7010131488923));
#76715=CARTESIAN_POINT('Ctrl Pts',(-0.851873382630387,-6.96575462400956,
10.6875868963149));
#76716=CARTESIAN_POINT('Ctrl Pts',(-1.39657024243448,-6.87538818450214,
10.6628559552064));
#76717=CARTESIAN_POINT('Ctrl Pts',(-1.64322505556015,-6.82064355797329,
10.6515640744785));
#76718=CARTESIAN_POINT('Ctrl Pts',(-2.0649757731466,-6.7028266784728,10.6316864536703));
#76719=CARTESIAN_POINT('Ctrl Pts',(-2.241515136561,-6.64587227581451,10.6231810823639));
#76720=CARTESIAN_POINT('Ctrl Pts',(-2.80079190623852,-6.44061801051559,
10.5957884557022));
#76721=CARTESIAN_POINT('Ctrl Pts',(-3.17285346079602,-6.26570104768405,
10.5769207822906));
#76722=CARTESIAN_POINT('Ctrl Pts',(-3.69805703859718,-5.95994617579252,
10.549352670991));
#76723=CARTESIAN_POINT('Ctrl Pts',(-3.86436596968462,-5.85348285204863,
10.5404595072674));
#76724=CARTESIAN_POINT('Ctrl Pts',(-4.24370203358389,-5.58742803797586,
10.5196559655641));
#76725=CARTESIAN_POINT('Ctrl Pts',(-4.45257443430411,-5.422447680154,10.5077914500351));
#76726=CARTESIAN_POINT('Ctrl Pts',(-4.75607783328552,-5.15333482244536,
10.4895493550559));
#76727=CARTESIAN_POINT('Ctrl Pts',(-4.85779286038752,-5.05756702575083,
10.483241303967));
#76728=CARTESIAN_POINT('Ctrl Pts',(-4.99884051926767,-4.91658318781238,
10.4741562363185));
#76729=CARTESIAN_POINT('Ctrl Pts',(-5.04055870617977,-4.87380391841118,
10.4714261515064));
#76730=CARTESIAN_POINT('Ctrl Pts',(-5.20565561878988,-4.70012052963085,
10.4604545036656));
#76731=CARTESIAN_POINT('Ctrl Pts',(-5.32452265652367,-4.56502369617191,
10.4521732286008));
#76732=CARTESIAN_POINT('Ctrl Pts',(-5.62112227210478,-4.2005620928327,10.4305535735194));
#76733=CARTESIAN_POINT('Ctrl Pts',(-5.7900515260717,-3.96447293077758,10.4172532673156));
#76734=CARTESIAN_POINT('Ctrl Pts',(-6.05025523930506,-3.54855865402196,
10.3949528946717));
#76735=CARTESIAN_POINT('Ctrl Pts',(-6.14929087420723,-3.3740303049451,10.3858983310391));
#76736=CARTESIAN_POINT('Ctrl Pts',(-6.37408834214991,-2.93500734957092,
10.3637259735005));
#76737=CARTESIAN_POINT('Ctrl Pts',(-6.49102774827429,-2.66642608209169,
10.3506794603042));
#76738=CARTESIAN_POINT('Ctrl Pts',(-6.63611703659724,-2.2665389844744,10.3315525730326));
#76739=CARTESIAN_POINT('Ctrl Pts',(-6.67783909290207,-2.1404936139626,10.3255617227238));
#76740=CARTESIAN_POINT('Ctrl Pts',(-6.74796060119245,-1.906587122782,10.3144495070837));
#76741=CARTESIAN_POINT('Ctrl Pts',(-6.77741310604404,-1.79908807295501,
10.3093488189413));
#76742=CARTESIAN_POINT('Ctrl Pts',(-6.89976228177878,-1.30675695056456,
10.286066241257));
#76743=CARTESIAN_POINT('Ctrl Pts',(-6.96252792258015,-0.915175995298078,
10.267808296208));
#76744=CARTESIAN_POINT('Ctrl Pts',(-7.00480120457911,-0.347201324706604,
10.2418684589118));
#76745=CARTESIAN_POINT('Ctrl Pts',(-7.01125219422837,-0.1735872788153,10.2340036335229));
#76746=CARTESIAN_POINT('Ctrl Pts',(-7.01124999944015,8.86030272035515E-5,
10.2261737535422));
#76747=CARTESIAN_POINT('Ctrl Pts',(-7.01124999944231,8.84321612436983E-5,
10.2261737612454));
#76748=CARTESIAN_POINT('Ctrl Pts',(-7.01124533029536,0.370276789916301,
10.2094844524627));
#76749=CARTESIAN_POINT('Ctrl Pts',(-6.98192239085777,0.739881399521689,
10.1930195260008));
#76750=CARTESIAN_POINT('Ctrl Pts',(-6.90640727853726,1.21284610091569,10.1714608011783));
#76751=CARTESIAN_POINT('Ctrl Pts',(-6.88676134899585,1.31983900532265,10.1665477865801));
#76752=CARTESIAN_POINT('Ctrl Pts',(-6.8068752874671,1.70431378819719,10.1486905702379));
#76753=CARTESIAN_POINT('Ctrl Pts',(-6.73228487181659,1.97852834723244,10.1356004187491));
#76754=CARTESIAN_POINT('Ctrl Pts',(-6.61922587762499,2.31261910254185,10.1193784660519));
#76755=CARTESIAN_POINT('Ctrl Pts',(-6.59622056257768,2.37744202355948,10.1162170948538));
#76756=CARTESIAN_POINT('Ctrl Pts',(-6.5722680052526,2.44190905433291,10.1130597871067));
#76757=CARTESIAN_POINT('',(-7.01124999902902,-0.00011668600800139,10.7735343569104));
#76758=CARTESIAN_POINT('Ctrl Pts',(-6.57243166141306,2.44196984210433,10.6603064506077));
#76759=CARTESIAN_POINT('Ctrl Pts',(-6.86113553316664,1.66245293340731,10.6980490814309));
#76760=CARTESIAN_POINT('Ctrl Pts',(-7.01103588237741,0.831054505111012,
10.735791712254));
#76761=CARTESIAN_POINT('Ctrl Pts',(-7.01168925918796,-0.000116388681771435,
10.7735343430772));
#76762=CARTESIAN_POINT('Ctrl Pts',(-7.01124999902902,-0.00011668600800139,
10.7735343569104));
#76763=CARTESIAN_POINT('Ctrl Pts',(-7.01124799109669,-0.120766245883287,
10.7790132748816));
#76764=CARTESIAN_POINT('Ctrl Pts',(-7.00813125367059,-0.241405380892823,
10.7844921928528));
#76765=CARTESIAN_POINT('Ctrl Pts',(-7.00190453737324,-0.361883146902471,
10.789971110824));
#76766=CARTESIAN_POINT('Ctrl Pts',(-6.99220925361489,-0.549472571609852,
10.7985020381833));
#76767=CARTESIAN_POINT('Ctrl Pts',(-6.97496935380637,-0.736704258608883,
10.8070329655426));
#76768=CARTESIAN_POINT('Ctrl Pts',(-6.95023495748845,-0.922962945196363,
10.8155638929019));
#76769=CARTESIAN_POINT('Ctrl Pts',(-6.92550525696389,-1.10918627081151,
10.8240932006755));
#76770=CARTESIAN_POINT('Ctrl Pts',(-6.89328393961082,-1.29443666124397,
10.8326225084492));
#76771=CARTESIAN_POINT('Ctrl Pts',(-6.85367284810497,-1.47810522414635,
10.8411518162229));
#76772=CARTESIAN_POINT('Ctrl Pts',(-6.81202562040045,-1.67121493585999,
10.8501195575678));
#76773=CARTESIAN_POINT('Ctrl Pts',(-6.76220895396378,-1.86257555729251,
10.8590872989127));
#76774=CARTESIAN_POINT('Ctrl Pts',(-6.70440205432244,-2.0514920561623,10.8680550402576));
#76775=CARTESIAN_POINT('Ctrl Pts',(-6.6494231153614,-2.23116660581882,10.8765840723814));
#76776=CARTESIAN_POINT('Ctrl Pts',(-6.58721713263291,-2.4086301375784,10.8851131045052));
#76777=CARTESIAN_POINT('Ctrl Pts',(-6.51798943486467,-2.583300270873,10.893642136629));
#76778=CARTESIAN_POINT('Ctrl Pts',(-6.44876104463667,-2.75797215133014,
10.9021712540656));
#76779=CARTESIAN_POINT('Ctrl Pts',(-6.37251091485545,-2.92985029402879,
10.9107003715023));
#76780=CARTESIAN_POINT('Ctrl Pts',(-6.28949269640831,-3.09837186023992,
10.9192294889389));
#76781=CARTESIAN_POINT('Ctrl Pts',(-6.20645768023238,-3.26692752474438,
10.927760332139));
#76782=CARTESIAN_POINT('Ctrl Pts',(-6.11665197635673,-3.43212498199062,
10.936291175339));
#76783=CARTESIAN_POINT('Ctrl Pts',(-6.02037580528256,-3.59342479059579,
10.944822018539));
#76784=CARTESIAN_POINT('Ctrl Pts',(-6.00554384178086,-3.61827406375831,
10.9461362498132));
#76785=CARTESIAN_POINT('Ctrl Pts',(-5.99055839931713,-3.64303088294956,
10.9474504810873));
#76786=CARTESIAN_POINT('Ctrl Pts',(-5.97542066998606,-3.66769333221895,
10.9487647123615));
#76787=CARTESIAN_POINT('Ctrl Pts',(-5.87715876445461,-3.8277820223575,10.9572956397208));
#76788=CARTESIAN_POINT('Ctrl Pts',(-5.77244288573805,-3.98394701045112,
10.96582656708));
#76789=CARTESIAN_POINT('Ctrl Pts',(-5.66161140464517,-4.13567199682128,
10.9743574944393));
#76790=CARTESIAN_POINT('Ctrl Pts',(-5.55080096476639,-4.28736817839798,
10.982886802213));
#76791=CARTESIAN_POINT('Ctrl Pts',(-5.43387742002723,-4.43462579325325,
10.9914161099866));
#76792=CARTESIAN_POINT('Ctrl Pts',(-5.31122151291524,-4.57695888153328,
10.9999454177603));
#76793=CARTESIAN_POINT('Ctrl Pts',(-5.1822607017228,-4.72660834364486,11.0089131591052));
#76794=CARTESIAN_POINT('Ctrl Pts',(-5.04696290758847,-4.87081338721959,
11.0178809004501));
#76795=CARTESIAN_POINT('Ctrl Pts',(-4.90581801919283,-5.00904942330009,
11.026848641795));
#76796=CARTESIAN_POINT('Ctrl Pts',(-4.7715780538619,-5.14052283974373,11.0353776739188));
#76797=CARTESIAN_POINT('Ctrl Pts',(-4.63204964690216,-5.2665970759815,11.0439067060426));
#76798=CARTESIAN_POINT('Ctrl Pts',(-4.48769173061396,-5.38685896357786,
11.0524357381664));
#76799=CARTESIAN_POINT('Ctrl Pts',(-4.34333237036528,-5.50712205411076,
11.060964855603));
#76800=CARTESIAN_POINT('Ctrl Pts',(-4.19414364159007,-5.62157248633174,
11.0694939730396));
#76801=CARTESIAN_POINT('Ctrl Pts',(-4.04061756016206,-5.72983737072965,
11.0780230904763));
#76802=CARTESIAN_POINT('Ctrl Pts',(-3.88706041459529,-5.83812416121257,
11.0865539336763));
#76803=CARTESIAN_POINT('Ctrl Pts',(-3.729164414304,-5.94022272839675,11.0950847768763));
#76804=CARTESIAN_POINT('Ctrl Pts',(-3.56745127519244,-6.03580300884877,
11.1036156200763));
#76805=CARTESIAN_POINT('Ctrl Pts',(-3.54253832580481,-6.05052776592441,
11.1049298513505));
#76806=CARTESIAN_POINT('Ctrl Pts',(-3.517534835176,-6.06509790795472,11.1062440826248));
#76807=CARTESIAN_POINT('Ctrl Pts',(-3.49244276676198,-6.0795123228259,11.107558313899));
#76808=CARTESIAN_POINT('Ctrl Pts',(-3.32956533633588,-6.17307905541145,
11.1160892412583));
#76809=CARTESIAN_POINT('Ctrl Pts',(-3.16289771561957,-6.26011251430186,
11.1246201686175));
#76810=CARTESIAN_POINT('Ctrl Pts',(-2.99298404964067,-6.34032120961522,
11.1331510959768));
#76811=CARTESIAN_POINT('Ctrl Pts',(-2.82310264155287,-6.42051467741086,
11.1416804037504));
#76812=CARTESIAN_POINT('Ctrl Pts',(-2.64997669479013,-6.49388583662647,
11.1502097115241));
#76813=CARTESIAN_POINT('Ctrl Pts',(-2.47417304661047,-6.56019011141646,
11.1587390192978));
#76814=CARTESIAN_POINT('Ctrl Pts',(-2.28933253127214,-6.62990263699949,
11.1677067606427));
#76815=CARTESIAN_POINT('Ctrl Pts',(-2.10153211272916,-6.6918024793668,11.1766745019876));
#76816=CARTESIAN_POINT('Ctrl Pts',(-1.91145295365878,-6.74566336014844,
11.1856422433325));
#76817=CARTESIAN_POINT('Ctrl Pts',(-1.73067262208771,-6.79688932271075,
11.1941712754562));
#76818=CARTESIAN_POINT('Ctrl Pts',(-1.54783149561706,-6.84084397960362,
11.20270030758));
#76819=CARTESIAN_POINT('Ctrl Pts',(-1.36353024650465,-6.87738408331009,
11.2112293397038));
#76820=CARTESIAN_POINT('Ctrl Pts',(-1.17922715389277,-6.91392455251415,
11.2197584571405));
#76821=CARTESIAN_POINT('Ctrl Pts',(-0.993464210436353,-6.94305026396572,
11.2282875745771));
#76822=CARTESIAN_POINT('Ctrl Pts',(-0.806851869341063,-6.96466916826929,
11.2368166920138));
#76823=CARTESIAN_POINT('Ctrl Pts',(-0.620201769504061,-6.98629244689569,
11.2453475352138));
#76824=CARTESIAN_POINT('Ctrl Pts',(-0.432702233044765,-7.00040585033402,
11.2538783784138));
#76825=CARTESIAN_POINT('Ctrl Pts',(-0.244969304306911,-7.00696914524728,
11.2624092216138));
#76826=CARTESIAN_POINT('Ctrl Pts',(-0.216047838940853,-7.00798026305063,
11.263723452888));
#76827=CARTESIAN_POINT('Ctrl Pts',(-0.187120839258501,-7.00881229177017,
11.2650376841623));
#76828=CARTESIAN_POINT('Ctrl Pts',(-0.158190561489543,-7.00946519420388,
11.2663519154365));
#76829=CARTESIAN_POINT('Ctrl Pts',(0.0296014222860561,-7.0137033091718,
11.2748828427958));
#76830=CARTESIAN_POINT('Ctrl Pts',(0.217595963931144,-7.01039104812785,
11.283413770155));
#76831=CARTESIAN_POINT('Ctrl Pts',(0.4051757782064,-6.9995327809258,11.2919446975143));
#76832=CARTESIAN_POINT('Ctrl Pts',(0.592719980695167,-6.98867657515181,
11.300474005288));
#76833=CARTESIAN_POINT('Ctrl Pts',(0.77984930738174,-6.97027723981227,11.3090033130616));
#76834=CARTESIAN_POINT('Ctrl Pts',(0.965948991419823,-6.94439119782829,
11.3175326208353));
#76835=CARTESIAN_POINT('Ctrl Pts',(1.16161479163565,-6.91717453088232,11.3265003621802));
#76836=CARTESIAN_POINT('Ctrl Pts',(1.35614194622031,-6.88168123828715,11.3354681035251));
#76837=CARTESIAN_POINT('Ctrl Pts',(1.5488240502208,-6.83803850705432,11.34443584487));
#76838=CARTESIAN_POINT('Ctrl Pts',(1.73207998853247,-6.79653081383059,11.3529648769938));
#76839=CARTESIAN_POINT('Ctrl Pts',(1.91366676134555,-6.74765205227895,11.3614939091175));
#76840=CARTESIAN_POINT('Ctrl Pts',(2.09298836882461,-6.69156381202966,11.3700229412413));
#76841=CARTESIAN_POINT('Ctrl Pts',(2.27231176999349,-6.63547501074978,11.3785520586779));
#76842=CARTESIAN_POINT('Ctrl Pts',(2.44936966928575,-6.57217668117308,11.3870811761146));
#76843=CARTESIAN_POINT('Ctrl Pts',(2.62358197262553,-6.50188005083256,11.3956102935512));
#76844=CARTESIAN_POINT('Ctrl Pts',(2.79782952570986,-6.43156919682232,11.4041411367512));
#76845=CARTESIAN_POINT('Ctrl Pts',(2.96923004923471,-6.35425732927099,11.4126719799512));
#76846=CARTESIAN_POINT('Ctrl Pts',(3.13722332970476,-6.27020385171457,11.4212028231512));
#76847=CARTESIAN_POINT('Ctrl Pts',(3.16310377527063,-6.25725487277663,11.4225170544255));
#76848=CARTESIAN_POINT('Ctrl Pts',(3.18890339925198,-6.24414598323843,11.4238312856998));
#76849=CARTESIAN_POINT('Ctrl Pts',(3.2146202025958,-6.23087822987763,11.4251455169741));
#76850=CARTESIAN_POINT('Ctrl Pts',(3.38155290730832,-6.14475469716764,11.4336764443334));
#76851=CARTESIAN_POINT('Ctrl Pts',(3.54505116448901,-6.05190407164105,11.4422073716927));
#76852=CARTESIAN_POINT('Ctrl Pts',(3.7045750104399,-5.95262551774629,11.4507382990519));
#76853=CARTESIAN_POINT('Ctrl Pts',(3.86406857099377,-5.85336581175731,11.4592676068256));
#76854=CARTESIAN_POINT('Ctrl Pts',(4.0195889662208,-5.74768077442588,11.4677969145993));
#76855=CARTESIAN_POINT('Ctrl Pts',(4.17062334758744,-5.63591407449213,11.476326222373));
#76856=CARTESIAN_POINT('Ctrl Pts',(4.3294213769491,-5.51840221039114,11.4852939637179));
#76857=CARTESIAN_POINT('Ctrl Pts',(4.48325975390525,-5.39416718527567,11.4942617050628));
#76858=CARTESIAN_POINT('Ctrl Pts',(4.63157901569038,-5.26365865001869,11.5032294464077));
#76859=CARTESIAN_POINT('Ctrl Pts',(4.77264237821296,-5.13953469875525,11.5117584785314));
#76860=CARTESIAN_POINT('Ctrl Pts',(4.90871346980811,-5.00973659621219,11.5202875106552));
#76861=CARTESIAN_POINT('Ctrl Pts',(5.03934623655124,-4.87469138209352,11.528816542779));
#76862=CARTESIAN_POINT('Ctrl Pts',(5.16998030996718,-4.73964481716591,11.5373456602157));
#76863=CARTESIAN_POINT('Ctrl Pts',(5.29517573927452,-4.5993512581201,11.5458747776523));
#76864=CARTESIAN_POINT('Ctrl Pts',(5.41452418602606,-4.45427372322794,11.554403895089));
#76865=CARTESIAN_POINT('Ctrl Pts',(5.53389678148686,-4.30916683365789,11.562934738289));
#76866=CARTESIAN_POINT('Ctrl Pts',(5.6474198376326,-4.15927427195977,11.571465581489));
#76867=CARTESIAN_POINT('Ctrl Pts',(5.75472552247272,-4.00509184957113,11.579996424689));
#76868=CARTESIAN_POINT('Ctrl Pts',(5.77125665352394,-3.9813390555407,11.5813106559632));
#76869=CARTESIAN_POINT('Ctrl Pts',(5.78764030715153,-3.95748450720761,11.5826248872374));
#76870=CARTESIAN_POINT('Ctrl Pts',(5.80387522874341,-3.93353008017972,11.5839391185116));
#76871=CARTESIAN_POINT('Ctrl Pts',(5.90925921975167,-3.77803729826333,11.5924700458709));
#76872=CARTESIAN_POINT('Ctrl Pts',(6.00840889593352,-3.61828041899149,11.6010009732301));
#76873=CARTESIAN_POINT('Ctrl Pts',(6.10099322995065,-3.45478048081153,11.6095319005894));
#76874=CARTESIAN_POINT('Ctrl Pts',(6.19355998695104,-3.29131158288457,11.618061208363));
#76875=CARTESIAN_POINT('Ctrl Pts',(6.27956373833922,-3.12410131048978,11.6265905161367));
#76876=CARTESIAN_POINT('Ctrl Pts',(6.35871855945826,-2.95369680977941,11.6351198239104));
#76877=CARTESIAN_POINT('Ctrl Pts',(6.44194219035925,-2.77453297527768,11.6440875652553));
#76878=CARTESIAN_POINT('Ctrl Pts',(6.51759406510952,-2.59183819829493,11.6530553066002));
#76879=CARTESIAN_POINT('Ctrl Pts',(6.58539803079892,-2.40627499227535,11.6620230479451));
#76880=CARTESIAN_POINT('Ctrl Pts',(6.64988497118259,-2.22978968964862,11.6705520800688));
#76881=CARTESIAN_POINT('Ctrl Pts',(6.70727338892337,-2.05071021315633,11.6790811121926));
#76882=CARTESIAN_POINT('Ctrl Pts',(6.75737590055037,-1.86962496270269,11.6876101443164));
#76883=CARTESIAN_POINT('Ctrl Pts',(6.80747891333487,-1.68853790091811,11.696139261753));
#76884=CARTESIAN_POINT('Ctrl Pts',(6.85029579585306,-1.50544532105624,11.7046683791897));
#76885=CARTESIAN_POINT('Ctrl Pts',(6.88568949677476,-1.32094917256713,11.7131974966263));
#76886=CARTESIAN_POINT('Ctrl Pts',(6.92109035918214,-1.13641569352227,11.7217283398263));
#76887=CARTESIAN_POINT('Ctrl Pts',(6.94906498328526,-0.950478379528501,
11.7302591830263));
#76888=CARTESIAN_POINT('Ctrl Pts',(6.96952757673796,-0.76374859711106,11.7387900262263));
#76889=CARTESIAN_POINT('Ctrl Pts',(6.97267997089618,-0.734981672888097,
11.7401042575005));
#76890=CARTESIAN_POINT('Ctrl Pts',(6.97565417904955,-0.706195953020086,
11.7414184887748));
#76891=CARTESIAN_POINT('Ctrl Pts',(6.97844999683549,-0.677393684770329,
11.7427327200491));
#76892=CARTESIAN_POINT('Ctrl Pts',(6.99659818650985,-0.490432635349663,
11.7512636474084));
#76893=CARTESIAN_POINT('Ctrl Pts',(7.0072317929105,-0.302709847237606,11.7597945747676));
#76894=CARTESIAN_POINT('Ctrl Pts',(7.01030941215522,-0.114841231045246,
11.7683255021269));
#76895=CARTESIAN_POINT('Ctrl Pts',(7.01338644711788,0.0729917185319949,
11.7768548099006));
#76896=CARTESIAN_POINT('Ctrl Pts',(7.00891035259778,0.260970134912832,11.7853841176742));
#76897=CARTESIAN_POINT('Ctrl Pts',(6.99689182124385,0.448476760056742,11.7939134254479));
#76898=CARTESIAN_POINT('Ctrl Pts',(6.9842554991193,0.645621822629625,11.8028811667928));
#76899=CARTESIAN_POINT('Ctrl Pts',(6.96328091396697,0.842244950637739,11.8118489081377));
#76900=CARTESIAN_POINT('Ctrl Pts',(6.93404253432215,1.03763225408199,11.8208166494826));
#76901=CARTESIAN_POINT('Ctrl Pts',(6.90623452005778,1.22346105127444,11.8293456816064));
#76902=CARTESIAN_POINT('Ctrl Pts',(6.870951978804,1.40817172144332,11.8378747137301));
#76903=CARTESIAN_POINT('Ctrl Pts',(6.82831187180202,1.5911579255082,11.8464037458539));
#76904=CARTESIAN_POINT('Ctrl Pts',(6.78567133828632,1.77414595991857,11.8549328632905));
#76905=CARTESIAN_POINT('Ctrl Pts',(6.73567316461057,1.95540919628536,11.8634619807272));
#76906=CARTESIAN_POINT('Ctrl Pts',(6.67848499248496,2.13435347767263,11.8719910981638));
#76907=CARTESIAN_POINT('Ctrl Pts',(6.62128524902705,2.31333396626264,11.8805219413638));
#76908=CARTESIAN_POINT('Ctrl Pts',(6.556892695528,2.48999427131952,11.8890527845638));
#76909=CARTESIAN_POINT('Ctrl Pts',(6.48552449095859,2.66375649031145,11.8975836277638));
#76910=CARTESIAN_POINT('Ctrl Pts',(6.47452975992965,2.69052567796768,11.8988978590381));
#76911=CARTESIAN_POINT('Ctrl Pts',(6.46336956671342,2.71722612121925,11.9002120903123));
#76912=CARTESIAN_POINT('Ctrl Pts',(6.4520448070097,2.74385574891231,11.9015263215866));
#76913=CARTESIAN_POINT('Ctrl Pts',(6.37853361892237,2.91671377162142,11.9100572489459));
#76914=CARTESIAN_POINT('Ctrl Pts',(6.29805924023454,3.08664550243246,11.9185881763051));
#76915=CARTESIAN_POINT('Ctrl Pts',(6.21087998261419,3.25309028526145,11.9271191036644));
#76916=CARTESIAN_POINT('Ctrl Pts',(6.12371727586372,3.41950346876258,11.935648411438));
#76917=CARTESIAN_POINT('Ctrl Pts',(6.02985237242374,3.58243075422884,11.9441777192117));
#76918=CARTESIAN_POINT('Ctrl Pts',(5.92958997594226,3.74133522685486,11.9527070269854));
#76919=CARTESIAN_POINT('Ctrl Pts',(5.82417377311273,3.90840789522019,11.9616747683303));
#76920=CARTESIAN_POINT('Ctrl Pts',(5.7116852314054,4.07103297223653,11.9706425096752));
#76921=CARTESIAN_POINT('Ctrl Pts',(5.59253128927933,4.22861920027468,11.9796102510201));
#76922=CARTESIAN_POINT('Ctrl Pts',(5.4792064551898,4.37849618150225,11.9881392831438));
#76923=CARTESIAN_POINT('Ctrl Pts',(5.35985298726444,4.52381527551863,11.9966683152676));
#76924=CARTESIAN_POINT('Ctrl Pts',(5.23486368244281,4.66409999772103,12.0051973473914));
#76925=CARTESIAN_POINT('Ctrl Pts',(5.10987312739806,4.80438612314112,12.013726464828));
#76926=CARTESIAN_POINT('Ctrl Pts',(4.97924682892356,4.9396375496616,12.0222555822646));
#76927=CARTESIAN_POINT('Ctrl Pts',(4.84341625951693,5.06941273714688,12.0307846997013));
#76928=CARTESIAN_POINT('Ctrl Pts',(4.70755820644357,5.19921418306587,12.0393155429012));
#76929=CARTESIAN_POINT('Ctrl Pts',(4.56649400128168,5.32353696597768,12.0478463861012));
#76930=CARTESIAN_POINT('Ctrl Pts',(4.42069082235599,5.44197750965929,12.0563772293012));
#76931=CARTESIAN_POINT('Ctrl Pts',(4.39822890468348,5.46022403734727,12.0576914605755));
#76932=CARTESIAN_POINT('Ctrl Pts',(4.37565457964087,5.47833103685979,12.0590056918498));
#76933=CARTESIAN_POINT('Ctrl Pts',(4.35296962466576,5.49629711799109,12.0603199231241));
#76934=CARTESIAN_POINT('Ctrl Pts',(4.20571722942396,5.61291839771571,12.0688508504834));
#76935=CARTESIAN_POINT('Ctrl Pts',(4.0537502967726,5.72363863137833,12.0773817778426));
#76936=CARTESIAN_POINT('Ctrl Pts',(3.89756389109848,5.82808907595837,12.0859127052019));
#76937=CARTESIAN_POINT('Ctrl Pts',(3.74140713721253,5.93251969075589,12.0944420129756));
#76938=CARTESIAN_POINT('Ctrl Pts',(3.5810327633266,6.03068272171986,12.1029713207493));
#76939=CARTESIAN_POINT('Ctrl Pts',(3.41696521332584,6.1222524689383,12.111500628523));
#76940=CARTESIAN_POINT('Ctrl Pts',(3.24446406897338,6.21852919266078,12.1204683698679));
#76941=CARTESIAN_POINT('Ctrl Pts',(3.06788037503395,6.30751675766089,12.1294361112128));
#76942=CARTESIAN_POINT('Ctrl Pts',(2.88785434964569,6.38889065626674,12.1384038525576));
#76943=CARTESIAN_POINT('Ctrl Pts',(2.71663534425694,6.46628367738049,12.1469328846814));
#76944=CARTESIAN_POINT('Ctrl Pts',(2.54230306279958,6.53679002485036,12.1554619168052));
#76945=CARTESIAN_POINT('Ctrl Pts',(2.36543039462724,6.60017921049676,12.163990948929));
#76946=CARTESIAN_POINT('Ctrl Pts',(2.18855595726061,6.6635690302026,12.1725200663657));
#76947=CARTESIAN_POINT('Ctrl Pts',(2.00914137174163,6.71984144557955,12.1810491838023));
#76948=CARTESIAN_POINT('Ctrl Pts',(1.8277767709993,6.76881515761033,12.189578301239));
#76949=CARTESIAN_POINT('Ctrl Pts',(1.64637547333213,6.81779877887711,12.198109144439));
#76950=CARTESIAN_POINT('Ctrl Pts',(1.46302366824735,6.85948066824455,12.206639987639));
#76951=CARTESIAN_POINT('Ctrl Pts',(1.27832467986038,6.89372994650645,12.215170830839));
#76952=CARTESIAN_POINT('Ctrl Pts',(1.24987061252392,6.89900626814958,12.2164850621132));
#76953=CARTESIAN_POINT('Ctrl Pts',(1.22138459165351,6.90410628749476,12.2177992933874));
#76954=CARTESIAN_POINT('Ctrl Pts',(1.1928688431785,6.90902963414357,12.2191135246616));
#76955=CARTESIAN_POINT('Ctrl Pts',(1.00776764857753,6.94098802187192,12.2276444520209));
#76956=CARTESIAN_POINT('Ctrl Pts',(0.821349726612002,6.96550897478315,12.2361753793801));
#76957=CARTESIAN_POINT('Ctrl Pts',(0.634226223665535,6.98250554312096,12.2447063067394));
#76958=CARTESIAN_POINT('Ctrl Pts',(0.44713824587523,6.99949888468215,12.2532356145131));
#76959=CARTESIAN_POINT('Ctrl Pts',(0.259345259236782,7.0089706646968,12.2617649222868));
#76960=CARTESIAN_POINT('Ctrl Pts',(0.071463615970264,7.01088578669575,12.2702942300605));
#76961=CARTESIAN_POINT('Ctrl Pts',(-0.126075741850434,7.01289935206193,
12.2792619714054));
#76962=CARTESIAN_POINT('Ctrl Pts',(-0.323712748584714,7.00655890577502,
12.2882297127503));
#76963=CARTESIAN_POINT('Ctrl Pts',(-0.520729958005908,6.99188578806428,
12.2971974540951));
#76964=CARTESIAN_POINT('Ctrl Pts',(-0.70810892484529,6.97793049124006,12.3057264862189));
#76965=CARTESIAN_POINT('Ctrl Pts',(-0.894926956630577,6.95643834403778,
12.3142555183427));
#76966=CARTESIAN_POINT('Ctrl Pts',(-1.08057071195963,6.9274810356258,12.3227845504665));
#76967=CARTESIAN_POINT('Ctrl Pts',(-1.26621632421679,6.89852343756421,12.3313136679031));
#76968=CARTESIAN_POINT('Ctrl Pts',(-1.45068733450797,6.86210057947786,12.3398427853397));
#76969=CARTESIAN_POINT('Ctrl Pts',(-1.63337879291733,6.81833559465563,12.3483719027764));
#76970=CARTESIAN_POINT('Ctrl Pts',(-1.81610721672529,6.77456175452006,12.3569027459764));
#76971=CARTESIAN_POINT('Ctrl Pts',(-1.99705507191243,6.7234428927166,12.3654335891764));
#76972=CARTESIAN_POINT('Ctrl Pts',(-2.17562994733623,6.66515272853922,12.3739644323764));
#76973=CARTESIAN_POINT('Ctrl Pts',(-2.20314055567612,6.65617275376423,12.3752786636506));
#76974=CARTESIAN_POINT('Ctrl Pts',(-2.2305948751188,6.64702267581864,12.3765928949249));
#76975=CARTESIAN_POINT('Ctrl Pts',(-2.25799077380797,6.63770323439502,12.3779071261992));
#76976=CARTESIAN_POINT('Ctrl Pts',(-2.43582280857313,6.57720895201938,12.3864380535585));
#76977=CARTESIAN_POINT('Ctrl Pts',(-2.61125281161355,6.50955370244616,12.3949689809177));
#76978=CARTESIAN_POINT('Ctrl Pts',(-2.783702519971,6.4349535229718,12.403499908277));
#76979=CARTESIAN_POINT('Ctrl Pts',(-2.95611948897335,6.36036750624545,12.4120292160506));
#76980=CARTESIAN_POINT('Ctrl Pts',(-3.12555701150585,6.27883931231684,12.4205585238243));
#76981=CARTESIAN_POINT('Ctrl Pts',(-3.29145706134546,6.19063300283736,12.429087831598));
#76982=CARTESIAN_POINT('Ctrl Pts',(-3.46588490186243,6.09789260826032,12.4380555729429));
#76983=CARTESIAN_POINT('Ctrl Pts',(-3.63640168893796,5.99776961881503,12.4470233142878));
#76984=CARTESIAN_POINT('Ctrl Pts',(-3.80238762400336,5.89062602100372,12.4559910556327));
#76985=CARTESIAN_POINT('Ctrl Pts',(-3.96025339173896,5.78872397538899,12.4645200877564));
#76986=CARTESIAN_POINT('Ctrl Pts',(-4.11402073983235,5.68047199133421,12.4730491198802));
#76987=CARTESIAN_POINT('Ctrl Pts',(-4.26318537528538,5.5662264612979,12.481578152004));
#76988=CARTESIAN_POINT('Ctrl Pts',(-4.41235150277912,5.45197978850424,12.4901072694406));
#76989=CARTESIAN_POINT('Ctrl Pts',(-4.55691458451787,5.33173963869023,12.4986363868772));
#76990=CARTESIAN_POINT('Ctrl Pts',(-4.69640230864733,5.20590356401576,12.5071655043139));
#76991=CARTESIAN_POINT('Ctrl Pts',(-4.83591825642416,5.08004202793945,12.5156963475138));
#76992=CARTESIAN_POINT('Ctrl Pts',(-4.97035656874706,4.94858251132437,12.5242271907138));
#76993=CARTESIAN_POINT('Ctrl Pts',(-5.09928014619986,4.81196098831567,12.5327580339138));
#76994=CARTESIAN_POINT('Ctrl Pts',(-5.11914165267813,4.79091356380326,12.5340722651881));
#76995=CARTESIAN_POINT('Ctrl Pts',(-5.13887234810774,4.76974369747548,12.5353864964624));
#76996=CARTESIAN_POINT('Ctrl Pts',(-5.15847071434015,4.74845305881768,12.5367007277367));
#76997=CARTESIAN_POINT('Ctrl Pts',(-5.28568623754314,4.6102527770157,12.5452315724605));
#76998=CARTESIAN_POINT('Ctrl Pts',(-5.40736656653399,4.46691356332463,12.5537624171842));
#76999=CARTESIAN_POINT('Ctrl Pts',(-5.52310728351011,4.31890176981807,12.562293261908));
#77000=CARTESIAN_POINT('Ctrl Pts',(-5.63883447817802,4.17090726893886,12.5708231099496));
#77001=CARTESIAN_POINT('Ctrl Pts',(-5.74862325482246,4.01824151702849,12.5793529579912));
#77002=CARTESIAN_POINT('Ctrl Pts',(-5.85210986254844,3.86140346495459,12.5878828060328));
#77003=CARTESIAN_POINT('Ctrl Pts',(-5.95558215690717,3.70458710535557,12.5964114743));
#77004=CARTESIAN_POINT('Ctrl Pts',(-6.0527538545703,3.54359985365895,12.6049401425672));
#77005=CARTESIAN_POINT('Ctrl Pts',(-6.14330460870189,3.37896952445596,12.6134688108344));
#77006=CARTESIAN_POINT('Ctrl Pts',(-6.23386368139959,3.21432407126764,12.6219982625991));
#77007=CARTESIAN_POINT('Ctrl Pts',(-6.31780044538522,3.04603513900085,12.6305277143639));
#77008=CARTESIAN_POINT('Ctrl Pts',(-6.3948401306816,2.87465585166714,12.6390571661286));
#77009=CARTESIAN_POINT('Ctrl Pts',(-6.45877643285204,2.732425806742,12.6461358763191));
#77010=CARTESIAN_POINT('Ctrl Pts',(-6.51796310877441,2.5880677856993,12.6532145865095));
#77011=CARTESIAN_POINT('Ctrl Pts',(-6.57226799596304,2.44190907933526,12.6602932967));
#77012=CARTESIAN_POINT('Origin',(0.,0.,10.));
#77013=CARTESIAN_POINT('',(-6.57184683924635,2.44175302781609,14.6603043765569));
#77014=CARTESIAN_POINT('',(-6.57226804984416,2.4419089343171,14.1134456015891));
#77015=CARTESIAN_POINT('',(-6.57226799596304,2.44190907933527,10.));
#77016=CARTESIAN_POINT('Ctrl Pts',(-6.57226804984416,2.44190893431709,14.1134456015891));
#77017=CARTESIAN_POINT('Ctrl Pts',(-6.48988173044915,2.66364733213147,14.1025828518473));
#77018=CARTESIAN_POINT('Ctrl Pts',(-6.39630361412272,2.88113588408464,14.0916770028235));
#77019=CARTESIAN_POINT('Ctrl Pts',(-6.20477826197012,3.270675629613,14.0717600846099));
#77020=CARTESIAN_POINT('Ctrl Pts',(-6.11023863081956,3.44406416570828,14.0627446265518));
#77021=CARTESIAN_POINT('Ctrl Pts',(-5.80031227068627,3.9594459635228,14.035439112705));
#77022=CARTESIAN_POINT('Ctrl Pts',(-5.56258254002533,4.2870170627201,14.0174075629248));
#77023=CARTESIAN_POINT('Ctrl Pts',(-5.17403817579258,4.73526728233403,13.9908142506871));
#77024=CARTESIAN_POINT('Ctrl Pts',(-5.04437180995973,4.87316514332628,13.9823164042756));
#77025=CARTESIAN_POINT('Ctrl Pts',(-4.72658268366533,5.18483684998203,13.9620929363086));
#77026=CARTESIAN_POINT('Ctrl Pts',(-4.53420453237304,5.35388677028809,13.9503106104565));
#77027=CARTESIAN_POINT('Ctrl Pts',(-4.09882958945337,5.69613542265287,13.924829527098));
#77028=CARTESIAN_POINT('Ctrl Pts',(-3.85314222011895,5.86512258394285,13.9111641428651));
#77029=CARTESIAN_POINT('Ctrl Pts',(-3.38651301337097,6.14406628020359,13.8864515842056));
#77030=CARTESIAN_POINT('Ctrl Pts',(-3.16909023227608,6.25898481690349,13.8753782590726));
#77031=CARTESIAN_POINT('Ctrl Pts',(-2.73841179111228,6.45841318393376,13.8540790468738));
#77032=CARTESIAN_POINT('Ctrl Pts',(-2.52616017117184,6.54434979977739,13.843858869066));
#77033=CARTESIAN_POINT('Ctrl Pts',(-2.16646658765174,6.66987166256495,13.8267472874566));
#77034=CARTESIAN_POINT('Ctrl Pts',(-2.02125552842448,6.71530274275546,13.8198910068932));
#77035=CARTESIAN_POINT('Ctrl Pts',(-1.63487962710397,6.822516228019,13.8016439752891));
#77036=CARTESIAN_POINT('Ctrl Pts',(-1.3917075404866,6.87624221271912,13.7901835469605));
#77037=CARTESIAN_POINT('Ctrl Pts',(-0.840175372970261,6.96763611611037,
13.7644616339783));
#77038=CARTESIAN_POINT('Ctrl Pts',(-0.531120257163189,6.99798292517838,
13.7502416090816));
#77039=CARTESIAN_POINT('Ctrl Pts',(0.181645536548465,7.02046808966678,13.7178637521637));
#77040=CARTESIAN_POINT('Ctrl Pts',(0.584707402117657,6.99843479598702,13.6998792989317));
#77041=CARTESIAN_POINT('Ctrl Pts',(1.17163332084612,6.91526944372014,13.6733053088329));
#77042=CARTESIAN_POINT('Ctrl Pts',(1.35846081373189,6.88100708483956,13.6647784087037));
#77043=CARTESIAN_POINT('Ctrl Pts',(1.79384769552674,6.78273672186202,13.6444997429995));
#77044=CARTESIAN_POINT('Ctrl Pts',(2.04074158588925,6.71258355814904,13.6326911383502));
#77045=CARTESIAN_POINT('Ctrl Pts',(2.56460529817627,6.53215039256923,13.6071974954196));
#77046=CARTESIAN_POINT('Ctrl Pts',(2.83952635221048,6.41742037794411,13.5935457310602));
#77047=CARTESIAN_POINT('Ctrl Pts',(3.32676001282588,6.17662955546867,13.5688407075346));
#77048=CARTESIAN_POINT('Ctrl Pts',(3.5413121731163,6.05617007167114,13.5577616718927));
#77049=CARTESIAN_POINT('Ctrl Pts',(3.94207716266246,5.80256919672595,13.5364782323738));
#77050=CARTESIAN_POINT('Ctrl Pts',(4.12897741638742,5.67109571939389,13.5262792566597));
#77051=CARTESIAN_POINT('Ctrl Pts',(4.42922490054694,5.43716583396649,13.5091833949684));
#77052=CARTESIAN_POINT('Ctrl Pts',(4.54624057387714,5.33970987365993,13.5023213004557));
#77053=CARTESIAN_POINT('Ctrl Pts',(4.84620827224397,5.07286991086351,13.4840515739854));
#77054=CARTESIAN_POINT('Ctrl Pts',(5.02345829493919,4.89740832209359,13.4725739360711));
#77055=CARTESIAN_POINT('Ctrl Pts',(5.39795781404628,4.48491737642743,13.4469403718156));
#77056=CARTESIAN_POINT('Ctrl Pts',(5.58968999466384,4.24356030890051,13.4328247814249));
#77057=CARTESIAN_POINT('Ctrl Pts',(5.99858913327381,3.65282013906985,13.4002009206419));
#77058=CARTESIAN_POINT('Ctrl Pts',(6.20214284058919,3.29539007315769,13.3818826938069));
#77059=CARTESIAN_POINT('Ctrl Pts',(6.45048723142797,2.75375762287443,13.3551672738472));
#77060=CARTESIAN_POINT('Ctrl Pts',(6.5210129851148,2.58231573513183,13.3468420622052));
#77061=CARTESIAN_POINT('Ctrl Pts',(6.67134828613846,2.17127315620059,13.326954777041));
#77062=CARTESIAN_POINT('Ctrl Pts',(6.74517234014827,1.92975711192974,13.3153370480986));
#77063=CARTESIAN_POINT('Ctrl Pts',(6.8756245571424,1.40278755445331,13.2903578840909));
#77064=CARTESIAN_POINT('Ctrl Pts',(6.92784099962088,1.11671380222594,13.2770266146276));
#77065=CARTESIAN_POINT('Ctrl Pts',(6.99018049632219,0.592679883307333,13.2530232141164));
#77066=CARTESIAN_POINT('Ctrl Pts',(7.00622988329145,0.355862965151497,13.2423242106312));
#77067=CARTESIAN_POINT('Ctrl Pts',(7.01457524698399,-0.137060179496263,
13.2201855464205));
#77068=CARTESIAN_POINT('Ctrl Pts',(7.00490678516095,-0.392850657460589,
13.2087707119927));
#77069=CARTESIAN_POINT('Ctrl Pts',(6.97473271599155,-0.718165076226803,
13.1940898122617));
#77070=CARTESIAN_POINT('Ctrl Pts',(6.9671105582604,-0.788687455659186,13.1908968216263));
#77071=CARTESIAN_POINT('Ctrl Pts',(6.94282124280033,-0.985426909372901,
13.1819446345389));
#77072=CARTESIAN_POINT('Ctrl Pts',(6.92378495850714,-1.11132076662028,13.1761573600352));
#77073=CARTESIAN_POINT('Ctrl Pts',(6.85264042021602,-1.50836258796409,13.1577099118988));
#77074=CARTESIAN_POINT('Ctrl Pts',(6.78794220051204,-1.77698582695205,13.1449735971886));
#77075=CARTESIAN_POINT('Ctrl Pts',(6.63373968894409,-2.28373638118698,13.120643079893));
#77076=CARTESIAN_POINT('Ctrl Pts',(6.54679125341049,-2.52219786746139,13.1090568645139));
#77077=CARTESIAN_POINT('Ctrl Pts',(6.33139713751134,-3.02617441237579,13.0842104105928));
#77078=CARTESIAN_POINT('Ctrl Pts',(6.19874104588227,-3.2893668581869,13.07100892477));
#77079=CARTESIAN_POINT('Ctrl Pts',(5.92623914614782,-3.75462576597372,13.0468571513832));
#77080=CARTESIAN_POINT('Ctrl Pts',(5.7915769575567,-3.95918656590113,13.0359157636759));
#77081=CARTESIAN_POINT('Ctrl Pts',(5.56187415965321,-4.27124809640272,13.0183664630607));
#77082=CARTESIAN_POINT('Ctrl Pts',(5.47376146129888,-4.3835987796216,13.0118464496891));
#77083=CARTESIAN_POINT('Ctrl Pts',(5.1957290971398,-4.71664776684635,12.9919466769759));
#77084=CARTESIAN_POINT('Ctrl Pts',(4.99543886527827,-4.92828153788388,12.9785181364631));
#77085=CARTESIAN_POINT('Ctrl Pts',(4.70567971801063,-5.19858278208314,12.9603589361663));
#77086=CARTESIAN_POINT('Ctrl Pts',(4.62718110597341,-5.26857474276685,12.955552163469));
#77087=CARTESIAN_POINT('Ctrl Pts',(4.37862847841751,-5.48035114091313,12.9406705061009));
#77088=CARTESIAN_POINT('Ctrl Pts',(4.20341205452278,-5.6158673035093,12.9306568739139));
#77089=CARTESIAN_POINT('Ctrl Pts',(3.78284448264097,-5.91041608574044,12.9075512508823));
#77090=CARTESIAN_POINT('Ctrl Pts',(3.53337802338744,-6.0628516570412,12.8945251024392));
#77091=CARTESIAN_POINT('Ctrl Pts',(3.13823435722511,-6.27160936871312,12.8744563144973));
#77092=CARTESIAN_POINT('Ctrl Pts',(2.99897940001549,-6.33937858309311,12.8674800403988));
#77093=CARTESIAN_POINT('Ctrl Pts',(2.62347826779143,-6.50697452681015,12.8487708491087));
#77094=CARTESIAN_POINT('Ctrl Pts',(2.38380876437409,-6.59854598723767,12.8369615147659));
#77095=CARTESIAN_POINT('Ctrl Pts',(1.85424117501637,-6.76825311556731,12.811377009426));
#77096=CARTESIAN_POINT('Ctrl Pts',(1.56324006235294,-6.84132637222216,12.7976383887479));
#77097=CARTESIAN_POINT('Ctrl Pts',(0.855568587195019,-6.97150426794817,
12.7649596695206));
#77098=CARTESIAN_POINT('Ctrl Pts',(0.436695241808399,-7.01021907867285,
12.7462354263558));
#77099=CARTESIAN_POINT('Ctrl Pts',(-0.163179941827193,-7.01166313000463,
12.7193342721605));
#77100=CARTESIAN_POINT('Ctrl Pts',(-0.343185637050606,-7.00516021896718,
12.7112415635933));
#77101=CARTESIAN_POINT('Ctrl Pts',(-0.769108155320197,-6.97331602692858,
12.6918310613502));
#77102=CARTESIAN_POINT('Ctrl Pts',(-1.01432928660154,-6.94188715756695,
12.6804597123928));
#77103=CARTESIAN_POINT('Ctrl Pts',(-1.47788151274357,-6.85738516255359,
12.6587786344256));
#77104=CARTESIAN_POINT('Ctrl Pts',(-1.69633470984525,-6.8066375957765,12.6484799003081));
#77105=CARTESIAN_POINT('Ctrl Pts',(-2.00825421886854,-6.71822553786148,
12.6336734228701));
#77106=CARTESIAN_POINT('Ctrl Pts',(-2.10393107729957,-6.68887985024936,
12.6291167729688));
#77107=CARTESIAN_POINT('Ctrl Pts',(-2.58074358319704,-6.53139035754671,
12.60631797778));
#77108=CARTESIAN_POINT('Ctrl Pts',(-2.95098538578073,-6.37267508528968,
12.5883699807238));
#77109=CARTESIAN_POINT('Ctrl Pts',(-3.47347277529501,-6.09334533611682,
12.5618108019302));
#77110=CARTESIAN_POINT('Ctrl Pts',(-3.63763677496041,-5.99678808579302,
12.5532612756259));
#77111=CARTESIAN_POINT('Ctrl Pts',(-4.0136257607369,-5.75451461614941,12.5329398890637));
#77112=CARTESIAN_POINT('Ctrl Pts',(-4.22177221571216,-5.60359409819699,
12.5211110930139));
#77113=CARTESIAN_POINT('Ctrl Pts',(-4.65195936006898,-5.25407745300491,
12.4956078013151));
#77114=CARTESIAN_POINT('Ctrl Pts',(-4.87059536823905,-5.05206508726229,
12.4819665011341));
#77115=CARTESIAN_POINT('Ctrl Pts',(-5.40298159409744,-4.49337581611234,
12.4468864383951));
#77116=CARTESIAN_POINT('Ctrl Pts',(-5.69452329112035,-4.11765027914722,
12.4257872801048));
#77117=CARTESIAN_POINT('Ctrl Pts',(-6.0266051379498,-3.58620364131152,12.3976400975817));
#77118=CARTESIAN_POINT('Ctrl Pts',(-6.10308650553591,-3.45444069495734,
12.3907750264937));
#77119=CARTESIAN_POINT('Ctrl Pts',(-6.29333432179012,-3.10060983671043,
12.3724936953937));
#77120=CARTESIAN_POINT('Ctrl Pts',(-6.39964465845916,-2.87478420958052,
12.3610072612852));
#77121=CARTESIAN_POINT('Ctrl Pts',(-6.60945928994317,-2.35943369831851,
12.3354063821366));
#77122=CARTESIAN_POINT('Ctrl Pts',(-6.7064248963462,-2.06778877808697,12.3213318384269));
#77123=CARTESIAN_POINT('Ctrl Pts',(-6.88833652734206,-1.37085309518822,
12.2886232045153));
#77124=CARTESIAN_POINT('Ctrl Pts',(-6.95715104834616,-0.962534456948641,
12.2701853129887));
#77125=CARTESIAN_POINT('Ctrl Pts',(-7.00402891719657,-0.367372067515399,
12.2434166832279));
#77126=CARTESIAN_POINT('Ctrl Pts',(-7.01125028116588,-0.183715007268657,
12.2351614322727));
#77127=CARTESIAN_POINT('Ctrl Pts',(-7.01124991933926,0.0527219778476604,
12.224417531267));
#77128=CARTESIAN_POINT('Ctrl Pts',(-7.01065540621941,0.105431274551816,
12.2220151425037));
#77129=CARTESIAN_POINT('Ctrl Pts',(-7.00253636237598,0.465329391008556,
12.2055710359533));
#77130=CARTESIAN_POINT('Ctrl Pts',(-6.97541837636501,0.771741537925146,
12.19138509787));
#77131=CARTESIAN_POINT('Ctrl Pts',(-6.89070485524561,1.31751841335441,12.1660295661737));
#77132=CARTESIAN_POINT('Ctrl Pts',(-6.8404535809429,1.55751929512058,12.1548446687587));
#77133=CARTESIAN_POINT('Ctrl Pts',(-6.71974142120346,2.01346896744278,12.1334725173748));
#77134=CARTESIAN_POINT('Ctrl Pts',(-6.65116662782657,2.22955761477444,12.1232869808214));
#77135=CARTESIAN_POINT('Ctrl Pts',(-6.57226802086842,2.44190901230376,12.1131304899038));
#77136=CARTESIAN_POINT('',(-7.01089646739046,9.29430367064582E-6,12.7735343569104));
#77137=CARTESIAN_POINT('Ctrl Pts',(-6.57226799596304,2.44190907933526,12.6602932967));
#77138=CARTESIAN_POINT('Ctrl Pts',(-6.63771323763456,2.26576670328787,12.668824166077));
#77139=CARTESIAN_POINT('Ctrl Pts',(-6.69606694557729,2.08700883280449,12.6773550354539));
#77140=CARTESIAN_POINT('Ctrl Pts',(-6.74714280676067,1.90622414937955,12.6858859048309));
#77141=CARTESIAN_POINT('Ctrl Pts',(-6.76631859965158,1.83835080242298,12.6890887129787));
#77142=CARTESIAN_POINT('Ctrl Pts',(-6.78446905917518,1.77019192375625,12.6922915211265));
#77143=CARTESIAN_POINT('Ctrl Pts',(-6.80158615379011,1.70177917341546,12.6954943292742));
#77144=CARTESIAN_POINT('Ctrl Pts',(-6.84778947410182,1.51711604637734,12.7041395096671));
#77145=CARTESIAN_POINT('Ctrl Pts',(-6.88647402267709,1.33054685313653,12.71278469006));
#77146=CARTESIAN_POINT('Ctrl Pts',(-6.91750562972503,1.14269087036808,12.7214298704529));
#77147=CARTESIAN_POINT('Ctrl Pts',(-6.9486768695701,0.953989592791284,12.7301139515291));
#77148=CARTESIAN_POINT('Ctrl Pts',(-6.97212604646289,0.763990200189306,
12.7387980326054));
#77149=CARTESIAN_POINT('Ctrl Pts',(-6.98776927354008,0.573329872123468,
12.7474821136816));
#77150=CARTESIAN_POINT('Ctrl Pts',(-7.00341250061727,0.382669544057622,
12.7561661947579));
#77151=CARTESIAN_POINT('Ctrl Pts',(-7.0112497463365,0.191348574450929,12.7648502758341));
#77152=CARTESIAN_POINT('Ctrl Pts',(-7.01124999999384,9.29477234728852E-6,
12.7735343569104));
#77153=CARTESIAN_POINT('Ctrl Pts',(-7.01065084487527,9.29397804994014E-6,
12.7735343569104));
#77154=CARTESIAN_POINT('Ctrl Pts',(-7.01062348710872,-0.593030242553413,
12.8004522148775));
#77155=CARTESIAN_POINT('Ctrl Pts',(-6.78980718077563,-2.35224106726475,
12.8803012733571));
#77156=CARTESIAN_POINT('Ctrl Pts',(-5.33497512123331,-4.99561196811091,
13.0130815323492));
#77157=CARTESIAN_POINT('Ctrl Pts',(-2.29473593201848,-6.93918478514677,
13.1718751338868));
#77158=CARTESIAN_POINT('Ctrl Pts',(1.30483947524629,-7.19134844267406,13.3306687354243));
#77159=CARTESIAN_POINT('Ctrl Pts',(4.58636348188468,-5.69063867172615,13.4894623369618));
#77160=CARTESIAN_POINT('Ctrl Pts',(6.74997271289944,-2.80284977393084,13.6482559384993));
#77161=CARTESIAN_POINT('Ctrl Pts',(7.26829275987721,0.768126836418118,13.8070495400368));
#77162=CARTESIAN_POINT('Ctrl Pts',(6.0149843910269,4.15187442678777,13.9658431415743));
#77163=CARTESIAN_POINT('Ctrl Pts',(3.29553842701307,6.52361287602135,14.124636743112));
#77164=CARTESIAN_POINT('Ctrl Pts',(-0.227186892364047,7.30523679260615,
14.2834303446494));
#77165=CARTESIAN_POINT('Ctrl Pts',(-3.69453596762048,6.306227276595,14.4422239461869));
#77166=CARTESIAN_POINT('Ctrl Pts',(-5.72519280635199,4.29984055996828,14.5678486234894));
#77167=CARTESIAN_POINT('Ctrl Pts',(-6.42048420230567,2.84995900409766,14.6405421002794));
#77168=CARTESIAN_POINT('Ctrl Pts',(-6.57184683924635,2.44175302781609,14.6603043765569));
#77169=CARTESIAN_POINT('Origin',(0.,0.,10.));
#77170=CARTESIAN_POINT('',(-6.57226799596304,2.44190907933525,16.660297082902));
#77171=CARTESIAN_POINT('',(-6.57226800013471,2.44190906810743,16.1128890894906));
#77172=CARTESIAN_POINT('',(-6.57226799596304,2.44190907933527,10.));
#77173=CARTESIAN_POINT('',(-7.01124982298433,-0.000107840775152304,14.2261657896268));
#77174=CARTESIAN_POINT('Ctrl Pts',(-6.57226800013471,2.44190906810743,16.1128890894906));
#77175=CARTESIAN_POINT('Ctrl Pts',(-6.47321406132191,2.70850746067215,16.1000058294698));
#77176=CARTESIAN_POINT('Ctrl Pts',(-6.35802203610628,2.96885445807938,16.0872561549564));
#77177=CARTESIAN_POINT('Ctrl Pts',(-6.11278607817882,3.44290730218137,16.063349230731));
#77178=CARTESIAN_POINT('Ctrl Pts',(-5.9865259289693,3.65804157181628,16.0522047637981));
#77179=CARTESIAN_POINT('Ctrl Pts',(-5.76512324278877,3.99301443674072,16.0340052163809));
#77180=CARTESIAN_POINT('Ctrl Pts',(-5.67705232938408,4.11726672994885,16.0270415683926));
#77181=CARTESIAN_POINT('Ctrl Pts',(-5.44697938517922,4.42042679168906,16.0095706924358));
#77182=CARTESIAN_POINT('Ctrl Pts',(-5.30014880499447,4.5954521419498,15.9990469678999));
#77183=CARTESIAN_POINT('Ctrl Pts',(-4.9779943555893,4.94344655030019,15.9772751995181));
#77184=CARTESIAN_POINT('Ctrl Pts',(-4.80156860392471,5.11498132426437,15.9660499864233));
#77185=CARTESIAN_POINT('Ctrl Pts',(-4.39253707364053,5.47282278803232,15.9414226446631));
#77186=CARTESIAN_POINT('Ctrl Pts',(-4.15633294329696,5.65429669936464,15.9280881994101));
#77187=CARTESIAN_POINT('Ctrl Pts',(-3.69635153410875,5.96325623571244,15.9032689427213));
#77188=CARTESIAN_POINT('Ctrl Pts',(-3.47570383842022,6.0944990142313,15.891797475402));
#77189=CARTESIAN_POINT('Ctrl Pts',(-3.08003929870703,6.30135401943445,15.8715281027282));
#77190=CARTESIAN_POINT('Ctrl Pts',(-2.90820878087578,6.38247790616418,15.8628131036066));
#77191=CARTESIAN_POINT('Ctrl Pts',(-2.36238037897974,6.61354847374406,15.8355561554066));
#77192=CARTESIAN_POINT('Ctrl Pts',(-1.97861052089875,6.73832154450749,15.8170388773893));
#77193=CARTESIAN_POINT('Ctrl Pts',(-1.39396728244381,6.87411447245193,15.7898084032682));
#77194=CARTESIAN_POINT('Ctrl Pts',(-1.19988063888418,6.91063546964989,15.7809130319414));
#77195=CARTESIAN_POINT('Ctrl Pts',(-0.742005937103939,6.97691953969843,
15.7601389480075));
#77196=CARTESIAN_POINT('Ctrl Pts',(-0.477558167889971,6.99999401830781,
15.7483059297299));
#77197=CARTESIAN_POINT('Ctrl Pts',(-0.071541594459456,7.01230200129441,
15.7300409646309));
#77198=CARTESIAN_POINT('Ctrl Pts',(0.0694518297413624,7.01232297728411,
15.7236763218157));
#77199=CARTESIAN_POINT('Ctrl Pts',(0.269598471889345,7.00631548122516,15.7145556093177));
#77200=CARTESIAN_POINT('Ctrl Pts',(0.328820463306528,7.00378590394022,15.7118477134487));
#77201=CARTESIAN_POINT('Ctrl Pts',(0.564864238061188,6.99070318140796,15.7010250888106));
#77202=CARTESIAN_POINT('Ctrl Pts',(0.741289758964006,6.97420185498736,15.6928712188857));
#77203=CARTESIAN_POINT('Ctrl Pts',(1.21556669494736,6.91164077589433,15.6708602767436));
#77204=CARTESIAN_POINT('Ctrl Pts',(1.5113885660617,6.85303513894415,15.6570445299789));
#77205=CARTESIAN_POINT('Ctrl Pts',(2.04796722688772,6.71028777253538,15.6318160627858));
#77206=CARTESIAN_POINT('Ctrl Pts',(2.28968221947585,6.63170342031206,15.6203815247903));
#77207=CARTESIAN_POINT('Ctrl Pts',(2.78430226587554,6.4406216954805,15.5965970575234));
#77208=CARTESIAN_POINT('Ctrl Pts',(3.03589054895038,6.32592388874584,15.5842764082701));
#77209=CARTESIAN_POINT('Ctrl Pts',(3.39248247578323,6.13717129633892,15.5660809455926));
#77210=CARTESIAN_POINT('Ctrl Pts',(3.50326970837654,6.07461188121227,15.5603107276888));
#77211=CARTESIAN_POINT('Ctrl Pts',(3.8770596907804,5.84991179339844,15.5403914030376));
#77212=CARTESIAN_POINT('Ctrl Pts',(4.13101616092723,5.67342620114508,15.5261290515184));
#77213=CARTESIAN_POINT('Ctrl Pts',(4.5640574494822,5.3279501468504,15.5006975734885));
#77214=CARTESIAN_POINT('Ctrl Pts',(4.7474702178148,5.16519148501618,15.4895121993205));
#77215=CARTESIAN_POINT('Ctrl Pts',(5.13528968010257,4.78290025263909,15.4648364469547));
#77216=CARTESIAN_POINT('Ctrl Pts',(5.33490156270971,4.55918454745838,15.451416581044));
#77217=CARTESIAN_POINT('Ctrl Pts',(5.67545653054044,4.12440384653347,15.4266795025067));
#77218=CARTESIAN_POINT('Ctrl Pts',(5.82044042599043,3.91713966465796,15.4153751288039));
#77219=CARTESIAN_POINT('Ctrl Pts',(6.0519929210181,3.54478534353158,15.3954709343119));
#77220=CARTESIAN_POINT('Ctrl Pts',(6.14376517877187,3.38323349232264,15.3869516693107));
#77221=CARTESIAN_POINT('Ctrl Pts',(6.41712351483554,2.85413772396954,15.3595685492939));
#77222=CARTESIAN_POINT('Ctrl Pts',(6.57295313255433,2.47424260436356,15.3407246351983));
#77223=CARTESIAN_POINT('Ctrl Pts',(6.72443327156962,1.98736912548396,15.3175940616596));
#77224=CARTESIAN_POINT('Ctrl Pts',(6.75211111071317,1.89119926224203,15.3130693715883));
#77225=CARTESIAN_POINT('Ctrl Pts',(6.80701456618315,1.68382859921106,15.3033945398204));
#77226=CARTESIAN_POINT('Ctrl Pts',(6.83359439481513,1.57248655484323,15.2982495684081));
#77227=CARTESIAN_POINT('Ctrl Pts',(6.91411086075386,1.19445148976342,15.2809054776283));
#77228=CARTESIAN_POINT('Ctrl Pts',(6.9552485774386,0.925288465248311,15.2687713686226));
#77229=CARTESIAN_POINT('Ctrl Pts',(6.99284093723039,0.524293531278006,15.2506312357174));
#77230=CARTESIAN_POINT('Ctrl Pts',(7.00139882810741,0.39385532063017,15.24471480721));
#77231=CARTESIAN_POINT('Ctrl Pts',(7.01113784027787,0.134658067137653,15.2328823042758));
#77232=CARTESIAN_POINT('Ctrl Pts',(7.01242829845094,0.00595524213021864,
15.2269784786135));
#77233=CARTESIAN_POINT('Ctrl Pts',(7.00274564231746,-0.547200268871436,
15.2015473216456));
#77234=CARTESIAN_POINT('Ctrl Pts',(6.9567734181557,-0.970150860339461,15.1820183440202));
#77235=CARTESIAN_POINT('Ctrl Pts',(6.81204441730288,-1.68764841325407,15.1488231010692));
#77236=CARTESIAN_POINT('Ctrl Pts',(6.73151808987719,-1.9846346023707,15.1350453103604));
#77237=CARTESIAN_POINT('Ctrl Pts',(6.54694360840102,-2.52259064812961,15.1095705677517));
#77238=CARTESIAN_POINT('Ctrl Pts',(6.44836945883007,-2.76486185781343,15.0978863546916));
#77239=CARTESIAN_POINT('Ctrl Pts',(6.25261318948531,-3.17818601317203,15.0771209286326));
#77240=CARTESIAN_POINT('Ctrl Pts',(6.16133430604431,-3.35171531608751,15.0681250871579));
#77241=CARTESIAN_POINT('Ctrl Pts',(5.86542071670862,-3.86122966625953,15.0410256747702));
#77242=CARTESIAN_POINT('Ctrl Pts',(5.63967235195088,-4.18406047064741,15.0229525707483));
#77243=CARTESIAN_POINT('Ctrl Pts',(5.18872032020449,-4.72565879527589,14.9909741946301));
#77244=CARTESIAN_POINT('Ctrl Pts',(4.97365607875764,-4.9515067511912,14.9770068633338));
#77245=CARTESIAN_POINT('Ctrl Pts',(4.5600833701806,-5.33159016168186,14.9518470206776));
#77246=CARTESIAN_POINT('Ctrl Pts',(4.36695640702267,-5.49089266049856,14.9406627538777));
#77247=CARTESIAN_POINT('Ctrl Pts',(4.04300218969833,-5.73018685385692,14.9224074571156));
#77248=CARTESIAN_POINT('Ctrl Pts',(3.91734723294093,-5.8168115766629,14.9154288695813));
#77249=CARTESIAN_POINT('Ctrl Pts',(3.39161092388185,-6.15448046359543,14.8867444051407));
#77250=CARTESIAN_POINT('Ctrl Pts',(2.9694697078568,-6.36890287010425,14.8649897459829));
#77251=CARTESIAN_POINT('Ctrl Pts',(2.25495160802314,-6.64523477725838,14.8302705939297));
#77252=CARTESIAN_POINT('Ctrl Pts',(1.97452636909528,-6.73388454633304,14.8171006516703));
#77253=CARTESIAN_POINT('Ctrl Pts',(1.44955634332344,-6.86421632964355,14.7928724134066));
#77254=CARTESIAN_POINT('Ctrl Pts',(1.20677118307273,-6.91103315866354,14.7818245875844));
#77255=CARTESIAN_POINT('Ctrl Pts',(0.811968626806374,-6.9657219929638,14.7637600545402));
#77256=CARTESIAN_POINT('Ctrl Pts',(0.661279679390137,-6.98163901305464,
14.7568323441896));
#77257=CARTESIAN_POINT('Ctrl Pts',(0.280341268960479,-7.00943293982593,
14.7392994496589));
#77258=CARTESIAN_POINT('Ctrl Pts',(0.0497985847253759,-7.0148600681602,
14.7286765207645));
#77259=CARTESIAN_POINT('Ctrl Pts',(-0.425974199871209,-7.00260129428196,
14.7068268352416));
#77260=CARTESIAN_POINT('Ctrl Pts',(-0.67085810083832,-6.98339686005644,
14.6956218542012));
#77261=CARTESIAN_POINT('Ctrl Pts',(-1.21022597131532,-6.91246027691765,
14.6709704752847));
#77262=CARTESIAN_POINT('Ctrl Pts',(-1.5034326253318,-6.85466613445188,14.6575931814329));
#77263=CARTESIAN_POINT('Ctrl Pts',(-2.03824900714496,-6.71327125673849,
14.6328151647518));
#77264=CARTESIAN_POINT('Ctrl Pts',(-2.28070177805989,-6.63482217396105,
14.6214275118978));
#77265=CARTESIAN_POINT('Ctrl Pts',(-2.69359025074597,-6.47591370039997,
14.6013436667967));
#77266=CARTESIAN_POINT('Ctrl Pts',(-2.86605324530143,-6.40145479332655,
14.5927292390086));
#77267=CARTESIAN_POINT('Ctrl Pts',(-3.40162189590929,-6.1442430883952,14.5654092401235));
#77268=CARTESIAN_POINT('Ctrl Pts',(-3.75194879847424,-5.93680448944979,
14.5467259846613));
#77269=CARTESIAN_POINT('Ctrl Pts',(-4.33345536788112,-5.52034398292059,
14.5142777345529));
#77270=CARTESIAN_POINT('Ctrl Pts',(-4.57241919879514,-5.32409803969959,
14.5004294443539));
#77271=CARTESIAN_POINT('Ctrl Pts',(-4.97954552277554,-4.94206056938269,
14.4754216982898));
#77272=CARTESIAN_POINT('Ctrl Pts',(-5.15218694091067,-4.76180664406206,
14.4642708526047));
#77273=CARTESIAN_POINT('Ctrl Pts',(-5.41419227337445,-4.45728033082596,
14.4460623757251));
#77274=CARTESIAN_POINT('Ctrl Pts',(-5.50974036375189,-4.33861558836717,
14.4390963386193));
#77275=CARTESIAN_POINT('Ctrl Pts',(-5.76967118537896,-3.99335009238114,
14.4192569208734));
#77276=CARTESIAN_POINT('Ctrl Pts',(-5.92445947460721,-3.75988456864519,
14.4063519711039));
#77277=CARTESIAN_POINT('Ctrl Pts',(-6.17781879655627,-3.32307854214122,
14.3832172779257));
#77278=CARTESIAN_POINT('Ctrl Pts',(-6.28131766397622,-3.1230349350003,14.3729688694029));
#77279=CARTESIAN_POINT('Ctrl Pts',(-6.45961563677712,-2.73355131727058,
14.3535934252928));
#77280=CARTESIAN_POINT('Ctrl Pts',(-6.53614067663435,-2.54515293123263,
14.3444624188076));
#77281=CARTESIAN_POINT('Ctrl Pts',(-6.71009702690288,-2.05703842655861,
14.321233622511));
#77282=CARTESIAN_POINT('Ctrl Pts',(-6.79571099819986,-1.75360051321066,
14.3071991625631));
#77283=CARTESIAN_POINT('Ctrl Pts',(-6.88269316615911,-1.34074929814142,
14.2880559608511));
#77284=CARTESIAN_POINT('Ctrl Pts',(-6.90235109867921,-1.23556569372825,
14.2831709090337));
#77285=CARTESIAN_POINT('Ctrl Pts',(-6.98059134672087,-0.756448238171518,
14.2609281236194));
#77286=CARTESIAN_POINT('Ctrl Pts',(-7.01124416818815,-0.378589122575148,
14.2434505387525));
#77287=CARTESIAN_POINT('Ctrl Pts',(-7.01124999916793,-0.000108017167545701,
14.2261654923484));
#77288=CARTESIAN_POINT('Ctrl Pts',(-7.01124999917043,-0.000107854693215219,
14.2261654849283));
#77289=CARTESIAN_POINT('Ctrl Pts',(-7.01125249254275,0.161977411666877,
14.2187631303534));
#77290=CARTESIAN_POINT('Ctrl Pts',(-7.00563439082637,0.324015580569475,
14.2113972867494));
#77291=CARTESIAN_POINT('Ctrl Pts',(-6.96413850419295,0.921565848855817,
14.1843028034796));
#77292=CARTESIAN_POINT('Ctrl Pts',(-6.89319891062956,1.35363011315425,14.1649058588365));
#77293=CARTESIAN_POINT('Ctrl Pts',(-6.74939118881894,1.90274460620333,14.1393430625006));
#77294=CARTESIAN_POINT('Ctrl Pts',(-6.7127397031953,2.02826123620837,14.1334263278157));
#77295=CARTESIAN_POINT('Ctrl Pts',(-6.64125641127595,2.2498358571789,14.1228073803761));
#77296=CARTESIAN_POINT('Ctrl Pts',(-6.60780328543634,2.34626773728307,14.11813097137));
#77297=CARTESIAN_POINT('Ctrl Pts',(-6.57226804984416,2.44190893431709,14.1134456015891));
#77298=CARTESIAN_POINT('',(-7.01125169162915,0.000100138860277758,14.7735343587116));
#77299=CARTESIAN_POINT('Ctrl Pts',(-6.57184683924635,2.44175302781609,14.6603043765569));
#77300=CARTESIAN_POINT('Ctrl Pts',(-6.82589327429279,1.75662177524929,14.6934733007919));
#77301=CARTESIAN_POINT('Ctrl Pts',(-6.99426377786268,0.93198229720219,14.7312166275764));
#77302=CARTESIAN_POINT('Ctrl Pts',(-7.01180477314546,0.100836115687778,
14.7689599543609));
#77303=CARTESIAN_POINT('Ctrl Pts',(-7.01173456867506,0.000100185423145271,
14.7735343569104));
#77304=CARTESIAN_POINT('Ctrl Pts',(-7.01124999928488,0.000100138697088386,
14.7735343587179));
#77305=CARTESIAN_POINT('Ctrl Pts',(-7.01125267389351,-0.187163629012723,
14.7820385643826));
#77306=CARTESIAN_POINT('Ctrl Pts',(-7.00374855171984,-0.374461240683102,
14.7905427700473));
#77307=CARTESIAN_POINT('Ctrl Pts',(-6.98875556332075,-0.561179328426533,
14.799046975712));
#77308=CARTESIAN_POINT('Ctrl Pts',(-6.97376533234169,-0.747863076105076,
14.8075496173345));
#77309=CARTESIAN_POINT('Ctrl Pts',(-6.9512890083875,-0.933967203653135,
14.816052258957));
#77310=CARTESIAN_POINT('Ctrl Pts',(-6.92139650471126,-1.11888202553745,
14.8245549005794));
#77311=CARTESIAN_POINT('Ctrl Pts',(-6.8915029616306,-1.30380327717031,14.8330578378507));
#77312=CARTESIAN_POINT('Ctrl Pts',(-6.85419276906023,-1.487534833791,14.841560775122));
#77313=CARTESIAN_POINT('Ctrl Pts',(-6.80958736459116,-1.66947491340852,
14.8500637123933));
#77314=CARTESIAN_POINT('Ctrl Pts',(-6.76498375237899,-1.85140768262575,
14.8585663080143));
#77315=CARTESIAN_POINT('Ctrl Pts',(-6.71308558969616,-2.03154881797963,
14.8670689036353));
#77316=CARTESIAN_POINT('Ctrl Pts',(-6.65406490118876,-2.20930913483556,
14.8755714992563));
#77317=CARTESIAN_POINT('Ctrl Pts',(-6.59502990840115,-2.38711253376063,
14.8840761555702));
#77318=CARTESIAN_POINT('Ctrl Pts',(-6.52886903775336,-2.56253366664827,
14.8925808118841));
#77319=CARTESIAN_POINT('Ctrl Pts',(-6.45580374874602,-2.73499991228095,
14.9010854681979));
#77320=CARTESIAN_POINT('Ctrl Pts',(-6.4056331363489,-2.85342464280321,14.9069252290651));
#77321=CARTESIAN_POINT('Ctrl Pts',(-6.35220815662905,-2.97045651455718,
14.9127649899323));
#77322=CARTESIAN_POINT('Ctrl Pts',(-6.29561354753464,-3.08591584826909,
14.9186047507994));
#77323=CARTESIAN_POINT('Ctrl Pts',(-6.21293815891979,-3.25458288982283,
14.9271356781587));
#77324=CARTESIAN_POINT('Ctrl Pts',(-6.12346653014017,-3.4199544303168,14.935666605518));
#77325=CARTESIAN_POINT('Ctrl Pts',(-6.02748666786554,-3.5814844731205,14.9441975328773));
#77326=CARTESIAN_POINT('Ctrl Pts',(-5.93152502724454,-3.74298384965294,
14.952726840651));
#77327=CARTESIAN_POINT('Ctrl Pts',(-5.82905777520553,-3.90064292077405,
14.9612561484246));
#77328=CARTESIAN_POINT('Ctrl Pts',(-5.72041797044929,-4.05394188486476,
14.9697854561983));
#77329=CARTESIAN_POINT('Ctrl Pts',(-5.60619373389166,-4.21512090371173,
14.9787531975432));
#77330=CARTESIAN_POINT('Ctrl Pts',(-5.48514584979197,-4.37147945782676,
14.9877209388881));
#77331=CARTESIAN_POINT('Ctrl Pts',(-5.35771237882822,-4.52244896358719,
14.996688680233));
#77332=CARTESIAN_POINT('Ctrl Pts',(-5.23651305720476,-4.66603291798798,
15.0052177123568));
#77333=CARTESIAN_POINT('Ctrl Pts',(-5.10953820610418,-4.80474224204222,
15.0137467444806));
#77334=CARTESIAN_POINT('Ctrl Pts',(-4.97720561001781,-4.93812220161746,
15.0222757766044));
#77335=CARTESIAN_POINT('Ctrl Pts',(-4.84487169025588,-5.07150349534466,
15.030804894041));
#77336=CARTESIAN_POINT('Ctrl Pts',(-4.70718013638103,-5.19955510299028,
15.0393340114776));
#77337=CARTESIAN_POINT('Ctrl Pts',(-4.564585478796,-5.32185925868626,15.0478631289143));
#77338=CARTESIAN_POINT('Ctrl Pts',(-4.42196196891348,-5.44418816114307,
15.0563939721143));
#77339=CARTESIAN_POINT('Ctrl Pts',(-4.27443360686351,-5.56076709028424,
15.0649248153143));
#77340=CARTESIAN_POINT('Ctrl Pts',(-4.12248854157675,-5.67121810434658,
15.0734556585142));
#77341=CARTESIAN_POINT('Ctrl Pts',(-4.09908042679984,-5.68823379359926,
15.0747698897885));
#77342=CARTESIAN_POINT('Ctrl Pts',(-4.07556754898652,-5.70510412730578,
15.0760841210628));
#77343=CARTESIAN_POINT('Ctrl Pts',(-4.05195175757022,-5.72182781258084,
15.077398352337));
#77344=CARTESIAN_POINT('Ctrl Pts',(-3.89865712438817,-5.83038446243009,
15.0859292796963));
#77345=CARTESIAN_POINT('Ctrl Pts',(-3.74097119772733,-5.932795727898,15.0944602070555));
#77346=CARTESIAN_POINT('Ctrl Pts',(-3.57940810442678,-6.02871994576493,
15.1029911344148));
#77347=CARTESIAN_POINT('Ctrl Pts',(-3.41787568367117,-6.12462595254278,
15.1115204421885));
#77348=CARTESIAN_POINT('Ctrl Pts',(-3.25246782836961,-6.2140472131687,15.1200497499622));
#77349=CARTESIAN_POINT('Ctrl Pts',(-3.08372569427818,-6.29668662114835,
15.1285790577359));
#77350=CARTESIAN_POINT('Ctrl Pts',(-2.90630967733213,-6.38357395776686,
15.1375467990808));
#77351=CARTESIAN_POINT('Ctrl Pts',(-2.72520788662829,-6.46296368691256,
15.1465145404256));
#77352=CARTESIAN_POINT('Ctrl Pts',(-2.54107702163925,-6.53456610132586,
15.1554822817705));
#77353=CARTESIAN_POINT('Ctrl Pts',(-2.36595398875098,-6.60266566722387,
15.1640113138943));
#77354=CARTESIAN_POINT('Ctrl Pts',(-2.1880914764758,-6.66372151148871,15.1725403460181));
#77355=CARTESIAN_POINT('Ctrl Pts',(-2.00807391033613,-6.71753420036901,
15.1810693781419));
#77356=CARTESIAN_POINT('Ctrl Pts',(-1.82805454354573,-6.77134742751822,
15.1895984955785));
#77357=CARTESIAN_POINT('Ctrl Pts',(-1.64588037411524,-6.81791726992008,
15.1981276130152));
#77358=CARTESIAN_POINT('Ctrl Pts',(-1.46215040842577,-6.85709433693604,
15.2066567304518));
#77359=CARTESIAN_POINT('Ctrl Pts',(-1.27838326720843,-6.89627933095586,
15.2151875736518));
#77360=CARTESIAN_POINT('Ctrl Pts',(-1.09306000066057,-6.92806849899944,
15.2237184168518));
#77361=CARTESIAN_POINT('Ctrl Pts',(-0.906790083467622,-6.95236350509845,
15.2322492600517));
#77362=CARTESIAN_POINT('Ctrl Pts',(-0.878094004441462,-6.95610630707885,
15.233563491326));
#77363=CARTESIAN_POINT('Ctrl Pts',(-0.849375472554494,-6.95967134686518,
15.2348777226002));
#77364=CARTESIAN_POINT('Ctrl Pts',(-0.82063673039657,-6.96305837396356,
15.2361919538745));
#77365=CARTESIAN_POINT('Ctrl Pts',(-0.634088041024037,-6.98504421671893,
15.2447228812337));
#77366=CARTESIAN_POINT('Ctrl Pts',(-0.446623371802602,-6.99953271404237,
15.2532538085928));
#77367=CARTESIAN_POINT('Ctrl Pts',(-0.258857652592978,-7.00646981569136,
15.261784735952));
#77368=CARTESIAN_POINT('Ctrl Pts',(-0.0711275804627589,-7.01340560034055,
15.2703140437257));
#77369=CARTESIAN_POINT('Ctrl Pts',(0.116903121738672,-7.01279283896196,
15.2788433514993));
#77370=CARTESIAN_POINT('Ctrl Pts',(0.304617106579406,-7.00462953916045,
15.2873726592729));
#77371=CARTESIAN_POINT('Ctrl Pts',(0.501980187799274,-6.99604661976255,
15.2963404006178));
#77372=CARTESIAN_POINT('Ctrl Pts',(0.698992770738884,-6.97911647346185,
15.3053081419628));
#77373=CARTESIAN_POINT('Ctrl Pts',(0.894939586006176,-6.95389888479111,
15.3142758833077));
#77374=CARTESIAN_POINT('Ctrl Pts',(1.08130052324435,-6.92991496112717,15.3228049154314));
#77375=CARTESIAN_POINT('Ctrl Pts',(1.26669714844205,-6.89843511430174,15.3313339475551));
#77376=CARTESIAN_POINT('Ctrl Pts',(1.45052084732403,-6.85956382242912,15.3398629796788));
#77377=CARTESIAN_POINT('Ctrl Pts',(1.63434638492899,-6.82069214174081,15.3483920971153));
#77378=CARTESIAN_POINT('Ctrl Pts',(1.81659866587765,-6.77442893478876,15.3569212145519));
#77379=CARTESIAN_POINT('Ctrl Pts',(1.99668021413705,-6.72092959976324,15.3654503319884));
#77380=CARTESIAN_POINT('Ctrl Pts',(2.17679819971142,-6.66741943979679,15.3739811751884));
#77381=CARTESIAN_POINT('Ctrl Pts',(2.35474428207199,-6.60667031551607,15.3825120183883));
#77382=CARTESIAN_POINT('Ctrl Pts',(2.52993621872838,-6.53888746589711,15.3910428615882));
#77383=CARTESIAN_POINT('Ctrl Pts',(2.5569256635951,-6.52844508186041,15.3923570928628));
#77384=CARTESIAN_POINT('Ctrl Pts',(2.58384977831759,-6.51783585807759,15.3936713241374));
#77385=CARTESIAN_POINT('Ctrl Pts',(2.61070647377534,-6.50706064750341,15.394985555412));
#77386=CARTESIAN_POINT('Ctrl Pts',(2.78503843687495,-6.43711668827126,15.4035164827715));
#77387=CARTESIAN_POINT('Ctrl Pts',(2.95658779836659,-6.36015088199504,15.4120474101311));
#77388=CARTESIAN_POINT('Ctrl Pts',(3.12478871300326,-6.27640996602257,15.4205783374906));
#77389=CARTESIAN_POINT('Ctrl Pts',(3.29295769491275,-6.19268494815522,15.4291076452646));
#77390=CARTESIAN_POINT('Ctrl Pts',(3.45777922458081,-6.10218752384163,15.4376369530385));
#77391=CARTESIAN_POINT('Ctrl Pts',(3.61871023981204,-6.00521130042728,15.4461662608125));
#77392=CARTESIAN_POINT('Ctrl Pts',(3.78791362151531,-5.90325019042656,15.4551340021572));
#77393=CARTESIAN_POINT('Ctrl Pts',(3.95281566599083,-5.79412685004287,15.464101743502));
#77394=CARTESIAN_POINT('Ctrl Pts',(4.11281687907556,-5.67823598326903,15.4730694848467));
#77395=CARTESIAN_POINT('Ctrl Pts',(4.26499070231872,-5.5680145922187,15.4815985169708));
#77396=CARTESIAN_POINT('Ctrl Pts',(4.41273147077283,-5.45167218924217,15.4901275490948));
#77397=CARTESIAN_POINT('Ctrl Pts',(4.55555472963676,-5.32959169803693,15.4986565812189));
#77398=CARTESIAN_POINT('Ctrl Pts',(4.69837941710968,-5.20750998570504,15.5071856986557));
#77399=CARTESIAN_POINT('Ctrl Pts',(4.83628626605543,-5.07969027187068,15.5157148160926));
#77400=CARTESIAN_POINT('Ctrl Pts',(4.96882496409711,-4.94655486562773,15.5242439335294));
#77401=CARTESIAN_POINT('Ctrl Pts',(5.10139047973582,-4.81339252105108,15.5327747767297));
#77402=CARTESIAN_POINT('Ctrl Pts',(5.22858545966223,-4.67491255350123,15.5413056199299));
#77403=CARTESIAN_POINT('Ctrl Pts',(5.34999681375057,-4.5315737504049,15.5498364631302));
#77404=CARTESIAN_POINT('Ctrl Pts',(5.36870101387559,-4.509491485703,15.5511506944033));
#77405=CARTESIAN_POINT('Ctrl Pts',(5.38726802491303,-4.48729397047949,15.5524649256764));
#77406=CARTESIAN_POINT('Ctrl Pts',(5.40569642042965,-4.46498295323219,15.5537791569495));
#77407=CARTESIAN_POINT('Ctrl Pts',(5.52531867163153,-4.3201578594079,15.5623100843081));
#77408=CARTESIAN_POINT('Ctrl Pts',(5.63913799204196,-4.17049797480998,15.5708410116668));
#77409=CARTESIAN_POINT('Ctrl Pts',(5.74677554440972,-4.01649068275708,15.5793719390254));
#77410=CARTESIAN_POINT('Ctrl Pts',(5.854392661927,-3.86251262878991,15.5879012467985));
#77411=CARTESIAN_POINT('Ctrl Pts',(5.95583017811103,-3.70418906531051,15.5964305545716));
#77412=CARTESIAN_POINT('Ctrl Pts',(6.05075168607242,-3.54203763333929,15.6049598623446));
#77413=CARTESIAN_POINT('Ctrl Pts',(6.15055246172042,-3.37155110156459,15.6139276036898));
#77414=CARTESIAN_POINT('Ctrl Pts',(6.24314950152241,-3.19683311189914,15.622895345035));
#77415=CARTESIAN_POINT('Ctrl Pts',(6.32820521176638,-3.0185170796722,15.6318630863802));
#77416=CARTESIAN_POINT('Ctrl Pts',(6.40909992728111,-2.84892441320293,15.6403921185034));
#77417=CARTESIAN_POINT('Ctrl Pts',(6.48317339141995,-2.67607762758904,15.6489211506266));
#77418=CARTESIAN_POINT('Ctrl Pts',(6.55018339351771,-2.50054475540529,15.6574501827497));
#77419=CARTESIAN_POINT('Ctrl Pts',(6.61719406589258,-2.3250101274289,15.6659793001857));
#77420=CARTESIAN_POINT('Ctrl Pts',(6.67714102887042,-2.14678964641217,15.6745084176218));
#77421=CARTESIAN_POINT('Ctrl Pts',(6.72983089626059,-1.96646959555351,15.6830375350578));
#77422=CARTESIAN_POINT('Ctrl Pts',(6.78253142480604,-1.78611305912071,15.6915683782572));
#77423=CARTESIAN_POINT('Ctrl Pts',(6.82797183996303,-1.60365639852797,15.7000992214567));
#77424=CARTESIAN_POINT('Ctrl Pts',(6.86600889366878,-1.41970012135,15.7086300646561));
#77425=CARTESIAN_POINT('Ctrl Pts',(6.87186874649866,-1.39136047339163,15.7099442959331));
#77426=CARTESIAN_POINT('Ctrl Pts',(6.8775529907978,-1.36298525616568,15.71125852721));
#77427=CARTESIAN_POINT('Ctrl Pts',(6.88306121050986,-1.33457668752101,15.712572758487));
#77428=CARTESIAN_POINT('Ctrl Pts',(6.91881612143904,-1.15017121812908,15.7211036858473));
#77429=CARTESIAN_POINT('Ctrl Pts',(6.9471622224435,-0.964296482546905,15.7296346132076));
#77430=CARTESIAN_POINT('Ctrl Pts',(6.9680000249124,-0.777561711583614,15.7381655405678));
#77431=CARTESIAN_POINT('Ctrl Pts',(6.98883387135136,-0.590862391975856,
15.7466948483425));
#77432=CARTESIAN_POINT('Ctrl Pts',(7.00216222993002,-0.403303667003667,
15.7552241561173));
#77433=CARTESIAN_POINT('Ctrl Pts',(7.00793734741366,-0.215501037641931,
15.763753463892));
#77434=CARTESIAN_POINT('Ctrl Pts',(7.01400932431902,-0.0180447553275768,
15.7727212052364));
#77435=CARTESIAN_POINT('Ctrl Pts',(7.0117310595895,0.17968080497015,15.7816889465807));
#77436=CARTESIAN_POINT('Ctrl Pts',(7.00110914759811,0.376957910008705,15.7906566879251));
#77437=CARTESIAN_POINT('Ctrl Pts',(6.99100686820331,0.564584058192902,15.7991857200499));
#77438=CARTESIAN_POINT('Ctrl Pts',(6.97335780402424,0.75180424923359,15.8077147521747));
#77439=CARTESIAN_POINT('Ctrl Pts',(6.94822102678319,0.93800379821618,15.8162437842995));
#77440=CARTESIAN_POINT('Ctrl Pts',(6.92308399810814,1.12420520968483,15.824772901737));
#77441=CARTESIAN_POINT('Ctrl Pts',(6.89045915088879,1.30938565568474,15.8333020191746));
#77442=CARTESIAN_POINT('Ctrl Pts',(6.85045716252722,1.49293778399487,15.8418311366122));
#77443=CARTESIAN_POINT('Ctrl Pts',(6.81044708024879,1.67652705185048,15.8503619798132));
#77444=CARTESIAN_POINT('Ctrl Pts',(6.7630569416163,1.85848704497405,15.8588928230141));
#77445=CARTESIAN_POINT('Ctrl Pts',(6.70844825699151,2.03822190788138,15.8674236662151));
#77446=CARTESIAN_POINT('Ctrl Pts',(6.7000354378544,2.06591121965774,15.8687378974849));
#77447=CARTESIAN_POINT('Ctrl Pts',(6.6914513948919,2.09354774952639,15.8700521287547));
#77448=CARTESIAN_POINT('Ctrl Pts',(6.68269682383722,2.12112935088268,15.8713663600245));
#77449=CARTESIAN_POINT('Ctrl Pts',(6.62586922322023,2.30016681787704,15.8798972873826));
#77450=CARTESIAN_POINT('Ctrl Pts',(6.56183281267897,2.47694989647158,15.8884282147407));
#77451=CARTESIAN_POINT('Ctrl Pts',(6.49079170234618,2.65089600687277,15.8969591420988));
#77452=CARTESIAN_POINT('Ctrl Pts',(6.41976407907667,2.82480909382896,15.9054884498714));
#77453=CARTESIAN_POINT('Ctrl Pts',(6.34173452556159,2.99588600406622,15.9140177576439));
#77454=CARTESIAN_POINT('Ctrl Pts',(6.25695558195389,3.16356340349867,15.9225470654165));
#77455=CARTESIAN_POINT('Ctrl Pts',(6.16781873074729,3.33985995507027,15.9315148067619));
#77456=CARTESIAN_POINT('Ctrl Pts',(6.07122048289653,3.5123979688746,15.9404825481074));
#77457=CARTESIAN_POINT('Ctrl Pts',(5.96751001349756,3.68055033946098,15.9494502894529));
#77458=CARTESIAN_POINT('Ctrl Pts',(5.86887314487242,3.84047655889336,15.9579793215755));
#77459=CARTESIAN_POINT('Ctrl Pts',(5.76380346821951,3.99643569594641,15.9665083536982));
#77460=CARTESIAN_POINT('Ctrl Pts',(5.65264693906213,4.14791624129653,15.9750373858208));
#77461=CARTESIAN_POINT('Ctrl Pts',(5.54148929804606,4.29939830185195,15.9835665032563));
#77462=CARTESIAN_POINT('Ctrl Pts',(5.4242448666277,4.44640143624321,15.9920956206917));
#77463=CARTESIAN_POINT('Ctrl Pts',(5.30130140845831,4.58844526383153,16.0006247381272));
#77464=CARTESIAN_POINT('Ctrl Pts',(5.17833307417169,4.7305178322651,16.0091555813261));
#77465=CARTESIAN_POINT('Ctrl Pts',(5.04966361108679,4.86762885876985,16.017686424525));
#77466=CARTESIAN_POINT('Ctrl Pts',(4.91571992023791,4.99933237825574,16.0262172677239));
#77467=CARTESIAN_POINT('Ctrl Pts',(4.89508503291352,5.01962215276915,16.0275314990033));
#77468=CARTESIAN_POINT('Ctrl Pts',(4.87432504185004,5.03978365965778,16.0288457302827));
#77469=CARTESIAN_POINT('Ctrl Pts',(4.85344158498705,5.05981534679067,16.0301599615621));
#77470=CARTESIAN_POINT('Ctrl Pts',(4.71788306016509,5.18984487088935,16.0386908889215));
#77471=CARTESIAN_POINT('Ctrl Pts',(4.57707285503567,5.31444585360377,16.0472218162808));
#77472=CARTESIAN_POINT('Ctrl Pts',(4.43146892713431,5.43320436854193,16.0557527436401));
#77473=CARTESIAN_POINT('Ctrl Pts',(4.28589264195185,5.5519403373284,16.0642820514138));
#77474=CARTESIAN_POINT('Ctrl Pts',(4.13552468734416,5.66483585838425,16.0728113591876));
#77475=CARTESIAN_POINT('Ctrl Pts',(3.98085634081318,5.7715170758049,16.0813406669613));
#77476=CARTESIAN_POINT('Ctrl Pts',(3.81823754891069,5.8836820474021,16.0903084083061));
#77477=CARTESIAN_POINT('Ctrl Pts',(3.65086490236855,5.98897679978346,16.099276149651));
#77478=CARTESIAN_POINT('Ctrl Pts',(3.47934504643782,6.08701771069615,16.1082438909959));
#77479=CARTESIAN_POINT('Ctrl Pts',(3.3162160817572,6.18026238028118,16.1167729231197));
#77480=CARTESIAN_POINT('Ctrl Pts',(3.14933626687556,6.26694580878486,16.1253019552436));
#77481=CARTESIAN_POINT('Ctrl Pts',(2.97925411531266,6.34678434160895,16.1338309873674));
#77482=CARTESIAN_POINT('Ctrl Pts',(2.8091702624791,6.42662367302921,16.1423601048041));
#77483=CARTESIAN_POINT('Ctrl Pts',(2.63588428751379,6.49961784478217,16.1508892222408));
#77484=CARTESIAN_POINT('Ctrl Pts',(2.45996652388457,6.56553053940558,16.1594183396775));
#77485=CARTESIAN_POINT('Ctrl Pts',(2.28401316543242,6.63145657066223,16.1679491828775));
#77486=CARTESIAN_POINT('Ctrl Pts',(2.10542724180266,6.69029815638646,16.1764800260775));
#77487=CARTESIAN_POINT('Ctrl Pts',(1.92479698862914,6.74186792477161,16.1850108692775));
#77488=CARTESIAN_POINT('Ctrl Pts',(1.89696973613013,6.74981257934058,16.1863251005515));
#77489=CARTESIAN_POINT('Ctrl Pts',(1.86909399370878,6.75758474548673,16.1876393318256));
#77490=CARTESIAN_POINT('Ctrl Pts',(1.84117194226723,6.76518384388096,16.1889535630996));
#77491=CARTESIAN_POINT('Ctrl Pts',(1.6599245489094,6.81451104960965,16.1974844904631));
#77492=CARTESIAN_POINT('Ctrl Pts',(1.47666268897109,6.85655875452296,16.2060154178265));
#77493=CARTESIAN_POINT('Ctrl Pts',(1.29198654137254,6.89118257916682,16.21454634519));
#77494=CARTESIAN_POINT('Ctrl Pts',(1.10734545430354,6.92579983052201,16.2230756529679));
#77495=CARTESIAN_POINT('Ctrl Pts',(0.921290916223461,6.95299595784342,16.2316049607458));
#77496=CARTESIAN_POINT('Ctrl Pts',(0.734433194305613,6.97267770986169,16.2401342685236));
#77497=CARTESIAN_POINT('Ctrl Pts',(0.537970390793006,6.99337116657229,16.2491020098664));
#77498=CARTESIAN_POINT('Ctrl Pts',(0.340620014977392,7.00575732159409,16.2580697512092));
#77499=CARTESIAN_POINT('Ctrl Pts',(0.143098313982019,7.00978954284902,16.267037492552));
#77500=CARTESIAN_POINT('Ctrl Pts',(-0.0447604644297263,7.0136245045541,
16.27556652468));
#77501=CARTESIAN_POINT('Ctrl Pts',(-0.232773874737426,7.00990335278436,
16.284095556808));
#77502=CARTESIAN_POINT('Ctrl Pts',(-0.420324544240595,6.99863942777515,
16.292624588936));
#77503=CARTESIAN_POINT('Ctrl Pts',(-0.607877089746412,6.98737539009691,
16.3011537063769));
#77504=CARTESIAN_POINT('Ctrl Pts',(-0.794966579746772,6.96856845001131,
16.3096828238178));
#77505=CARTESIAN_POINT('Ctrl Pts',(-0.980979128331375,6.94228395503081,
16.3182119412587));
#77506=CARTESIAN_POINT('Ctrl Pts',(-1.16702931429466,6.91599414170217,16.3267427844628));
#77507=CARTESIAN_POINT('Ctrl Pts',(-1.35200182054923,6.88222379533962,16.335273627667));
#77508=CARTESIAN_POINT('Ctrl Pts',(-1.53529045784463,6.84108980883538,16.3438044708711));
#77509=CARTESIAN_POINT('Ctrl Pts',(-1.56352725110343,6.83475285369201,16.3451187021265));
#77510=CARTESIAN_POINT('Ctrl Pts',(-1.5917241011711,6.82824123295892,16.3464329333818));
#77511=CARTESIAN_POINT('Ctrl Pts',(-1.61987881577253,6.82155548131886,16.3477471646371));
#77512=CARTESIAN_POINT('Ctrl Pts',(-1.80263647253457,6.77815698409637,16.3562780919815));
#77513=CARTESIAN_POINT('Ctrl Pts',(-1.98368036090121,6.72740238701715,16.3648090193258));
#77514=CARTESIAN_POINT('Ctrl Pts',(-2.16241437270051,6.66945204969931,16.3733399466702));
#77515=CARTESIAN_POINT('Ctrl Pts',(-2.34111445207794,6.61151271417835,16.381869254429));
#77516=CARTESIAN_POINT('Ctrl Pts',(-2.51750523886751,6.5463804590188,16.3903985621877));
#77517=CARTESIAN_POINT('Ctrl Pts',(-2.69100622734431,6.47426536735205,16.3989278699465));
#77518=CARTESIAN_POINT('Ctrl Pts',(-2.87342571941059,6.39844333021178,16.4078956112989));
#77519=CARTESIAN_POINT('Ctrl Pts',(-3.05265015788515,6.31490179316538,16.4168633526512));
#77520=CARTESIAN_POINT('Ctrl Pts',(-3.22802827723604,6.22394248076447,16.4258310940035));
#77521=CARTESIAN_POINT('Ctrl Pts',(-3.39482675551182,6.13743297233983,16.4343601261124));
#77522=CARTESIAN_POINT('Ctrl Pts',(-3.55814595624871,6.04421426208676,16.4428891582213));
#77523=CARTESIAN_POINT('Ctrl Pts',(-3.71745013063991,5.94459343342379,16.4514181903302));
#77524=CARTESIAN_POINT('Ctrl Pts',(-3.87675589849528,5.84497160828839,16.4599473077521));
#77525=CARTESIAN_POINT('Ctrl Pts',(-4.03204630186012,5.73894770187934,16.4684764251739));
#77526=CARTESIAN_POINT('Ctrl Pts',(-4.18281353555963,5.62687279838803,16.4770055425957));
#77527=CARTESIAN_POINT('Ctrl Pts',(-4.33361127518242,5.51477521789772,16.4855363857811));
#77528=CARTESIAN_POINT('Ctrl Pts',(-4.47988377199704,5.39662437836349,16.4940672289665));
#77529=CARTESIAN_POINT('Ctrl Pts',(-4.62115464027263,5.27281294502154,16.502598072152));
#77530=CARTESIAN_POINT('Ctrl Pts',(-4.64291832747283,5.25373899623116,16.5039123034928));
#77531=CARTESIAN_POINT('Ctrl Pts',(-4.66456337440864,5.23453077896803,16.5052265348337));
#77532=CARTESIAN_POINT('Ctrl Pts',(-4.68608811179318,5.21518981159944,16.5065407661746));
#77533=CARTESIAN_POINT('Ctrl Pts',(-4.82580898526699,5.08964417513982,16.515071674014));
#77534=CARTESIAN_POINT('Ctrl Pts',(-4.9605056051731,4.95845889673718,16.5236025818534));
#77535=CARTESIAN_POINT('Ctrl Pts',(-5.08973123700736,4.82205998485414,16.5321334896928));
#77536=CARTESIAN_POINT('Ctrl Pts',(-5.21893223860777,4.68568707042261,16.5406627715525));
#77537=CARTESIAN_POINT('Ctrl Pts',(-5.34266412260317,4.54410272777213,16.5491920534121));
#77538=CARTESIAN_POINT('Ctrl Pts',(-5.46051764513451,4.39776916284548,16.5577213352718));
#77539=CARTESIAN_POINT('Ctrl Pts',(-5.57862951534997,4.25111481889759,16.566269314241));
#77540=CARTESIAN_POINT('Ctrl Pts',(-5.69083701234519,4.09969063387712,16.5748172932102));
#77541=CARTESIAN_POINT('Ctrl Pts',(-5.79676882468995,3.94399515156937,16.5833652721794));
#77542=CARTESIAN_POINT('Ctrl Pts',(-5.90246402738797,3.78864743120634,16.5918941583544));
#77543=CARTESIAN_POINT('Ctrl Pts',(-6.00191139183001,3.62904773780094,16.6004230445295));
#77544=CARTESIAN_POINT('Ctrl Pts',(-6.09478521133198,3.46572067400548,16.6089519307045));
#77545=CARTESIAN_POINT('Ctrl Pts',(-6.18797089231485,3.30184517341417,16.6175094560708));
#77546=CARTESIAN_POINT('Ctrl Pts',(-6.27453863167416,3.13421748467873,16.626066981437));
#77547=CARTESIAN_POINT('Ctrl Pts',(-6.35420545475499,2.96339325794973,16.6346245068033));
#77548=CARTESIAN_POINT('Ctrl Pts',(-6.43387227783583,2.79256903122072,16.6431820321695));
#77549=CARTESIAN_POINT('Ctrl Pts',(-6.50663805954855,2.61854855142873,16.6517395575358));
#77550=CARTESIAN_POINT('Ctrl Pts',(-6.57226799596304,2.44190907933527,16.660297082902));
#77551=CARTESIAN_POINT('Origin',(0.,0.,10.));
#77552=CARTESIAN_POINT('',(-6.57226799068689,2.44190909353574,18.6606197598975));
#77553=CARTESIAN_POINT('',(-6.57226799602084,2.4419090791797,18.1135379835087));
#77554=CARTESIAN_POINT('',(-6.57226799596304,2.44190907933527,10.));
#77555=CARTESIAN_POINT('',(5.31037376991263,4.57794244025893,20.));
#77556=CARTESIAN_POINT('Ctrl Pts',(5.31037376991263,4.57794244025893,20.));
#77557=CARTESIAN_POINT('Ctrl Pts',(5.55565403033897,4.29341945242257,19.9829453662211));
#77558=CARTESIAN_POINT('Ctrl Pts',(5.77767458878684,3.98964000774632,19.9662196358398));
#77559=CARTESIAN_POINT('Ctrl Pts',(6.08131410266316,3.49529120368377,19.940098230979));
#77560=CARTESIAN_POINT('Ctrl Pts',(6.1806630589801,3.31645053343412,19.9308546963185));
#77561=CARTESIAN_POINT('Ctrl Pts',(6.41359417612191,2.85021658136766,19.907128727684));
#77562=CARTESIAN_POINT('Ctrl Pts',(6.53577546978317,2.5576468760439,19.8925703550586));
#77563=CARTESIAN_POINT('Ctrl Pts',(6.69473545277011,2.0903225110574,19.8698046355055));
#77564=CARTESIAN_POINT('Ctrl Pts',(6.74535157808797,1.92071957393734,19.8616423248671));
#77565=CARTESIAN_POINT('Ctrl Pts',(6.8152036502563,1.64961803264622,19.8488003608201));
#77566=CARTESIAN_POINT('Ctrl Pts',(6.83870751356947,1.54929681753912,19.8440923805288));
#77567=CARTESIAN_POINT('Ctrl Pts',(6.9143733926581,1.19094681265089,19.8274618806421));
#77568=CARTESIAN_POINT('Ctrl Pts',(6.95420852687898,0.930538557183069,19.8156952816196));
#77569=CARTESIAN_POINT('Ctrl Pts',(7.00881853782953,0.360400403229322,19.7900396878859));
#77570=CARTESIAN_POINT('Ctrl Pts',(7.017895173745,0.0506844751069775,19.7761629443979));
#77571=CARTESIAN_POINT('Ctrl Pts',(6.99209058764831,-0.648427924427146,
19.7444234601358));
#77572=CARTESIAN_POINT('Ctrl Pts',(6.94519564887154,-1.03635691554328,19.7265001555966));
#77573=CARTESIAN_POINT('Ctrl Pts',(6.82655782453199,-1.61068380040626,19.6995319153759));
#77574=CARTESIAN_POINT('Ctrl Pts',(6.77876578482327,-1.8012580651144,19.6905184966276));
#77575=CARTESIAN_POINT('Ctrl Pts',(6.65032448269472,-2.2352778291736,19.6699693779279));
#77576=CARTESIAN_POINT('Ctrl Pts',(6.56419733625245,-2.47681250315935,19.65850962379));
#77577=CARTESIAN_POINT('Ctrl Pts',(6.34902861498852,-2.98953904402741,19.6336010567148));
#77578=CARTESIAN_POINT('Ctrl Pts',(6.21540594260978,-3.25825620184757,19.620165435284));
#77579=CARTESIAN_POINT('Ctrl Pts',(5.83012947859726,-3.9225460193432,19.5853624107861));
#77580=CARTESIAN_POINT('Ctrl Pts',(5.55529778581468,-4.30295532809216,19.5638058413775));
#77581=CARTESIAN_POINT('Ctrl Pts',(5.14165688626341,-4.76917849267796,19.5351939530897));
#77582=CARTESIAN_POINT('Ctrl Pts',(5.03486121828757,-4.88178997914994,19.5280970198765));
#77583=CARTESIAN_POINT('Ctrl Pts',(4.74773465933112,-5.16509921326354,19.509814228205));
#77584=CARTESIAN_POINT('Ctrl Pts',(4.56191851216949,-5.32992844535567,19.4987169755029));
#77585=CARTESIAN_POINT('Ctrl Pts',(4.12664730964557,-5.67656647657017,19.4737940545565));
#77586=CARTESIAN_POINT('Ctrl Pts',(3.87314804944286,-5.85246486991511,19.4599770166617));
#77587=CARTESIAN_POINT('Ctrl Pts',(3.24938844208059,-6.2269526488941,19.4269736096934));
#77588=CARTESIAN_POINT('Ctrl Pts',(2.87124052423138,-6.4101036203911,19.4076836649396));
#77589=CARTESIAN_POINT('Ctrl Pts',(2.31094660388895,-6.62189052319189,19.3801419837845));
#77590=CARTESIAN_POINT('Ctrl Pts',(2.14049861486476,-6.67893524115426,19.3719020764516));
#77591=CARTESIAN_POINT('Ctrl Pts',(1.72437665409792,-6.80063266404377,19.3522215577717));
#77592=CARTESIAN_POINT('Ctrl Pts',(1.47701297532513,-6.85860891162722,19.3408675238262));
#77593=CARTESIAN_POINT('Ctrl Pts',(0.932207350322201,-6.95545063084083,
19.316082598644));
#77594=CARTESIAN_POINT('Ctrl Pts',(0.634316160635225,-6.98891576151712,
19.3026646152065));
#77595=CARTESIAN_POINT('Ctrl Pts',(-0.124644237268658,-7.02524261816539,
19.2682337929834));
#77596=CARTESIAN_POINT('Ctrl Pts',(-0.585535579499694,-7.00190686331401,
19.2470436360377));
#77597=CARTESIAN_POINT('Ctrl Pts',(-1.19980159345292,-6.90970025782923,
19.2185170065727));
#77598=CARTESIAN_POINT('Ctrl Pts',(-1.35794966021049,-6.88036744296449,
19.2111570507939));
#77599=CARTESIAN_POINT('Ctrl Pts',(-1.77425050592426,-6.78823912375196,
19.1918237362095));
#77600=CARTESIAN_POINT('Ctrl Pts',(-2.03008335220301,-6.71616862577159,
19.1799590454234));
#77601=CARTESIAN_POINT('Ctrl Pts',(-2.54972011497008,-6.53736841838324,
19.1553416626722));
#77602=CARTESIAN_POINT('Ctrl Pts',(-2.81236293520454,-6.42875336597622,
19.1426042906477));
#77603=CARTESIAN_POINT('Ctrl Pts',(-3.48462403918343,-6.10164008147154,
19.1087121466996));
#77604=CARTESIAN_POINT('Ctrl Pts',(-3.88039834917778,-5.85790973655747,
19.0873556188328));
#77605=CARTESIAN_POINT('Ctrl Pts',(-4.3727690342133,-5.48275957578848,19.0589313843948));
#77606=CARTESIAN_POINT('Ctrl Pts',(-4.49318056685592,-5.3845233618943,19.0518229749148));
#77607=CARTESIAN_POINT('Ctrl Pts',(-4.77148915802518,-5.1416271231717,19.0350754083327));
#77608=CARTESIAN_POINT('Ctrl Pts',(-4.92622018437202,-4.99357541539983,
19.0254867024873));
#77609=CARTESIAN_POINT('Ctrl Pts',(-5.23516438800496,-4.66961003420178,
19.0054335969687));
#77610=CARTESIAN_POINT('Ctrl Pts',(-5.38783954789928,-4.4925925650562,18.9949805237359));
#77611=CARTESIAN_POINT('Ctrl Pts',(-5.59301834925927,-4.22916425451325,
18.9799308442156));
#77612=CARTESIAN_POINT('Ctrl Pts',(-5.65293930776931,-4.14873010642308,
18.9753991570484));
#77613=CARTESIAN_POINT('Ctrl Pts',(-5.97047727161498,-3.70282940005589,
18.9505847048781));
#77614=CARTESIAN_POINT('Ctrl Pts',(-6.19440298925313,-3.31464917833267,
18.9300080082272));
#77615=CARTESIAN_POINT('Ctrl Pts',(-6.44880809220584,-2.75647615086778,
18.9018250263312));
#77616=CARTESIAN_POINT('Ctrl Pts',(-6.51237863114435,-2.60273185054225,
18.8942076656584));
#77617=CARTESIAN_POINT('Ctrl Pts',(-6.65046309758209,-2.23194254520588,
18.8762599453689));
#77618=CARTESIAN_POINT('Ctrl Pts',(-6.71991072903908,-2.01321378874463,
18.865991669355));
#77619=CARTESIAN_POINT('Ctrl Pts',(-6.83706346274827,-1.56993525329702,
18.8454543787509));
#77620=CARTESIAN_POINT('Ctrl Pts',(-6.88471681233285,-1.34566219767677,
18.8351972394528));
#77621=CARTESIAN_POINT('Ctrl Pts',(-6.93728882573627,-1.02062451566611,
18.8203517590086));
#77622=CARTESIAN_POINT('Ctrl Pts',(-6.95115568489195,-0.921458118086937,
18.8158259878938));
#77623=CARTESIAN_POINT('Ctrl Pts',(-7.01323504839045,-0.395622882039393,
18.7918147907539));
#77624=CARTESIAN_POINT('Ctrl Pts',(-7.02429911688816,0.0345009806129306,
18.7720628725));
#77625=CARTESIAN_POINT('Ctrl Pts',(-6.98755142286396,0.589862748977917,
18.7464806984229));
#77626=CARTESIAN_POINT('Ctrl Pts',(-6.97569749796841,0.716559743081308,
18.7406447006897));
#77627=CARTESIAN_POINT('Ctrl Pts',(-6.94460089884169,0.973356402409076,
18.7288464105356));
#77628=CARTESIAN_POINT('Ctrl Pts',(-6.92513284087342,1.1033766193804,18.7228976715111));
#77629=CARTESIAN_POINT('Ctrl Pts',(-6.85429960972639,1.49995522653845,18.7047562101925));
#77630=CARTESIAN_POINT('Ctrl Pts',(-6.79110456959091,1.76413981815084,18.6926508731029));
#77631=CARTESIAN_POINT('Ctrl Pts',(-6.67031407091704,2.16475174188527,18.6738737089538));
#77632=CARTESIAN_POINT('Ctrl Pts',(-6.6234614295815,2.30412468515178,18.6672617016403));
#77633=CARTESIAN_POINT('Ctrl Pts',(-6.57226799068689,2.44190909353574,18.6606197598975));
#77634=CARTESIAN_POINT('',(-5.31040820991542,4.5779024898487,19.999999977237));
#77635=CARTESIAN_POINT('Origin',(0.,0.,20.));
#77636=CARTESIAN_POINT('',(-7.01125027639237,-0.000179547635693209,18.226489882947));
#77637=CARTESIAN_POINT('Ctrl Pts',(-5.31040820991542,4.5779024898487,19.999999977237));
#77638=CARTESIAN_POINT('Ctrl Pts',(-5.18798945140932,4.71990935470875,19.9914851839));
#77639=CARTESIAN_POINT('Ctrl Pts',(-5.05984933106507,4.85702836085778,19.9829703905629));
#77640=CARTESIAN_POINT('Ctrl Pts',(-4.92640288943302,4.98880558184883,19.9744555972259));
#77641=CARTESIAN_POINT('Ctrl Pts',(-4.79298172464453,5.12055784217282,19.9659424167239));
#77642=CARTESIAN_POINT('Ctrl Pts',(-4.6542564637124,5.24697011976722,19.9574292362219));
#77643=CARTESIAN_POINT('Ctrl Pts',(-4.51067912035527,5.36762521378784,19.9489160557199));
#77644=CARTESIAN_POINT('Ctrl Pts',(-4.36709695434415,5.48828436052151,19.9404025892667));
#77645=CARTESIAN_POINT('Ctrl Pts',(-4.2186626136012,5.60318573534523,19.9318891228134));
#77646=CARTESIAN_POINT('Ctrl Pts',(-4.06586200678471,5.71195174211798,19.9233756563602));
#77647=CARTESIAN_POINT('Ctrl Pts',(-3.91306982999273,5.82071174825943,19.9148626595957));
#77648=CARTESIAN_POINT('Ctrl Pts',(-3.75591212076988,5.92333688501612,19.9063496628312));
#77649=CARTESIAN_POINT('Ctrl Pts',(-3.59490490813367,6.01949211013491,19.8978366660668));
#77650=CARTESIAN_POINT('Ctrl Pts',(-3.43385658166986,6.11567188887018,19.889321495475));
#77651=CARTESIAN_POINT('Ctrl Pts',(-3.26895705176141,6.20537829485712,19.8808063248831));
#77652=CARTESIAN_POINT('Ctrl Pts',(-3.10074907371748,6.28832105926059,19.8722911542913));
#77653=CARTESIAN_POINT('Ctrl Pts',(-2.94870341965684,6.36329423835694,19.8645941669241));
#77654=CARTESIAN_POINT('Ctrl Pts',(-2.79395503517537,6.4327416004527,19.8568971795569));
#77655=CARTESIAN_POINT('Ctrl Pts',(-2.63692048472963,6.49648188789235,19.8492001921897));
#77656=CARTESIAN_POINT('Ctrl Pts',(-2.46287341495907,6.56712755296231,19.8406693428096));
#77657=CARTESIAN_POINT('Ctrl Pts',(-2.28595593848525,6.63078694304454,19.8321384934295));
#77658=CARTESIAN_POINT('Ctrl Pts',(-2.10674665552219,6.68724495528211,19.8236076440493));
#77659=CARTESIAN_POINT('Ctrl Pts',(-1.92757135827927,6.74369226067363,19.815078412482));
#77660=CARTESIAN_POINT('Ctrl Pts',(-1.7461054138216,6.79294082162602,19.8065491809146));
#77661=CARTESIAN_POINT('Ctrl Pts',(-1.5629435514884,6.83482509047312,19.7980199493472));
#77662=CARTESIAN_POINT('Ctrl Pts',(-1.37036403797662,6.87886292681973,19.789052169456));
#77663=CARTESIAN_POINT('Ctrl Pts',(-1.17590996346703,6.91475912243078,19.7800843895647));
#77664=CARTESIAN_POINT('Ctrl Pts',(-0.980286876873871,6.94238173838985,
19.7711166096734));
#77665=CARTESIAN_POINT('Ctrl Pts',(-0.794236169154417,6.96865270332425,
19.7625876480642));
#77666=CARTESIAN_POINT('Ctrl Pts',(-0.607128448303999,6.98744038349346,
19.7540586864549));
#77667=CARTESIAN_POINT('Ctrl Pts',(-0.419578243030414,6.99868420922644,
19.7455297248456));
#77668=CARTESIAN_POINT('Ctrl Pts',(-0.232026111967852,7.00992815041243,
19.7370006756599));
#77669=CARTESIAN_POINT('Ctrl Pts',(-0.0440317932571628,7.01362806729796,
19.7284716264742));
#77670=CARTESIAN_POINT('Ctrl Pts',(0.143787428283975,7.00977544133673,19.7199425772885));
#77671=CARTESIAN_POINT('Ctrl Pts',(0.331644731820408,7.00592203422177,19.7114117987632));
#77672=CARTESIAN_POINT('Ctrl Pts',(0.519326561139531,6.99451303291472,19.7028810202379));
#77673=CARTESIAN_POINT('Ctrl Pts',(0.70621711009679,6.97559201472582,19.6943502417127));
#77674=CARTESIAN_POINT('Ctrl Pts',(0.735016010041088,6.97267638034673,19.6930356913592));
#77675=CARTESIAN_POINT('Ctrl Pts',(0.763796129616165,6.96958247142347,19.6917211410057));
#77676=CARTESIAN_POINT('Ctrl Pts',(0.792555226703233,6.96631055689634,19.6904065906522));
#77677=CARTESIAN_POINT('Ctrl Pts',(0.979182207176351,6.94507805690804,19.6818760529093));
#77678=CARTESIAN_POINT('Ctrl Pts',(1.16498755152204,6.91633800535125,19.6733455151664));
#77679=CARTESIAN_POINT('Ctrl Pts',(1.34936030466879,6.88017829207094,19.6648149774235));
#77680=CARTESIAN_POINT('Ctrl Pts',(1.53369791849532,6.84402547041491,19.6562860655027));
#77681=CARTESIAN_POINT('Ctrl Pts',(1.71660318558908,6.80045586793386,19.6477571535819));
#77682=CARTESIAN_POINT('Ctrl Pts',(1.89747469270541,6.74960860739662,19.6392282416612));
#77683=CARTESIAN_POINT('Ctrl Pts',(2.08765656171744,6.69614398382329,19.6302603039489));
#77684=CARTESIAN_POINT('Ctrl Pts',(2.27558941965171,6.63463278937865,19.6212923662367));
#77685=CARTESIAN_POINT('Ctrl Pts',(2.46059050773937,6.56529671193336,19.6123244285245));
#77686=CARTESIAN_POINT('Ctrl Pts',(2.6365289878981,6.4993571857825,19.6037958012199));
#77687=CARTESIAN_POINT('Ctrl Pts',(2.80981574927779,6.42634117637166,19.5952671739153));
#77688=CARTESIAN_POINT('Ctrl Pts',(2.97988221300527,6.34648946734451,19.5867385466107));
#77689=CARTESIAN_POINT('Ctrl Pts',(3.14995034945622,6.26663697291956,19.5782098354211));
#77690=CARTESIAN_POINT('Ctrl Pts',(3.31679784912225,6.17994877762485,19.5696811242314));
#77691=CARTESIAN_POINT('Ctrl Pts',(3.47987861391564,6.08671269199661,19.5611524130417));
#77692=CARTESIAN_POINT('Ctrl Pts',(3.6429923841662,5.99345773657931,19.5526219757502));
#77693=CARTESIAN_POINT('Ctrl Pts',(3.80233763150214,5.89365239680338,19.5440915384587));
#77694=CARTESIAN_POINT('Ctrl Pts',(3.95739447931174,5.78762952318244,19.5355611011672));
#77695=CARTESIAN_POINT('Ctrl Pts',(3.98131594971838,5.77127279292784,19.5342450638163));
#77696=CARTESIAN_POINT('Ctrl Pts',(4.00513540809726,5.75476816370005,19.5329290264655));
#77697=CARTESIAN_POINT('Ctrl Pts',(4.02885100789913,5.73811694884744,19.5316129891146));
#77698=CARTESIAN_POINT('Ctrl Pts',(4.18258888964484,5.63017439115037,19.5230816934143));
#77699=CARTESIAN_POINT('Ctrl Pts',(4.33201243443761,5.51603136176059,19.514550397714));
#77700=CARTESIAN_POINT('Ctrl Pts',(4.47662714238184,5.3960574487852,19.5060191020136));
#77701=CARTESIAN_POINT('Ctrl Pts',(4.62121448336393,5.27610623973516,19.4974894207801));
#77702=CARTESIAN_POINT('Ctrl Pts',(4.76099456804004,5.15032654452421,19.4889597395466));
#77703=CARTESIAN_POINT('Ctrl Pts',(4.8955057910262,5.01912837179215,19.4804300583131));
#77704=CARTESIAN_POINT('Ctrl Pts',(5.03692220244502,4.88119508741199,19.4714625024185));
#77705=CARTESIAN_POINT('Ctrl Pts',(5.17251429392865,4.73727261406377,19.4624949465238));
#77706=CARTESIAN_POINT('Ctrl Pts',(5.30178872069088,4.58788218284373,19.4535273906291));
#77707=CARTESIAN_POINT('Ctrl Pts',(5.42474695774191,4.44579078460535,19.4449979785011));
#77708=CARTESIAN_POINT('Ctrl Pts',(5.54198992424946,4.29875324043526,19.4364685663731));
#77709=CARTESIAN_POINT('Ctrl Pts',(5.65313348451946,4.14725311124181,19.4279391542451));
#77710=CARTESIAN_POINT('Ctrl Pts',(5.7642781654629,3.99575145445495,19.4194096561141));
#77711=CARTESIAN_POINT('Ctrl Pts',(5.86932313880391,3.83978737149075,19.4108801579831));
#77712=CARTESIAN_POINT('Ctrl Pts',(5.96792650977962,3.67987496205641,19.402350659852));
#77713=CARTESIAN_POINT('Ctrl Pts',(6.06654981684823,3.51993022077966,19.3938194371869));
#77714=CARTESIAN_POINT('Ctrl Pts',(6.15872876038105,3.35603581968886,19.3852882145219));
#77715=CARTESIAN_POINT('Ctrl Pts',(6.24416602015155,3.18873286358151,19.3767569918568));
#77716=CARTESIAN_POINT('Ctrl Pts',(6.2573106041863,3.16299318312217,19.3754444570969));
#77717=CARTESIAN_POINT('Ctrl Pts',(6.27029570105889,3.13717286887965,19.374131922337));
#77718=CARTESIAN_POINT('Ctrl Pts',(6.28312032557758,3.11127394113953,19.3728193875771));
#77719=CARTESIAN_POINT('Ctrl Pts',(6.36647279498715,2.94294623851925,19.3642886884315));
#77720=CARTESIAN_POINT('Ctrl Pts',(6.44307130431841,2.77123815692641,19.3557579892859));
#77721=CARTESIAN_POINT('Ctrl Pts',(6.51265843964136,2.5967107291857,19.3472272901403));
#77722=CARTESIAN_POINT('Ctrl Pts',(6.58223233947808,2.42221649659459,19.3386982135353));
#77723=CARTESIAN_POINT('Ctrl Pts',(6.6447974132034,2.24490427231277,19.3301691369303));
#77724=CARTESIAN_POINT('Ctrl Pts',(6.70014446921764,2.06535484944168,19.3216400603253));
#77725=CARTESIAN_POINT('Ctrl Pts',(6.75833886257202,1.87656848041739,19.3126722041348));
#77726=CARTESIAN_POINT('Ctrl Pts',(6.80855287612425,1.68530900095786,19.3037043479443));
#77727=CARTESIAN_POINT('Ctrl Pts',(6.85060260265691,1.49227026472099,19.2947364917539));
#77728=CARTESIAN_POINT('Ctrl Pts',(6.89059360966207,1.30868254395132,19.2862076943203));
#77729=CARTESIAN_POINT('Ctrl Pts',(6.92320057024404,1.12348594464433,19.2776788968867));
#77730=CARTESIAN_POINT('Ctrl Pts',(6.94831751475442,0.937288790425337,19.2691500994531));
#77731=CARTESIAN_POINT('Ctrl Pts',(6.97343470978042,0.751089779081735,19.2606212169536));
#77732=CARTESIAN_POINT('Ctrl Pts',(6.99106170173282,0.563890496800545,19.252092334454));
#77733=CARTESIAN_POINT('Ctrl Pts',(7.0011442243662,0.376305875749824,19.2435634519545));
#77734=CARTESIAN_POINT('Ctrl Pts',(7.01122878832538,0.188683275976775,19.2350328426819));
#77735=CARTESIAN_POINT('Ctrl Pts',(7.01376581664533,0.000675487465281344,
19.2265022334094));
#77736=CARTESIAN_POINT('Ctrl Pts',(7.00875310516585,-0.187100169235761,
19.2179716241368));
#77737=CARTESIAN_POINT('Ctrl Pts',(7.00798022766499,-0.216052080964084,
19.2166563447711));
#77738=CARTESIAN_POINT('Ctrl Pts',(7.00702797435457,-0.244998475659424,
19.2153410654053));
#77739=CARTESIAN_POINT('Ctrl Pts',(7.00589644736758,-0.273937093622513,
19.2140257860396));
#77740=CARTESIAN_POINT('Ctrl Pts',(6.99855724805962,-0.461635917751245,
19.2054947500839));
#77741=CARTESIAN_POINT('Ctrl Pts',(6.98366933982935,-0.649071725155701,
19.1969637141282));
#77742=CARTESIAN_POINT('Ctrl Pts',(6.96127512095335,-0.835628657296986,
19.1884326781726));
#77743=CARTESIAN_POINT('Ctrl Pts',(6.9388851500791,-1.02215020110084,19.1799032604852));
#77744=CARTESIAN_POINT('Ctrl Pts',(6.90899174655451,-1.20779289846891,19.1713738427979));
#77745=CARTESIAN_POINT('Ctrl Pts',(6.87168910763913,-1.39194661192652,19.1628444251106));
#77746=CARTESIAN_POINT('Ctrl Pts',(6.83246973865202,-1.58556273798198,19.1538767383932));
#77747=CARTESIAN_POINT('Ctrl Pts',(6.78505972286755,-1.77753247551099,19.1449090516758));
#77748=CARTESIAN_POINT('Ctrl Pts',(6.72962952354261,-1.9671586205397,19.1359413649585));
#77749=CARTESIAN_POINT('Ctrl Pts',(6.67691000526172,-2.14751155343776,19.1274122214664));
#77750=CARTESIAN_POINT('Ctrl Pts',(6.61693607122333,-2.32574431516057,19.1188830779744));
#77751=CARTESIAN_POINT('Ctrl Pts',(6.54990572828462,-2.50127197903073,19.1103539344824));
#77752=CARTESIAN_POINT('Ctrl Pts',(6.48287471454436,-2.67680139948192,19.1018247056355));
#77753=CARTESIAN_POINT('Ctrl Pts',(6.40878726305569,-2.84962538310911,19.0932954767887));
#77754=CARTESIAN_POINT('Ctrl Pts',(6.32788994435908,-3.01917793688601,19.0847662479419));
#77755=CARTESIAN_POINT('Ctrl Pts',(6.24697626283045,-3.18876478549493,19.0762352939162));
#77756=CARTESIAN_POINT('Ctrl Pts',(6.1592500956831,-3.35507860668506,19.0677043398906));
#77757=CARTESIAN_POINT('Ctrl Pts',(6.06500487318369,-3.51757621818748,19.0591733858649));
#77758=CARTESIAN_POINT('Ctrl Pts',(6.0504914749463,-3.5426002192542,19.0578596520773));
#77759=CARTESIAN_POINT('Ctrl Pts',(6.03582356627391,-3.56753376894369,19.0565459182897));
#77760=CARTESIAN_POINT('Ctrl Pts',(6.02100231375902,-3.59237493870121,19.0552321845021));
#77761=CARTESIAN_POINT('Ctrl Pts',(5.92475871613629,-3.75368408205597,19.0467012950977));
#77762=CARTESIAN_POINT('Ctrl Pts',(5.82201244059844,-3.91115091479425,19.0381704056934));
#77763=CARTESIAN_POINT('Ctrl Pts',(5.71309534362803,-4.06425493259413,19.029639516289));
#77764=CARTESIAN_POINT('Ctrl Pts',(5.60419892977575,-4.21732987627641,19.0211102468818));
#77765=CARTESIAN_POINT('Ctrl Pts',(5.48913421041692,-4.36604340895412,19.0125809774747));
#77766=CARTESIAN_POINT('Ctrl Pts',(5.36827579144815,-4.50990483152935,19.0040517080675));
#77767=CARTESIAN_POINT('Ctrl Pts',(5.24120402305307,-4.66116219139263,18.9950839476423));
#77768=CARTESIAN_POINT('Ctrl Pts',(5.10772737401113,-4.80705511621083,18.986116187217));
#77769=CARTESIAN_POINT('Ctrl Pts',(4.96832911193144,-4.94705290026643,18.9771484267918));
#77770=CARTESIAN_POINT('Ctrl Pts',(4.83575121102563,-5.08020099024009,18.9686194334222));
#77771=CARTESIAN_POINT('Ctrl Pts',(4.69781753508435,-5.20801678046617,18.9600904400527));
#77772=CARTESIAN_POINT('Ctrl Pts',(4.55498178807121,-5.33008137581779,18.9515614466831));
#77773=CARTESIAN_POINT('Ctrl Pts',(4.41214461187468,-5.45214719252117,18.9430323679743));
#77774=CARTESIAN_POINT('Ctrl Pts',(4.26440550148309,-5.56846150289737,18.9345032892655));
#77775=CARTESIAN_POINT('Ctrl Pts',(4.11225174759387,-5.67864527214997,18.9259742105567));
#77776=CARTESIAN_POINT('Ctrl Pts',(3.96006720244786,-5.7888513392207,18.9174434058238));
#77777=CARTESIAN_POINT('Ctrl Pts',(3.80346647799771,-5.89292420839794,18.9089126010908));
#77778=CARTESIAN_POINT('Ctrl Pts',(3.6429671003538,-5.99052729467447,18.9003817963578));
#77779=CARTESIAN_POINT('Ctrl Pts',(3.61823776881749,-6.00556572731472,18.8990673918934));
#77780=CARTESIAN_POINT('Ctrl Pts',(3.59341593729415,-6.02045065357043,18.897752987429));
#77781=CARTESIAN_POINT('Ctrl Pts',(3.56850355590312,-6.03518093631059,18.8964385829646));
#77782=CARTESIAN_POINT('Ctrl Pts',(3.40681370596188,-6.13078549407908,18.8879076498001));
#77783=CARTESIAN_POINT('Ctrl Pts',(3.24125192648159,-6.21990487450771,18.8793767166356));
#77784=CARTESIAN_POINT('Ctrl Pts',(3.07235866038221,-6.30224077804668,18.8708457834711));
#77785=CARTESIAN_POINT('Ctrl Pts',(2.90349745789746,-6.3845610504907,18.8623164698653));
#77786=CARTESIAN_POINT('Ctrl Pts',(2.73130630606696,-6.46010028189103,18.8537871562595));
#77787=CARTESIAN_POINT('Ctrl Pts',(2.55634892730108,-6.52860679811448,18.8452578426536));
#77788=CARTESIAN_POINT('Ctrl Pts',(2.37239836777744,-6.60063469473256,18.8362901042181));
#77789=CARTESIAN_POINT('Ctrl Pts',(2.18539004318896,-6.66488769423388,18.8273223657825));
#77790=CARTESIAN_POINT('Ctrl Pts',(1.99600222015603,-6.72113098366876,18.818354627347));
#77791=CARTESIAN_POINT('Ctrl Pts',(1.81587922292988,-6.77462285925311,18.8098255894211));
#77792=CARTESIAN_POINT('Ctrl Pts',(1.63360429009838,-6.82086986851293,18.8012965514952));
#77793=CARTESIAN_POINT('Ctrl Pts',(1.44977624868172,-6.85972123276583,18.7927675135693));
#77794=CARTESIAN_POINT('Ctrl Pts',(1.26594636924264,-6.89857298547785,18.784238390365));
#77795=CARTESIAN_POINT('Ctrl Pts',(1.08056365043727,-6.9300288852799,18.7757092671606));
#77796=CARTESIAN_POINT('Ctrl Pts',(0.894237342332065,-6.95398922476005,
18.7671801439563));
#77797=CARTESIAN_POINT('Ctrl Pts',(0.707873335172129,-6.97795441209104,
18.7586492950704));
#77798=CARTESIAN_POINT('Ctrl Pts',(0.520565661225884,-6.99442097193293,
18.7501184461845));
#77799=CARTESIAN_POINT('Ctrl Pts',(0.332929811888472,-7.00334093864178,
18.7415875972986));
#77800=CARTESIAN_POINT('Ctrl Pts',(0.304023893006349,-7.00471508881099,
18.740273392008));
#77801=CARTESIAN_POINT('Ctrl Pts',(0.275110191864145,-7.00591024057634,
18.7389591867175));
#77802=CARTESIAN_POINT('Ctrl Pts',(0.246190963911276,-7.00692632841166,
18.737644981427));
#77803=CARTESIAN_POINT('Ctrl Pts',(0.0584668930673313,-7.01352208349517,
18.7291140494303));
#77804=CARTESIAN_POINT('Ctrl Pts',(-0.129554522942743,-7.01257059255586,
18.7205831174336));
#77805=CARTESIAN_POINT('Ctrl Pts',(-0.31725599199883,-7.00406847468247,
18.7120521854369));
#77806=CARTESIAN_POINT('Ctrl Pts',(-0.504921828007146,-6.99556797084212,
18.7035228729433));
#77807=CARTESIAN_POINT('Ctrl Pts',(-0.692267532516735,-6.97951971442561,
18.6949935604497));
#77808=CARTESIAN_POINT('Ctrl Pts',(-0.878677678046428,-6.95597240510649,
18.6864642479561));
#77809=CARTESIAN_POINT('Ctrl Pts',(-1.07466973887797,-6.93121470928806,
18.6774965089506));
#77810=CARTESIAN_POINT('Ctrl Pts',(-1.26962716618774,-6.89816674783037,
18.668528769945));
#77811=CARTESIAN_POINT('Ctrl Pts',(-1.46284201475234,-6.85694682802597,
18.6595610309395));
#77812=CARTESIAN_POINT('Ctrl Pts',(-1.64660478770015,-6.81774338781308,
18.6510319939686));
#77813=CARTESIAN_POINT('Ctrl Pts',(-1.82879107709652,-6.77114849393829,
18.6425029569977));
#77814=CARTESIAN_POINT('Ctrl Pts',(-2.00880290052994,-6.71731624008596,
18.6339739200268));
#77815=CARTESIAN_POINT('Ctrl Pts',(-2.18881652506152,-6.66348344761803,
18.6254447977191));
#77816=CARTESIAN_POINT('Ctrl Pts',(-2.36665534772529,-6.60241324131081,
18.6169156754114));
#77817=CARTESIAN_POINT('Ctrl Pts',(-2.5417366673616,-6.53430954855137,18.6083865531037));
#77818=CARTESIAN_POINT('Ctrl Pts',(-2.7168534126708,-6.46619207580016,18.5998557050271));
#77819=CARTESIAN_POINT('Ctrl Pts',(-2.88921125551704,-6.39103838602187,
18.5913248569505));
#77820=CARTESIAN_POINT('Ctrl Pts',(-3.05824676884958,-6.30910082843198,
18.582794008874));
#77821=CARTESIAN_POINT('Ctrl Pts',(-3.08428733395646,-6.29647803538067,
18.5814797992125));
#77822=CARTESIAN_POINT('Ctrl Pts',(-3.11024909430534,-6.28369433482796,
18.580165589551));
#77823=CARTESIAN_POINT('Ctrl Pts',(-3.13613003795766,-6.27075074831712,
18.5788513798895));
#77824=CARTESIAN_POINT('Ctrl Pts',(-3.30413086052554,-6.18673011869823,
18.5703204581765));
#77825=CARTESIAN_POINT('Ctrl Pts',(-3.46878197991479,-6.09593981105469,
18.5617895364636));
#77826=CARTESIAN_POINT('Ctrl Pts',(-3.62953971911893,-5.99867218556224,
18.5532586147506));
#77827=CARTESIAN_POINT('Ctrl Pts',(-3.79026693713249,-5.90142302713552,
18.5447293127039));
#77828=CARTESIAN_POINT('Ctrl Pts',(-3.94710198822778,-5.79769916344609,
18.5362000106572));
#77829=CARTESIAN_POINT('Ctrl Pts',(-4.09952774958241,-5.68783779593826,
18.5276707086105));
#77830=CARTESIAN_POINT('Ctrl Pts',(-4.25978883871199,-5.57232909023393,
18.5187029644223));
#77831=CARTESIAN_POINT('Ctrl Pts',(-4.41517508286484,-5.45003547304751,
18.509735220234));
#77832=CARTESIAN_POINT('Ctrl Pts',(-4.56512141629977,-5.32139953554901,
18.5007674760458));
#77833=CARTESIAN_POINT('Ctrl Pts',(-4.70773211005469,-5.19905669549259,
18.4922384497549));
#77834=CARTESIAN_POINT('Ctrl Pts',(-4.84542218018709,-5.07097747392741,
18.483709423464));
#77835=CARTESIAN_POINT('Ctrl Pts',(-4.97774024638283,-4.93758327545376,
18.475180397173));
#77836=CARTESIAN_POINT('Ctrl Pts',(-5.11005963591569,-4.80418774288039,
18.4666512855817));
#77837=CARTESIAN_POINT('Ctrl Pts',(-5.23700670082084,-4.66547734685421,
18.4581221739904));
#77838=CARTESIAN_POINT('Ctrl Pts',(-5.35816732152366,-4.521909941281,18.4495930623992));
#77839=CARTESIAN_POINT('Ctrl Pts',(-5.47935245785444,-4.37831348629323,
18.4410622250283));
#77840=CARTESIAN_POINT('Ctrl Pts',(-5.59474861470344,-4.22985829349008,
18.4325313876574));
#77841=CARTESIAN_POINT('Ctrl Pts',(-5.70398176399658,-4.07703551597169,
18.4240005502865));
#77842=CARTESIAN_POINT('Ctrl Pts',(-5.72081017823964,-4.05349170145661,
18.422686292975));
#77843=CARTESIAN_POINT('Ctrl Pts',(-5.73749239856006,-4.02984428476107,
18.4213720356635));
#77844=CARTESIAN_POINT('Ctrl Pts',(-5.75402714681736,-4.00609512570394,
18.420057778352));
#77845=CARTESIAN_POINT('Ctrl Pts',(-5.86135529224486,-3.85193776222923,
18.411526847148));
#77846=CARTESIAN_POINT('Ctrl Pts',(-5.96250314914113,-3.69343835465417,
18.402995915944));
#77847=CARTESIAN_POINT('Ctrl Pts',(-6.05713317387302,-3.53111374448161,
18.39446498474));
#77848=CARTESIAN_POINT('Ctrl Pts',(-6.15174523378733,-3.3688199504482,18.3859356730708));
#77849=CARTESIAN_POINT('Ctrl Pts',(-6.23984177667961,-3.20270266741765,
18.3774063614017));
#77850=CARTESIAN_POINT('Ctrl Pts',(-6.32113003023968,-3.03330540884069,
18.3688770497325));
#77851=CARTESIAN_POINT('Ctrl Pts',(-6.40659670132452,-2.85520071169926,
18.3599093103227));
#77852=CARTESIAN_POINT('Ctrl Pts',(-6.48453655148899,-2.67347028005893,
18.3509415709129));
#77853=CARTESIAN_POINT('Ctrl Pts',(-6.55466513137106,-2.48877310699236,
18.341973831503));
#77854=CARTESIAN_POINT('Ctrl Pts',(-6.62136300926237,-2.31311135087554,
18.3334447954221));
#77855=CARTESIAN_POINT('Ctrl Pts',(-6.68099549066131,-2.134766492544,18.3249157593412));
#77856=CARTESIAN_POINT('Ctrl Pts',(-6.7333678186597,-1.95432453321805,18.3163867232603));
#77857=CARTESIAN_POINT('Ctrl Pts',(-6.78574067054998,-1.77388076889159,
18.3078576018615));
#77858=CARTESIAN_POINT('Ctrl Pts',(-6.83085314168356,-1.59134015661709,
18.2993284804628));
#77859=CARTESIAN_POINT('Ctrl Pts',(-6.8685606331945,-1.40730287807238,18.290799359064));
#77860=CARTESIAN_POINT('Ctrl Pts',(-6.90627575428454,-1.22322836217992,
18.2822685119179));
#77861=CARTESIAN_POINT('Ctrl Pts',(-6.93658284265557,-1.03765687534071,
18.2737376647717));
#77862=CARTESIAN_POINT('Ctrl Pts',(-6.95938843614138,-0.851198659186938,
18.2652068176255));
#77863=CARTESIAN_POINT('Ctrl Pts',(-6.96290173566313,-0.822473971006945,
18.2638926040219));
#77864=CARTESIAN_POINT('Ctrl Pts',(-6.96623710401648,-0.79372825189046,
18.2625783904182));
#77865=CARTESIAN_POINT('Ctrl Pts',(-6.96939430864683,-0.764963746265907,
18.2612641768145));
#77866=CARTESIAN_POINT('Ctrl Pts',(-6.99107740060903,-0.567414491869339,
18.2522384031436));
#77867=CARTESIAN_POINT('Ctrl Pts',(-7.00435755886076,-0.368935936278,18.2432126294727));
#77868=CARTESIAN_POINT('Ctrl Pts',(-7.00918342474411,-0.170218332715454,
18.2341868558018));
#77869=CARTESIAN_POINT('Ctrl Pts',(-7.0105595408299,-0.113553166836021,
18.2316131182311));
#77870=CARTESIAN_POINT('Ctrl Pts',(-7.01124853702015,-0.0568685892723279,
18.2290393806603));
#77871=CARTESIAN_POINT('Ctrl Pts',(-7.01124999767256,-0.000180655715778411,
18.2264656430896));
#77872=CARTESIAN_POINT('Ctrl Pts',(-7.01124999770178,-0.00017951820933601,
18.2264903645786));
#77873=CARTESIAN_POINT('Ctrl Pts',(-7.01125577494277,0.225455981633749,
18.2161082295559));
#77874=CARTESIAN_POINT('Ctrl Pts',(-7.00036947495541,0.45096251588819,18.2057421677263));
#77875=CARTESIAN_POINT('Ctrl Pts',(-6.96472858178406,0.819141872311974,
18.1888528438194));
#77876=CARTESIAN_POINT('Ctrl Pts',(-6.94640026963132,0.962269013776619,
18.1822947481454));
#77877=CARTESIAN_POINT('Ctrl Pts',(-6.85270045561988,1.54951348992101,18.1553737625081));
#77878=CARTESIAN_POINT('Ctrl Pts',(-6.73903764732082,1.98641993334926,18.1353824772627));
#77879=CARTESIAN_POINT('Ctrl Pts',(-6.58028721034065,2.4202438351479,18.1145789804434));
#77880=CARTESIAN_POINT('Ctrl Pts',(-6.57629094993498,2.43108151336865,18.1140585918785));
#77881=CARTESIAN_POINT('Ctrl Pts',(-6.57226799602084,2.4419090791797,18.1135379835087));
#77882=CARTESIAN_POINT('Origin',(0.,0.,10.));
#77883=CARTESIAN_POINT('Ctrl Pts',(-6.57226799602084,2.4419090791797,18.1135379835087));
#77884=CARTESIAN_POINT('Ctrl Pts',(-6.53133773793476,2.55207068494202,18.1082412201375));
#77885=CARTESIAN_POINT('Ctrl Pts',(-6.48764442560255,2.6611854159813,18.1029188956554));
#77886=CARTESIAN_POINT('Ctrl Pts',(-6.30695942002566,3.08147038585748,18.0820569411487));
#77887=CARTESIAN_POINT('Ctrl Pts',(-6.15015392438222,3.38360801034555,18.0663501241534));
#77888=CARTESIAN_POINT('Ctrl Pts',(-5.86864123543347,3.84130686026723,18.0416943762633));
#77889=CARTESIAN_POINT('Ctrl Pts',(-5.75817549473653,4.00499751101801,18.0326790081895));
#77890=CARTESIAN_POINT('Ctrl Pts',(-5.39944115363625,4.4909951943229,18.0052513848175));
#77891=CARTESIAN_POINT('Ctrl Pts',(-5.12992452278029,4.79654896948932,17.9871027008005));
#77892=CARTESIAN_POINT('Ctrl Pts',(-4.69960032454455,5.20639762371295,17.9604604173751));
#77893=CARTESIAN_POINT('Ctrl Pts',(-4.55861995612133,5.33027220463726,17.952033971876));
#77894=CARTESIAN_POINT('Ctrl Pts',(-4.21508981287583,5.60851188158642,17.9319478743448));
#77895=CARTESIAN_POINT('Ctrl Pts',(-4.00876384610101,5.75779448881512,17.9202319016981));
#77896=CARTESIAN_POINT('Ctrl Pts',(-3.5436809163475,6.05715507631821,17.8947825417151));
#77897=CARTESIAN_POINT('Ctrl Pts',(-3.28250574277425,6.20257714731901,17.8810827646505));
#77898=CARTESIAN_POINT('Ctrl Pts',(-2.79124019713527,6.43636850206716,17.8563510001969));
#77899=CARTESIAN_POINT('Ctrl Pts',(-2.5642408750039,6.53012504120916,17.8452919196435));
#77900=CARTESIAN_POINT('Ctrl Pts',(-2.11497689976914,6.68863573172338,17.8239116387394));
#77901=CARTESIAN_POINT('Ctrl Pts',(-1.89349946819157,6.75467501023395,17.8135973338988));
#77902=CARTESIAN_POINT('Ctrl Pts',(-1.52228723506105,6.84566566269185,17.7964290318575));
#77903=CARTESIAN_POINT('Ctrl Pts',(-1.37428288747775,6.87690647911858,17.7896118758936));
#77904=CARTESIAN_POINT('Ctrl Pts',(-0.98282969575925,6.94639175307489,17.7715185702293));
#77905=CARTESIAN_POINT('Ctrl Pts',(-0.738177543202611,6.97663273517866,
17.7601749637869));
#77906=CARTESIAN_POINT('Ctrl Pts',(-0.183398802384542,7.01569486897031,
17.7345861519763));
#77907=CARTESIAN_POINT('Ctrl Pts',(0.126754820707417,7.0169472577802,17.7203819579545));
#77908=CARTESIAN_POINT('Ctrl Pts',(0.846874154652356,6.97208169737093,17.687618328165));
#77909=CARTESIAN_POINT('Ctrl Pts',(1.25471991553141,6.91034021910658,17.6692493842604));
#77910=CARTESIAN_POINT('Ctrl Pts',(1.83421043486687,6.76959301527378,17.642511571504));
#77911=CARTESIAN_POINT('Ctrl Pts',(2.01183802309883,6.7189451289178,17.6342161601171));
#77912=CARTESIAN_POINT('Ctrl Pts',(2.42641487902089,6.58281859570323,17.6143884008321));
#77913=CARTESIAN_POINT('Ctrl Pts',(2.66116811632201,6.49146912758555,17.602800622479));
#77914=CARTESIAN_POINT('Ctrl Pts',(3.15600305987535,6.26755131160755,17.5778092829768));
#77915=CARTESIAN_POINT('Ctrl Pts',(3.41376406077169,6.13096847145579,17.5644362120504));
#77916=CARTESIAN_POINT('Ctrl Pts',(3.86482288946793,5.85467229233321,17.5403776519203));
#77917=CARTESIAN_POINT('Ctrl Pts',(4.06093352070668,5.72039031683214,17.5296647633831));
#77918=CARTESIAN_POINT('Ctrl Pts',(4.45285995469801,5.42169838677391,17.5075367241649));
#77919=CARTESIAN_POINT('Ctrl Pts',(4.64726673012376,5.25601431003394,17.4961458788654));
#77920=CARTESIAN_POINT('Ctrl Pts',(4.88354866598726,5.03126229743105,17.4814921676409));
#77921=CARTESIAN_POINT('Ctrl Pts',(4.93414858539626,4.98164887497338,17.4783022024546));
#77922=CARTESIAN_POINT('Ctrl Pts',(5.07353905926242,4.84076846240518,17.4693521145051));
#77923=CARTESIAN_POINT('Ctrl Pts',(5.16060638394841,4.74783936484442,17.4635638527226));
#77924=CARTESIAN_POINT('Ctrl Pts',(5.42826320812631,4.44609673030629,17.4451170301998));
#77925=CARTESIAN_POINT('Ctrl Pts',(5.5990773457441,4.22896559385304,17.4323824610446));
#77926=CARTESIAN_POINT('Ctrl Pts',(5.90138954951528,3.79414303750813,17.4080568591738));
#77927=CARTESIAN_POINT('Ctrl Pts',(6.03473533685795,3.57825279917168,17.3964737812563));
#77928=CARTESIAN_POINT('Ctrl Pts',(6.29037366494197,3.10926715376298,17.3722594653965));
#77929=CARTESIAN_POINT('Ctrl Pts',(6.40974632530941,2.85508291359299,17.3596717378527));
#77930=CARTESIAN_POINT('Ctrl Pts',(6.60837584665915,2.35640389469369,17.3356250786124));
#77931=CARTESIAN_POINT('Ctrl Pts',(6.69006400772755,2.11336480498559,17.3241785838793));
#77932=CARTESIAN_POINT('Ctrl Pts',(6.79564330085926,1.73106141829922,17.3062202441551));
#77933=CARTESIAN_POINT('Ctrl Pts',(6.8289457084578,1.59462860734483,17.2998097485968));
#77934=CARTESIAN_POINT('Ctrl Pts',(6.91332233390364,1.19754536294385,17.2811943685785));
#77935=CARTESIAN_POINT('Ctrl Pts',(6.95371495757701,0.934873996140607,17.2689473466327));
#77936=CARTESIAN_POINT('Ctrl Pts',(6.99798936661613,0.474061066159394,17.2477059060085));
#77937=CARTESIAN_POINT('Ctrl Pts',(7.0085616606389,0.276865067678228,17.2386905353353));
#77938=CARTESIAN_POINT('Ctrl Pts',(7.01540315346882,-0.326580580999011,
17.2112891308239));
#77939=CARTESIAN_POINT('Ctrl Pts',(6.98471968828257,-0.732278758725528,
17.1931655772121));
#77940=CARTESIAN_POINT('Ctrl Pts',(6.88872141348215,-1.31850892653739,17.1665339124638));
#77941=CARTESIAN_POINT('Ctrl Pts',(6.85090468186664,-1.50268153047177,17.1580922539858));
#77942=CARTESIAN_POINT('Ctrl Pts',(6.7444976813099,-1.93243280045099,17.1379766420135));
#77943=CARTESIAN_POINT('Ctrl Pts',(6.66982445252792,-2.17623173407646,17.1262462788252));
#77944=CARTESIAN_POINT('Ctrl Pts',(6.47922635886562,-2.69561356648885,17.1007900355964));
#77945=CARTESIAN_POINT('Ctrl Pts',(6.35861599103292,-2.96895849518786,17.0870977161311));
#77946=CARTESIAN_POINT('Ctrl Pts',(6.10772186199823,-3.45161258521224,17.0623701269612));
#77947=CARTESIAN_POINT('Ctrl Pts',(5.98312763001639,-3.66334308149199,17.0513079683639));
#77948=CARTESIAN_POINT('Ctrl Pts',(5.72079747825706,-4.059925913999,17.029968743167));
#77949=CARTESIAN_POINT('Ctrl Pts',(5.5845505269411,-4.24538774841203,17.0196980445586));
#77950=CARTESIAN_POINT('Ctrl Pts',(5.34369734822726,-4.54153596251342,17.0025518482901));
#77951=CARTESIAN_POINT('Ctrl Pts',(5.24416405093607,-4.65611351135732,16.9957123191847));
#77952=CARTESIAN_POINT('Ctrl Pts',(4.97250429443794,-4.94906326508929,16.9775308935524));
#77953=CARTESIAN_POINT('Ctrl Pts',(4.79450538407557,-5.12169328135939,16.9661202686862));
#77954=CARTESIAN_POINT('Ctrl Pts',(4.3754672734317,-5.4870651028578,16.9405405962388));
#77955=CARTESIAN_POINT('Ctrl Pts',(4.13008625304336,-5.67406298365945,16.9264118914367));
#77956=CARTESIAN_POINT('Ctrl Pts',(3.52843577889293,-6.07279443747314,16.8936350917234));
#77957=CARTESIAN_POINT('Ctrl Pts',(3.16413259506985,-6.27032385217807,16.8751827475865));
#77958=CARTESIAN_POINT('Ctrl Pts',(2.66319233617672,-6.48710393375469,16.8507083923684));
#77959=CARTESIAN_POINT('Ctrl Pts',(2.54037925818996,-6.53617499077462,16.8447697234657));
#77960=CARTESIAN_POINT('Ctrl Pts',(2.29498709661735,-6.62626200791968,16.832955593691));
#77961=CARTESIAN_POINT('Ctrl Pts',(2.17251663596854,-6.66741960960383,16.8270757708442));
#77962=CARTESIAN_POINT('Ctrl Pts',(1.7874059135473,-6.78510259665264,16.8086451312496));
#77963=CARTESIAN_POINT('Ctrl Pts',(1.5213784048371,-6.84966018891278,16.7960269483759));
#77964=CARTESIAN_POINT('Ctrl Pts',(1.05714718378318,-6.93393037632997,16.7743603600334));
#77965=CARTESIAN_POINT('Ctrl Pts',(0.860616104300867,-6.96105539785072,
16.7652915256496));
#77966=CARTESIAN_POINT('Ctrl Pts',(0.421103786264986,-7.00281635562354,
16.7452193779524));
#77967=CARTESIAN_POINT('Ctrl Pts',(0.177974285219394,-7.0132084955377,16.7342586441171));
#77968=CARTESIAN_POINT('Ctrl Pts',(-0.373439342799838,-7.00808003194474,
16.7095072797542));
#77969=CARTESIAN_POINT('Ctrl Pts',(-0.681145051399979,-6.98488944475263,
16.6957761549718));
#77970=CARTESIAN_POINT('Ctrl Pts',(-1.11188518927663,-6.92368562289141,
16.6761375206015));
#77971=CARTESIAN_POINT('Ctrl Pts',(-1.23693917084852,-6.90244100766074,
16.670376238896));
#77972=CARTESIAN_POINT('Ctrl Pts',(-1.63347048804642,-6.82395433360602,
16.6518977433815));
#77973=CARTESIAN_POINT('Ctrl Pts',(-1.90215610330906,-6.75398993883881,
16.6390996309057));
#77974=CARTESIAN_POINT('Ctrl Pts',(-2.40957541225703,-6.5891705065465,16.6145901415609));
#77975=CARTESIAN_POINT('Ctrl Pts',(-2.64864766505702,-6.49676003461844,
16.6028879703152));
#77976=CARTESIAN_POINT('Ctrl Pts',(-3.18090903097595,-6.25674558791332,
16.5764155993003));
#77977=CARTESIAN_POINT('Ctrl Pts',(-3.46987517683895,-6.10123086062648,
16.5617436376327));
#77978=CARTESIAN_POINT('Ctrl Pts',(-3.94323687007113,-5.80193640726703,
16.5366577967459));
#77979=CARTESIAN_POINT('Ctrl Pts',(-4.1332767915154,-5.66812163071558,16.5262578023159));
#77980=CARTESIAN_POINT('Ctrl Pts',(-4.58211232271473,-5.31748371384333,
16.5004089646846));
#77981=CARTESIAN_POINT('Ctrl Pts',(-4.83257114760226,-5.09093681140747,
16.4848332158554));
#77982=CARTESIAN_POINT('Ctrl Pts',(-5.24816949750473,-4.65660461718289,
16.4572069757215));
#77983=CARTESIAN_POINT('Ctrl Pts',(-5.41968614758737,-4.45581145880002,
16.445143873667));
#77984=CARTESIAN_POINT('Ctrl Pts',(-5.72638183929998,-4.0527799460245,16.4221745402546));
#77985=CARTESIAN_POINT('Ctrl Pts',(-5.86316847114925,-3.85223731052618,
16.4112674976456));
#77986=CARTESIAN_POINT('Ctrl Pts',(-6.13392524450991,-3.40734379154622,
16.3879183058445));
#77987=CARTESIAN_POINT('Ctrl Pts',(-6.26428803646808,-3.16128498604509,
16.3755084088207));
#77988=CARTESIAN_POINT('Ctrl Pts',(-6.4328345428192,-2.79153832645471,16.3571500982043));
#77989=CARTESIAN_POINT('Ctrl Pts',(-6.48277698657554,-2.67350854187538,
16.3513209450489));
#77990=CARTESIAN_POINT('Ctrl Pts',(-6.6324184378392,-2.29096768202361,16.3325272908703));
#77991=CARTESIAN_POINT('Ctrl Pts',(-6.71937052319194,-2.02177319322608,
16.3194861559102));
#77992=CARTESIAN_POINT('Ctrl Pts',(-6.85147135246525,-1.50866756857715,
16.2951586814586));
#77993=CARTESIAN_POINT('Ctrl Pts',(-6.90040199395209,-1.26617269724376,
16.2838722597639));
#77994=CARTESIAN_POINT('Ctrl Pts',(-6.98624916328889,-0.683289388699604,
16.2571717977581));
#77995=CARTESIAN_POINT('Ctrl Pts',(-7.01125858868385,-0.341787511429588,
16.2418817111034));
#77996=CARTESIAN_POINT('Ctrl Pts',(-7.01124466201124,0.212568646146331,
16.2170454330908));
#77997=CARTESIAN_POINT('Ctrl Pts',(-7.00158828261392,0.424848241481843,
16.2075242251945));
#77998=CARTESIAN_POINT('Ctrl Pts',(-6.96549144408797,0.820913657941926,
16.1894710556958));
#77999=CARTESIAN_POINT('Ctrl Pts',(-6.94136090725623,1.0047273438697,16.1809707123927));
#78000=CARTESIAN_POINT('Ctrl Pts',(-6.8404564236361,1.59194968198766,16.1535746267476));
#78001=CARTESIAN_POINT('Ctrl Pts',(-6.73553476393021,1.9896563466863,16.134698335654));
#78002=CARTESIAN_POINT('Ctrl Pts',(-6.58847844020422,2.39794234569235,16.1150125326801));
#78003=CARTESIAN_POINT('Ctrl Pts',(-6.58042797879554,2.4199469208126,16.1139504014194));
#78004=CARTESIAN_POINT('Ctrl Pts',(-6.57226800013471,2.44190906810743,16.1128890894906));
#78005=CARTESIAN_POINT('',(-7.0112499981366,-0.00016164628603672,16.7735343569104));
#78006=CARTESIAN_POINT('Ctrl Pts',(-6.57226799596304,2.44190907933527,16.660297082902));
#78007=CARTESIAN_POINT('Ctrl Pts',(-6.58514542129488,2.40725017614552,16.6619761778387));
#78008=CARTESIAN_POINT('Ctrl Pts',(-6.59774827257987,2.37249050223351,16.6636552727754));
#78009=CARTESIAN_POINT('Ctrl Pts',(-6.61007499971753,2.33763450107353,16.6653343677121));
#78010=CARTESIAN_POINT('Ctrl Pts',(-6.67265846254533,2.16066869104471,16.6738592238545));
#78011=CARTESIAN_POINT('Ctrl Pts',(-6.72814251569491,1.98115620202462,16.6823840799969));
#78012=CARTESIAN_POINT('Ctrl Pts',(-6.77633856351089,1.79968392646465,16.6909089361393));
#78013=CARTESIAN_POINT('Ctrl Pts',(-6.82452658430392,1.61824187500369,16.6994323724719));
#78014=CARTESIAN_POINT('Ctrl Pts',(-6.86542894192989,1.43484098467328,16.7079558088046));
#78015=CARTESIAN_POINT('Ctrl Pts',(-6.89890725570808,1.25008209315963,16.7164792451373));
#78016=CARTESIAN_POINT('Ctrl Pts',(-6.93238090759436,1.0653489295243,16.7250014945722));
#78017=CARTESIAN_POINT('Ctrl Pts',(-6.95843252528074,0.879258444382991,
16.733523744007));
#78018=CARTESIAN_POINT('Ctrl Pts',(-6.97697497069008,0.69242098528582,16.7420459934418));
#78019=CARTESIAN_POINT('Ctrl Pts',(-6.99551756399199,0.505582035992998,
16.7505683108492));
#78020=CARTESIAN_POINT('Ctrl Pts',(-7.00655083429286,0.317996406289197,
16.7590906282566));
#78021=CARTESIAN_POINT('Ctrl Pts',(-7.01003949854652,0.130279665787652,
16.767612945664));
#78022=CARTESIAN_POINT('Ctrl Pts',(-7.01084748753039,0.0868036969395056,
16.7695867494128));
#78023=CARTESIAN_POINT('Ctrl Pts',(-7.01125100063413,0.0433207061692093,
16.7715605531616));
#78024=CARTESIAN_POINT('Ctrl Pts',(-7.0112499981366,-0.00016164628603672,
16.7735343569104));
#78025=CARTESIAN_POINT('Ctrl Pts',(-6.57226799068689,2.44190909353574,18.6606197598975));
#78026=CARTESIAN_POINT('Ctrl Pts',(-6.55458256276715,2.4895084788389,18.6583252162124));
#78027=CARTESIAN_POINT('Ctrl Pts',(-6.53637908263129,2.53691828524661,18.6560271977506));
#78028=CARTESIAN_POINT('Ctrl Pts',(-6.34950578661924,3.00824777710428,18.6330474945965));
#78029=CARTESIAN_POINT('Ctrl Pts',(-6.14035688537109,3.41493452497112,18.6120463439572));
#78030=CARTESIAN_POINT('Ctrl Pts',(-5.80529356625243,3.93478342108527,18.583636287599));
#78031=CARTESIAN_POINT('Ctrl Pts',(-5.71267994946519,4.06807616298501,18.576207268064));
#78032=CARTESIAN_POINT('Ctrl Pts',(-5.48133729766782,4.3775326923495,18.5586842567907));
#78033=CARTESIAN_POINT('Ctrl Pts',(-5.33861997283839,4.55049345230517,18.5486484067481));
#78034=CARTESIAN_POINT('Ctrl Pts',(-5.03271150353628,4.88698673714595,18.5282781650059));
#78035=CARTESIAN_POINT('Ctrl Pts',(-4.86923449019688,5.04988898793645,18.5179552406326));
#78036=CARTESIAN_POINT('Ctrl Pts',(-4.62367611942892,5.27155371416962,18.5030418091212));
#78037=CARTESIAN_POINT('Ctrl Pts',(-4.54789521056789,5.3370692648912,18.4985146599895));
#78038=CARTESIAN_POINT('Ctrl Pts',(-4.13498086892453,5.67886755600364,18.4742101598731));
#78039=CARTESIAN_POINT('Ctrl Pts',(-3.77404342110726,5.92487840940232,18.4541564401886));
#78040=CARTESIAN_POINT('Ctrl Pts',(-3.242360167737,6.21885906131579,18.4262355797459));
#78041=CARTESIAN_POINT('Ctrl Pts',(-3.08909591832835,6.29639546514875,18.4183677192841));
#78042=CARTESIAN_POINT('Ctrl Pts',(-2.77205432161874,6.44242143264674,18.4025303922832));
#78043=CARTESIAN_POINT('Ctrl Pts',(-2.60821163962649,6.51047715200553,18.3945656421109));
#78044=CARTESIAN_POINT('Ctrl Pts',(-2.06320144224783,6.7129793869552,18.3685009461884));
#78045=CARTESIAN_POINT('Ctrl Pts',(-1.67298773499486,6.82070373535555,18.3504665571867));
#78046=CARTESIAN_POINT('Ctrl Pts',(-1.08158271529183,6.93013475092709,18.3231586639686));
#78047=CARTESIAN_POINT('Ctrl Pts',(-0.886061138421088,6.95783606780917,
18.314143806508));
#78048=CARTESIAN_POINT('Ctrl Pts',(-0.425571818255266,7.00335100387356,
18.2929120378822));
#78049=CARTESIAN_POINT('Ctrl Pts',(-0.160241699369519,7.01443930242023,
18.2806741832081));
#78050=CARTESIAN_POINT('Ctrl Pts',(0.245827482243395,7.00835292333669,18.2620503839529));
#78051=CARTESIAN_POINT('Ctrl Pts',(0.386485679439094,7.00200487711029,18.2556228942669));
#78052=CARTESIAN_POINT('Ctrl Pts',(0.586026920853302,6.98696783929156,18.2465618493075));
#78053=CARTESIAN_POINT('Ctrl Pts',(0.645134947704559,6.9817582393844,18.2438834074806));
#78054=CARTESIAN_POINT('Ctrl Pts',(0.880753138408596,6.95797382925482,18.2332156076782));
#78055=CARTESIAN_POINT('Ctrl Pts',(1.05659691472483,6.93345005546821,18.2252730372193));
#78056=CARTESIAN_POINT('Ctrl Pts',(1.52729742197193,6.84948019116534,18.2038567245137));
#78057=CARTESIAN_POINT('Ctrl Pts',(1.81956694668522,6.77769789226068,18.1903810293141));
#78058=CARTESIAN_POINT('Ctrl Pts',(2.3485594573209,6.61108125147755,18.1652379015473));
#78059=CARTESIAN_POINT('Ctrl Pts',(2.58646861352615,6.52167948143408,18.15363616957));
#78060=CARTESIAN_POINT('Ctrl Pts',(3.07192843455,6.30850155802817,18.1292817568975));
#78061=CARTESIAN_POINT('Ctrl Pts',(3.31807333418695,6.18258247536715,18.1165372275004));
#78062=CARTESIAN_POINT('Ctrl Pts',(3.66578414484173,5.97794588678848,18.0980866228301));
#78063=CARTESIAN_POINT('Ctrl Pts',(3.77364609060732,5.91044893355489,18.0923037700712));
#78064=CARTESIAN_POINT('Ctrl Pts',(4.13696044959863,5.66909503045029,18.0726073341635));
#78065=CARTESIAN_POINT('Ctrl Pts',(4.38272739932649,5.48131230138458,18.0588444751542));
#78066=CARTESIAN_POINT('Ctrl Pts',(4.79977390069267,5.11662435263432,18.0339809489723));
#78067=CARTESIAN_POINT('Ctrl Pts',(4.97565379040086,4.9457598651466,18.0229388622396));
#78068=CARTESIAN_POINT('Ctrl Pts',(5.34582704617447,4.54636883134513,17.9981839042158));
#78069=CARTESIAN_POINT('Ctrl Pts',(5.53514067636744,4.31387863218984,17.9844428078976));
#78070=CARTESIAN_POINT('Ctrl Pts',(5.85572995542538,3.86418701494117,17.9590315263988));
#78071=CARTESIAN_POINT('Ctrl Pts',(5.99122114808128,3.65058713423913,17.9473952100159));
#78072=CARTESIAN_POINT('Ctrl Pts',(6.20573847891588,3.26816843022517,17.9274715867082));
#78073=CARTESIAN_POINT('Ctrl Pts',(6.29012433195544,3.10265249767159,17.919128472505));
#78074=CARTESIAN_POINT('Ctrl Pts',(6.53934905997762,2.56174114659309,17.8924263265319));
#78075=CARTESIAN_POINT('Ctrl Pts',(6.67788656577902,2.17518501476121,17.8741384016438));
#78076=CARTESIAN_POINT('Ctrl Pts',(6.80724963445372,1.6819606212768,17.8509845146513));
#78077=CARTESIAN_POINT('Ctrl Pts',(6.83056039668648,1.58463987738861,17.8464274245965));
#78078=CARTESIAN_POINT('Ctrl Pts',(6.87605250695625,1.37500134497382,17.8366293681007));
#78079=CARTESIAN_POINT('Ctrl Pts',(6.89758215531807,1.26257154065238,17.8313857131571));
#78080=CARTESIAN_POINT('Ctrl Pts',(6.96096076284132,0.881288036443326,17.813638932025));
#78081=CARTESIAN_POINT('Ctrl Pts',(6.98991291079394,0.610541472833123,17.8010883076366));
#78082=CARTESIAN_POINT('Ctrl Pts',(7.00937466701543,0.208262084983773,17.7826476501432));
#78083=CARTESIAN_POINT('Ctrl Pts',(7.01203894166487,0.0775724229597804,
17.7766950933235));
#78084=CARTESIAN_POINT('Ctrl Pts',(7.01007379652506,-0.18180591059101,17.7649676521403));
#78085=CARTESIAN_POINT('Ctrl Pts',(7.0055558984855,-0.310443448558691,17.7591853188952));
#78086=CARTESIAN_POINT('Ctrl Pts',(6.97092465084892,-0.862598097317044,
17.7343729716898));
#78087=CARTESIAN_POINT('Ctrl Pts',(6.90591976661297,-1.28301726522208,17.7154419265826));
#78088=CARTESIAN_POINT('Ctrl Pts',(6.72904978721014,-1.99294172322638,17.6822117280348));
#78089=CARTESIAN_POINT('Ctrl Pts',(6.63531696194163,-2.28571449999727,17.6681312389614));
#78090=CARTESIAN_POINT('Ctrl Pts',(6.42669735932324,-2.81490724271353,17.6419589531438));
#78091=CARTESIAN_POINT('Ctrl Pts',(6.31713590902911,-3.05285743066206,17.6299049845625));
#78092=CARTESIAN_POINT('Ctrl Pts',(6.10246935669569,-3.45776205930725,17.6090865492287));
#78093=CARTESIAN_POINT('Ctrl Pts',(6.00315165776121,-3.62745406270624,17.6002645423005));
#78094=CARTESIAN_POINT('Ctrl Pts',(5.68456426588421,-4.12278248941258,17.5738682960467));
#78095=CARTESIAN_POINT('Ctrl Pts',(5.44496429707679,-4.43440695890372,17.5563448717549));
#78096=CARTESIAN_POINT('Ctrl Pts',(4.96219934494556,-4.963790794616,17.5238205337869));
#78097=CARTESIAN_POINT('Ctrl Pts',(4.7275055404023,-5.18780550218222,17.5089601753391));
#78098=CARTESIAN_POINT('Ctrl Pts',(4.28541895943661,-5.5547783297998,17.4825233881553));
#78099=CARTESIAN_POINT('Ctrl Pts',(4.08423258697901,-5.70433385709519,17.4709919160538));
#78100=CARTESIAN_POINT('Ctrl Pts',(3.72264300981196,-5.94417265756288,17.4512749069998));
#78101=CARTESIAN_POINT('Ctrl Pts',(3.5658926489595,-6.03950914948238,17.4430343854042));
#78102=CARTESIAN_POINT('Ctrl Pts',(3.04382720564884,-6.32961457142564,17.4162542512617));
#78103=CARTESIAN_POINT('Ctrl Pts',(2.66498689040986,-6.49821087624218,17.3977908826496));
#78104=CARTESIAN_POINT('Ctrl Pts',(2.17883809683168,-6.66485590964755,17.3744533230881));
#78105=CARTESIAN_POINT('Ctrl Pts',(2.08349590294417,-6.69527328252417,17.369895785479));
#78106=CARTESIAN_POINT('Ctrl Pts',(1.76114285095497,-6.79056219558045,17.3545416326272));
#78107=CARTESIAN_POINT('Ctrl Pts',(1.53151605379391,-6.84600727960147,17.3436894004361));
#78108=CARTESIAN_POINT('Ctrl Pts',(1.07736912722764,-6.93166756745294,17.3224239485234));
#78109=CARTESIAN_POINT('Ctrl Pts',(0.853305623856332,-6.96280195982973,
17.3120247101515));
#78110=CARTESIAN_POINT('Ctrl Pts',(0.465224142115352,-6.99771002274748,
17.294304996123));
#78111=CARTESIAN_POINT('Ctrl Pts',(0.301855577424184,-7.00665849027971,
17.2869423355451));
#78112=CARTESIAN_POINT('Ctrl Pts',(-0.31487034555525,-7.01882804343387,
17.2592578592243));
#78113=CARTESIAN_POINT('Ctrl Pts',(-0.767857977525109,-6.98380127946097,
17.239071530554));
#78114=CARTESIAN_POINT('Ctrl Pts',(-1.31309911089605,-6.88792156656363,
17.2139122766892));
#78115=CARTESIAN_POINT('Ctrl Pts',(-1.41152849570265,-6.86842630052985,
17.2093391709666));
#78116=CARTESIAN_POINT('Ctrl Pts',(-1.73908280158202,-6.79621110509029,
17.1940072918837));
#78117=CARTESIAN_POINT('Ctrl Pts',(-1.96596790703423,-6.73408217683143,
17.1831951785447));
#78118=CARTESIAN_POINT('Ctrl Pts',(-2.387998090881,-6.59536487749762,17.1627549784192));
#78119=CARTESIAN_POINT('Ctrl Pts',(-2.58367594814301,-6.52119568161628,
17.1531392145756));
#78120=CARTESIAN_POINT('Ctrl Pts',(-2.91723454841433,-6.37739044629956,
17.1366116831451));
#78121=CARTESIAN_POINT('Ctrl Pts',(-3.05667272893022,-6.31174451470895,
17.1296685981729));
#78122=CARTESIAN_POINT('Ctrl Pts',(-3.60576021747791,-6.03077357350732,
17.1019685257737));
#78123=CARTESIAN_POINT('Ctrl Pts',(-3.99580179444336,-5.77973197456279,
17.081381589345));
#78124=CARTESIAN_POINT('Ctrl Pts',(-4.4367312836426,-5.42983216305697,17.0558080495292));
#78125=CARTESIAN_POINT('Ctrl Pts',(-4.5138578123915,-5.36588755094415,17.0512433669858));
#78126=CARTESIAN_POINT('Ctrl Pts',(-4.76446179643785,-5.14888736696189,
17.0360949011651));
#78127=CARTESIAN_POINT('Ctrl Pts',(-4.93173378149902,-4.9889014263526,17.0254592928678));
#78128=CARTESIAN_POINT('Ctrl Pts',(-5.24325703051603,-4.65994099330217,
17.0046125870816));
#78129=CARTESIAN_POINT('Ctrl Pts',(-5.38800240598723,-4.49179545947177,
16.9944144973066));
#78130=CARTESIAN_POINT('Ctrl Pts',(-5.6235730215545,-4.19033686984055,16.977013590253));
#78131=CARTESIAN_POINT('Ctrl Pts',(-5.71821836225299,-4.06023105500928,
16.9697713622525));
#78132=CARTESIAN_POINT('Ctrl Pts',(-5.98889905027684,-3.65987374037618,
16.9480780493933));
#78133=CARTESIAN_POINT('Ctrl Pts',(-6.15084999122691,-3.38062591369407,
16.9337020803631));
#78134=CARTESIAN_POINT('Ctrl Pts',(-6.38719282423073,-2.89948773449133,
16.9095315441764));
#78135=CARTESIAN_POINT('Ctrl Pts',(-6.47256455400576,-2.70354712639233,
16.8998455551178));
#78136=CARTESIAN_POINT('Ctrl Pts',(-6.6779079742761,-2.16650438430513,16.8735948063815));
#78137=CARTESIAN_POINT('Ctrl Pts',(-6.78067367814398,-1.81952062373872,
16.8569220515564));
#78138=CARTESIAN_POINT('Ctrl Pts',(-6.88455722143499,-1.33373202292574,
16.8341322263777));
#78139=CARTESIAN_POINT('Ctrl Pts',(-6.90903608853085,-1.20049609308365,
16.8279420002742));
#78140=CARTESIAN_POINT('Ctrl Pts',(-6.98395896766335,-0.71374121309055,
16.8056121326512));
#78141=CARTESIAN_POINT('Ctrl Pts',(-7.01124216365981,-0.35721143636207,
16.7897364775856));
#78142=CARTESIAN_POINT('Ctrl Pts',(-7.01124999831217,-0.000153842705974752,
16.7737082138839));
#78143=CARTESIAN_POINT('Origin',(0.,0.,24.4167025567876));
#78144=CARTESIAN_POINT('',(-8.12490033498142,-0.000187321799185458,17.4167025567876));
#78145=CARTESIAN_POINT('Ctrl Pts',(4.94687992157187,6.44602802604219,18.7083406766545));
#78146=CARTESIAN_POINT('Ctrl Pts',(5.82016762916966,5.77439204688032,18.6651775777328));
#78147=CARTESIAN_POINT('Ctrl Pts',(7.46076195865801,3.88189356139278,18.5690832782987));
#78148=CARTESIAN_POINT('Ctrl Pts',(8.46957003418644,0.089278768870349,18.420057778352));
#78149=CARTESIAN_POINT('Ctrl Pts',(7.480065253005,-3.97368988069115,18.2612641768145));
#78150=CARTESIAN_POINT('Ctrl Pts',(4.66731299336978,-7.0680815798286,18.1024705752769));
#78151=CARTESIAN_POINT('Ctrl Pts',(0.716914735007744,-8.43964576898856,
17.9436769737395));
#78152=CARTESIAN_POINT('Ctrl Pts',(-3.40822973045652,-7.75406717637959,
17.7848833722019));
#78153=CARTESIAN_POINT('Ctrl Pts',(-6.70262660827141,-5.17845383384662,
17.6260897706644));
#78154=CARTESIAN_POINT('Ctrl Pts',(-7.98609311183373,-2.21229264724039,
17.503362832193));
#78155=CARTESIAN_POINT('Ctrl Pts',(-8.12526575298013,-0.430719974176783,
17.433567094234));
#78156=CARTESIAN_POINT('Ctrl Pts',(-8.12490033498142,-0.000187321799185458,
17.4167025567876));
#78157=CARTESIAN_POINT('Ctrl Pts',(-8.12490033498142,-0.000187321799185458,
17.4167025567876));
#78158=CARTESIAN_POINT('Ctrl Pts',(-8.12411884851139,0.920553977010579,
17.3806358937215));
#78159=CARTESIAN_POINT('Ctrl Pts',(-7.73854515129239,3.1932071511791,17.2916380301429));
#78160=CARTESIAN_POINT('Ctrl Pts',(-5.66109559838795,6.30028445507239,17.1497089660519));
#78161=CARTESIAN_POINT('Ctrl Pts',(-1.95691771365938,8.24087742028646,16.9909153645144));
#78162=CARTESIAN_POINT('Ctrl Pts',(1.91681060280639,8.17778432394259,16.8437979275536));
#78163=CARTESIAN_POINT('Ctrl Pts',(4.11071045687717,7.08613171679798,16.7496116911053));
#78164=CARTESIAN_POINT('Ctrl Pts',(4.94678612080823,6.44590587665303,16.7083566551695));
#78165=CARTESIAN_POINT('',(-8.12524999730276,-0.00020935965107711,17.5832974432124));
#78166=CARTESIAN_POINT('Ctrl Pts',(-8.12524999730276,-0.00020935965107711,
17.5832974432124));
#78167=CARTESIAN_POINT('Ctrl Pts',(-8.12525538426066,0.208858526346167,
17.5751067683804));
#78168=CARTESIAN_POINT('Ctrl Pts',(-8.11718725248735,0.417953074078032,
17.5669160935484));
#78169=CARTESIAN_POINT('Ctrl Pts',(-8.10106550486504,0.626438543183453,
17.5587254187164));
#78170=CARTESIAN_POINT('Ctrl Pts',(-8.08475759734551,0.837331420865582,
17.5504401651067));
#78171=CARTESIAN_POINT('Ctrl Pts',(-8.06020892462738,1.04760075430505,17.5421549114969));
#78172=CARTESIAN_POINT('Ctrl Pts',(-8.0274942255562,1.25659222549,17.5338696578872));
#78173=CARTESIAN_POINT('Ctrl Pts',(-7.99515416061828,1.46319041961937,17.5256792833041));
#78174=CARTESIAN_POINT('Ctrl Pts',(-7.95483417279298,1.66853956545462,17.5174889087211));
#78175=CARTESIAN_POINT('Ctrl Pts',(-7.90665826764153,1.87201565197404,17.509298534138));
#78176=CARTESIAN_POINT('Ctrl Pts',(-7.8576452427206,2.07902740334725,17.5009658410149));
#78177=CARTESIAN_POINT('Ctrl Pts',(-7.80050083925289,2.28410008993034,17.4926331478919));
#78178=CARTESIAN_POINT('Ctrl Pts',(-7.73540939159931,2.48658985497351,17.4843004547688));
#78179=CARTESIAN_POINT('Ctrl Pts',(-7.67031794394573,2.68907962001667,17.4759677616458));
#78180=CARTESIAN_POINT('Ctrl Pts',(-7.5972795603539,2.88898615586395,17.4676350685228));
#78181=CARTESIAN_POINT('Ctrl Pts',(-7.51653138681063,3.08568363148113,17.4593023753997));
#78182=CARTESIAN_POINT('Ctrl Pts',(-7.43685433004201,3.27977193395646,17.4510802146515));
#78183=CARTESIAN_POINT('Ctrl Pts',(-7.34964262325963,3.47080453946901,17.4428580539032));
#78184=CARTESIAN_POINT('Ctrl Pts',(-7.25515605850115,3.65819602116865,17.434635893155));
#78185=CARTESIAN_POINT('Ctrl Pts',(-7.16068691028673,3.84555296132253,17.4264152479833));
#78186=CARTESIAN_POINT('Ctrl Pts',(-7.05894571328507,4.02926985380545,17.4181946028116));
#78187=CARTESIAN_POINT('Ctrl Pts',(-6.95023901936932,4.20878428244264,17.4099739576399));
#78188=CARTESIAN_POINT('Ctrl Pts',(-6.84154453784167,4.38827854396967,17.4017542359966));
#78189=CARTESIAN_POINT('Ctrl Pts',(-6.72588627446995,4.56357103183399,17.3935345143532));
#78190=CARTESIAN_POINT('Ctrl Pts',(-6.60361549295675,4.73412610559558,17.3853147927099));
#78191=CARTESIAN_POINT('Ctrl Pts',(-6.48133491430855,4.90469484534557,17.3770944124486));
#78192=CARTESIAN_POINT('Ctrl Pts',(-6.3524409285994,5.07052517105891,17.3688740321874));
#78193=CARTESIAN_POINT('Ctrl Pts',(-6.21732730281701,5.23111161916338,17.3606536519262));
#78194=CARTESIAN_POINT('Ctrl Pts',(-6.08221417704902,5.39169747298629,17.352433302086));
#78195=CARTESIAN_POINT('Ctrl Pts',(-5.94088164930919,5.54703926389823,17.3442129522459));
#78196=CARTESIAN_POINT('Ctrl Pts',(-5.79376317510849,5.69666532571967,17.3359926024058));
#78197=CARTESIAN_POINT('Ctrl Pts',(-5.64661324509857,5.84632337950459,17.3277704949499));
#78198=CARTESIAN_POINT('Ctrl Pts',(-5.49367510409307,5.99026305219196,17.319548387494));
#78199=CARTESIAN_POINT('Ctrl Pts',(-5.33541918058525,6.12804942293574,17.3113262800381));
#78200=CARTESIAN_POINT('Ctrl Pts',(-5.26601546468522,6.1884761413677,17.3077204446461));
#78201=CARTESIAN_POINT('Ctrl Pts',(-5.19558943929163,6.24771989754552,17.3041146092542));
#78202=CARTESIAN_POINT('Ctrl Pts',(-5.12418284498617,6.30574640575162,17.3005087738622));
#78203=CARTESIAN_POINT('Ctrl Pts',(-4.96135887548661,6.43806060578053,17.292286614024));
#78204=CARTESIAN_POINT('Ctrl Pts',(-4.79338046715548,6.56408672460702,17.2840644541859));
#78205=CARTESIAN_POINT('Ctrl Pts',(-4.6207558352372,6.68343497564099,17.2758422943477));
#78206=CARTESIAN_POINT('Ctrl Pts',(-4.44816302311957,6.80276122727944,17.2676216500956));
#78207=CARTESIAN_POINT('Ctrl Pts',(-4.27092593939041,6.91541190012624,17.2594010058435));
#78208=CARTESIAN_POINT('Ctrl Pts',(-4.08958285136217,7.02103978512759,17.2511803615913));
#78209=CARTESIAN_POINT('Ctrl Pts',(-3.90826013602747,7.12665580353643,17.2429606408741));
#78210=CARTESIAN_POINT('Ctrl Pts',(-3.7228325922447,7.2252504607178,17.2347409201569));
#78211=CARTESIAN_POINT('Ctrl Pts',(-3.53386493967195,7.31652145152718,17.2265211994396));
#78212=CARTESIAN_POINT('Ctrl Pts',(-3.34488214583468,7.40779975553644,17.2183008201072));
#78213=CARTESIAN_POINT('Ctrl Pts',(-3.15235894102377,7.49175308982551,17.2100804407748));
#78214=CARTESIAN_POINT('Ctrl Pts',(-2.95688293066066,7.56812598315248,17.2018600614424));
#78215=CARTESIAN_POINT('Ctrl Pts',(-2.761407643692,7.64449859384769,17.193639712531));
#78216=CARTESIAN_POINT('Ctrl Pts',(-2.56297984890816,7.7132907147765,17.1854193636196));
#78217=CARTESIAN_POINT('Ctrl Pts',(-2.36220583361238,7.7742955412145,17.1771990147081));
#78218=CARTESIAN_POINT('Ctrl Pts',(-2.16138889010998,7.83531341131151,17.1689769081747));
#78219=CARTESIAN_POINT('Ctrl Pts',(-1.95822500634198,7.88854057469016,17.1607548016412));
#78220=CARTESIAN_POINT('Ctrl Pts',(-1.75333535652475,7.93382018261444,17.1525326951077));
#78221=CARTESIAN_POINT('Ctrl Pts',(-1.66348010082346,7.95367775351526,17.1489268541801));
#78222=CARTESIAN_POINT('Ctrl Pts',(-1.57329309072578,7.97200742702453,17.1453210132524));
#78223=CARTESIAN_POINT('Ctrl Pts',(-1.48282738326448,7.9887990658134,17.1417151723247));
#78224=CARTESIAN_POINT('Ctrl Pts',(-1.27654442924292,8.02708792630468,17.1334930123575));
#78225=CARTESIAN_POINT('Ctrl Pts',(-1.06874362769325,8.05738902441135,17.1252708523903));
#78226=CARTESIAN_POINT('Ctrl Pts',(-0.860057740986279,8.07960322322016,
17.1170486924231));
#78227=CARTESIAN_POINT('Ctrl Pts',(-0.651410321219439,8.10181332729947,
17.1088280480416));
#78228=CARTESIAN_POINT('Ctrl Pts',(-0.441878435251749,8.11593947599364,
17.10060740366));
#78229=CARTESIAN_POINT('Ctrl Pts',(-0.232100864634496,8.12193429862221,
17.0923867592785));
#78230=CARTESIAN_POINT('Ctrl Pts',(-0.0223468611301164,8.1279284477724,
17.0841670384316));
#78231=CARTESIAN_POINT('Ctrl Pts',(0.18765247701369,8.12579308616848,17.0759473175847));
#78232=CARTESIAN_POINT('Ctrl Pts',(0.39725662308003,8.11553293000029,17.0677275967378));
#78233=CARTESIAN_POINT('Ctrl Pts',(0.606877563909257,8.10527195172579,17.0595072172767));
#78234=CARTESIAN_POINT('Ctrl Pts',(0.816102954456935,8.08688488981133,17.0512868378156));
#78235=CARTESIAN_POINT('Ctrl Pts',(1.02429457811477,8.06042853573832,17.0430664583545));
#78236=CARTESIAN_POINT('Ctrl Pts',(1.2324854313022,8.03397227957434,17.0348461093152));
#78237=CARTESIAN_POINT('Ctrl Pts',(1.43964223279993,7.99944683084303,17.0266257602759));
#78238=CARTESIAN_POINT('Ctrl Pts',(1.64513364442268,7.95696065432578,17.0184054112366));
#78239=CARTESIAN_POINT('Ctrl Pts',(1.850668992846,7.91446539369815,17.0101833045772));
#78240=CARTESIAN_POINT('Ctrl Pts',(2.05453795092107,7.86400606457075,17.0019611979178));
#78241=CARTESIAN_POINT('Ctrl Pts',(2.25612000826752,7.80574212172007,16.9937390912584));
#78242=CARTESIAN_POINT('Ctrl Pts',(2.34452468451809,7.78019021956866,16.9901332511013));
#78243=CARTESIAN_POINT('Ctrl Pts',(2.43248969275652,7.75313791034859,16.9865274109443));
#78244=CARTESIAN_POINT('Ctrl Pts',(2.51996359225185,7.72460167621769,16.9829215707872));
#78245=CARTESIAN_POINT('Ctrl Pts',(2.71942272518129,7.65953298087359,16.9746994867672));
#78246=CARTESIAN_POINT('Ctrl Pts',(2.91639318855617,7.58672398261398,16.9664774027471));
#78247=CARTESIAN_POINT('Ctrl Pts',(3.11027192380636,7.50639035239188,16.9582553187271));
#78248=CARTESIAN_POINT('Ctrl Pts',(3.30412189462654,7.42606864070784,16.9500344545601));
#78249=CARTESIAN_POINT('Ctrl Pts',(3.49488077973406,7.33822463680505,16.9418135903931));
#78250=CARTESIAN_POINT('Ctrl Pts',(3.68196493807873,7.24312237624485,16.9335927262261));
#78251=CARTESIAN_POINT('Ctrl Pts',(3.86902427864327,7.14803273154168,16.9253729526036));
#78252=CARTESIAN_POINT('Ctrl Pts',(4.05240960296455,7.04568688678982,16.9171531789811));
#78253=CARTESIAN_POINT('Ctrl Pts',(4.23156069383441,6.93639543688908,16.9089334053586));
#78254=CARTESIAN_POINT('Ctrl Pts',(4.41071458111957,6.82710228103009,16.9007135034315));
#78255=CARTESIAN_POINT('Ctrl Pts',(4.58563385038789,6.71086345612257,16.8924936015045));
#78256=CARTESIAN_POINT('Ctrl Pts',(4.75578533036544,6.58803411147672,16.8842736995774));
#78257=CARTESIAN_POINT('Ctrl Pts',(4.82013425799734,6.54158175848671,16.8811650467798));
#78258=CARTESIAN_POINT('Ctrl Pts',(4.88380156985135,6.49418724095744,16.8780563939822));
#78259=CARTESIAN_POINT('Ctrl Pts',(4.94675954817621,6.44587135576157,16.8749477411846));
#78260=CARTESIAN_POINT('Ctrl Pts',(4.94710325578446,6.44631862759455,18.8749389137103));
#78261=CARTESIAN_POINT('Ctrl Pts',(5.92706477576575,5.69317017844722,18.8265096717068));
#78262=CARTESIAN_POINT('Ctrl Pts',(7.61516726084699,3.64267874792156,18.7251492291908));
#78263=CARTESIAN_POINT('Ctrl Pts',(8.46357381179856,-0.330935089626715,
18.5708575861624));
#78264=CARTESIAN_POINT('Ctrl Pts',(7.27375726455099,-4.33981891403078,18.4120639846248));
#78265=CARTESIAN_POINT('Ctrl Pts',(4.31098181048916,-7.29088689580246,18.2532703830874));
#78266=CARTESIAN_POINT('Ctrl Pts',(0.297414436183603,-8.46481700753604,
18.0944767815498));
#78267=CARTESIAN_POINT('Ctrl Pts',(-3.78864659254454,-7.57546998599963,
17.9356831800123));
#78268=CARTESIAN_POINT('Ctrl Pts',(-6.95123456136923,-4.83962029144108,
17.7768895784748));
#78269=CARTESIAN_POINT('Ctrl Pts',(-8.03731400816114,-1.94327236285129,
17.6594276662081));
#78270=CARTESIAN_POINT('Ctrl Pts',(-8.12560543629606,-0.296289995508007,
17.594896954454));
#78271=CARTESIAN_POINT('Ctrl Pts',(-8.12529972492543,-0.000209360932384682,
17.5832974432124));
#78272=CARTESIAN_POINT('Origin',(-15.,0.,10.));
#78273=CARTESIAN_POINT('',(-18.5,4.28626379701574E-16,20.));
#78274=CARTESIAN_POINT('Origin',(-15.,0.,20.));
#78275=CARTESIAN_POINT('',(-18.5,4.28626379701574E-16,0.));
#78276=CARTESIAN_POINT('',(-18.5,4.28626379701574E-16,10.));
#78277=CARTESIAN_POINT('Origin',(-15.,0.,0.));
#78278=CARTESIAN_POINT('Origin',(15.,0.,10.));
#78279=CARTESIAN_POINT('',(11.5,4.28626379701574E-16,20.));
#78280=CARTESIAN_POINT('Origin',(15.,0.,20.));
#78281=CARTESIAN_POINT('',(11.5,4.28626379701574E-16,0.));
#78282=CARTESIAN_POINT('',(11.5,4.28626379701574E-16,10.));
#78283=CARTESIAN_POINT('Origin',(15.,0.,0.));
#78284=CARTESIAN_POINT('Ctrl Pts',(5.309423840314,4.57791301092332,19.9996006767769));
#78285=CARTESIAN_POINT('Ctrl Pts',(6.07080882312251,3.6948682496547,19.9466604262186));
#78286=CARTESIAN_POINT('Ctrl Pts',(7.14359879543109,1.54261656134898,19.8407889751478));
#78287=CARTESIAN_POINT('Ctrl Pts',(7.01054163748306,-2.06378246543655,19.6819863235645));
#78288=CARTESIAN_POINT('Ctrl Pts',(5.16894015188214,-5.16605670552577,19.523192722027));
#78289=CARTESIAN_POINT('Ctrl Pts',(2.06730382912507,-7.00954776020371,19.3643991204894));
#78290=CARTESIAN_POINT('Ctrl Pts',(-1.53817327458349,-7.1442614489232,19.2056055189519));
#78291=CARTESIAN_POINT('Ctrl Pts',(-4.7687545802584,-5.53768944867667,19.0468119174144));
#78292=CARTESIAN_POINT('Ctrl Pts',(-6.83694841393584,-2.58126320243491,
18.8880183158769));
#78293=CARTESIAN_POINT('Ctrl Pts',(-7.23866073718961,1.00431105009051,18.7292247143393));
#78294=CARTESIAN_POINT('Ctrl Pts',(-5.87596341879415,4.34510146585654,18.5704311128019));
#78295=CARTESIAN_POINT('Ctrl Pts',(-3.08101653625123,6.62677675416298,18.4116375112643));
#78296=CARTESIAN_POINT('Ctrl Pts',(0.464921543395092,7.2931953172938,18.2528439097268));
#78297=CARTESIAN_POINT('Ctrl Pts',(3.89753562459927,6.18191362226655,18.0940503081893));
#78298=CARTESIAN_POINT('Ctrl Pts',(6.38013528416437,3.56380671277158,17.9352567066518));
#78299=CARTESIAN_POINT('Ctrl Pts',(7.30759258545994,0.077030223116708,17.7764631051143));
#78300=CARTESIAN_POINT('Ctrl Pts',(6.45384230379842,-3.42852194289047,17.6176695035767));
#78301=CARTESIAN_POINT('Ctrl Pts',(4.02698385947594,-6.09838047713161,17.4588759020392));
#78302=CARTESIAN_POINT('Ctrl Pts',(0.618558059122632,-7.2817737614107,17.3000823005017));
#78303=CARTESIAN_POINT('Ctrl Pts',(-2.9406397499871,-6.69025270191448,17.1412886989642));
#78304=CARTESIAN_POINT('Ctrl Pts',(-5.78306387549879,-4.46799904689602,
16.9824950974267));
#78305=CARTESIAN_POINT('Ctrl Pts',(-7.21588046124865,-1.15668166355883,
16.8237014958892));
#78306=CARTESIAN_POINT('Ctrl Pts',(-6.88984399838259,2.4365740239086,16.6649078943516));
#78307=CARTESIAN_POINT('Ctrl Pts',(-4.88442507156545,5.43592080640939,16.5061142928141));
#78308=CARTESIAN_POINT('Ctrl Pts',(-1.68843959220725,7.11027531398814,16.3473206912766));
#78309=CARTESIAN_POINT('Ctrl Pts',(1.91909886907681,7.05151776748327,16.1885270897391));
#78310=CARTESIAN_POINT('Ctrl Pts',(5.05886171908715,5.27397017464772,16.0297334882016));
#78311=CARTESIAN_POINT('Ctrl Pts',(6.96553951464736,2.21090537228499,15.8709398866641));
#78312=CARTESIAN_POINT('Ctrl Pts',(7.17438425046917,-1.39106215608347,15.7121462851265));
#78313=CARTESIAN_POINT('Ctrl Pts',(5.63449053777354,-4.65396171828115,15.553352683589));
#78314=CARTESIAN_POINT('Ctrl Pts',(2.72120366726484,-6.78246960160486,15.3945590820515));
#78315=CARTESIAN_POINT('Ctrl Pts',(-0.855369878873554,-7.25776726450987,
15.235765480514));
#78316=CARTESIAN_POINT('Ctrl Pts',(-4.22344912882297,-5.9640020750913,15.0769718789765));
#78317=CARTESIAN_POINT('Ctrl Pts',(-6.56207308072387,-3.21652610415333,
14.9181782774389));
#78318=CARTESIAN_POINT('Ctrl Pts',(-7.30120792003263,0.314970163523136,
14.7593846759014));
#78319=CARTESIAN_POINT('Ctrl Pts',(-6.26069135448818,3.76969323145719,14.6005910743639));
#78320=CARTESIAN_POINT('Ctrl Pts',(-3.69414672805278,6.30556288106581,14.4417974728264));
#78321=CARTESIAN_POINT('Ctrl Pts',(-0.227162956982798,7.30446714596158,
14.2830038712889));
#78322=CARTESIAN_POINT('Ctrl Pts',(3.2951912240184,6.52292557773042,14.1242102697514));
#78323=CARTESIAN_POINT('Ctrl Pts',(6.01435067952836,4.15143700411245,13.9654166682138));
#78324=CARTESIAN_POINT('Ctrl Pts',(7.26752700548849,0.768045910055647,13.8066230666763));
#78325=CARTESIAN_POINT('Ctrl Pts',(6.74926156636189,-2.80255447837998,13.6478294651388));
#78326=CARTESIAN_POINT('Ctrl Pts',(4.58588028341133,-5.69003913182298,13.4890358636013));
#78327=CARTESIAN_POINT('Ctrl Pts',(1.30470200327209,-7.19059079478976,13.3302422620638));
#78328=CARTESIAN_POINT('Ctrl Pts',(-2.29449416903913,-6.938453704083,13.1714486605263));
#78329=CARTESIAN_POINT('Ctrl Pts',(-5.33441305243017,-4.99508565307144,
13.0126550589887));
#78330=CARTESIAN_POINT('Ctrl Pts',(-7.07408192420626,-1.83417780628703,
12.8538614574512));
#78331=CARTESIAN_POINT('Ctrl Pts',(-7.0894607918695,1.77380635245304,12.6950678559137));
#78332=CARTESIAN_POINT('Ctrl Pts',(-5.37680109439524,4.94942959206086,12.5362742543762));
#78333=CARTESIAN_POINT('Ctrl Pts',(-2.35355940472716,6.91864158804875,12.3774806528387));
#78334=CARTESIAN_POINT('Ctrl Pts',(1.24335657923632,7.20145177810193,12.2186870513011));
#78335=CARTESIAN_POINT('Ctrl Pts',(4.53720746668328,5.72892587661342,12.0598934497636));
#78336=CARTESIAN_POINT('Ctrl Pts',(6.72512523585276,2.85998843661194,11.9010998482261));
#78337=CARTESIAN_POINT('Ctrl Pts',(7.2738103321706,-0.706064123904859,11.7423062466886));
#78338=CARTESIAN_POINT('Ctrl Pts',(6.04952211803567,-4.10001529739278,11.5835126451511));
#78339=CARTESIAN_POINT('Ctrl Pts',(3.35067782304803,-6.49459786450181,11.4247190436135));
#78340=CARTESIAN_POINT('Ctrl Pts',(-0.164885918955666,-7.30613823638642,
11.2659254420761));
#78341=CARTESIAN_POINT('Ctrl Pts',(-3.64025912529407,-6.33682545097865,
11.1071318405385));
#78342=CARTESIAN_POINT('Ctrl Pts',(-6.22832815712936,-3.82292710662485,
10.948338239001));
#78343=CARTESIAN_POINT('Ctrl Pts',(-7.29825757752986,-0.377199718300082,
10.7895446374635));
#78344=CARTESIAN_POINT('Ctrl Pts',(-6.589254731778,3.16046917010732,10.630751035926));
#78345=CARTESIAN_POINT('Ctrl Pts',(-4.27413731309761,5.92778150105453,10.4719574343885));
#78346=CARTESIAN_POINT('Ctrl Pts',(-0.917209476593015,7.25021172597777,
10.313163832851));
#78347=CARTESIAN_POINT('Ctrl Pts',(2.66328590537004,6.80542074244604,10.1543702313134));
#78348=CARTESIAN_POINT('Ctrl Pts',(5.59461192317713,4.70182525456889,9.99557662977594));
#78349=CARTESIAN_POINT('Ctrl Pts',(7.16226509701906,1.45217146903525,9.8367830282384));
#78350=CARTESIAN_POINT('Ctrl Pts',(6.98413383608689,-2.15144552686879,9.67798942670091));
#78351=CARTESIAN_POINT('Ctrl Pts',(5.10363719545182,-5.2306529872147,9.51919582516338));
#78352=CARTESIAN_POINT('Ctrl Pts',(1.97914158858717,-7.03490169567296,9.36040222362587));
#78353=CARTESIAN_POINT('Ctrl Pts',(-1.62776489427362,-7.12441048399288,
9.20160862208835));
#78354=CARTESIAN_POINT('Ctrl Pts',(-4.83790770287762,-5.47736180600617,
9.04281502055083));
#78355=CARTESIAN_POINT('Ctrl Pts',(-6.86882245301825,-2.49521971064066,
8.88402141901332));
#78356=CARTESIAN_POINT('Ctrl Pts',(-7.22547868839144,1.09512602884728,8.7252278174758));
#78357=CARTESIAN_POINT('Ctrl Pts',(-5.82094233215892,4.41853750251569,8.56643421593827));
#78358=CARTESIAN_POINT('Ctrl Pts',(-2.99756565354991,6.66494136869301,8.40764061440078));
#78359=CARTESIAN_POINT('Ctrl Pts',(0.556460252544306,7.28678223105342,8.24884701286324));
#78360=CARTESIAN_POINT('Ctrl Pts',(3.97485034590289,6.13248791463411,8.09005341132574));
#78361=CARTESIAN_POINT('Ctrl Pts',(6.42438048079358,3.48341480927208,7.93125980978821));
#78362=CARTESIAN_POINT('Ctrl Pts',(7.30798373438186,-0.0147320557892091,
7.7724662082507));
#78363=CARTESIAN_POINT('Ctrl Pts',(6.41028399509764,-3.50928801862323,7.61367260671317));
#78364=CARTESIAN_POINT('Ctrl Pts',(3.95009335809719,-6.14846369085595,7.45487900517566));
#78365=CARTESIAN_POINT('Ctrl Pts',(0.527077217284989,-7.28896651813388,
7.29608540363814));
#78366=CARTESIAN_POINT('Ctrl Pts',(-3.02441269396098,-6.65280175204892,
7.13729180210062));
#78367=CARTESIAN_POINT('Ctrl Pts',(-5.83870947790314,-4.39503298373306,
6.9784982005631));
#78368=CARTESIAN_POINT('Ctrl Pts',(-7.22983524155821,-1.06598577635001,
6.81970459902561));
#78369=CARTESIAN_POINT('Ctrl Pts',(-6.85870651452891,2.52289283224952,6.66091099748806));
#78370=CARTESIAN_POINT('Ctrl Pts',(-4.81578500776411,5.49682254165551,6.50211739595056));
#78371=CARTESIAN_POINT('Ctrl Pts',(-1.59902779485203,7.13091532741401,6.34332379441303));
#78372=CARTESIAN_POINT('Ctrl Pts',(2.00748849528066,7.02686510734148,6.18453019287553));
#78373=CARTESIAN_POINT('Ctrl Pts',(5.12468442089522,5.21003386569524,6.02573659133799));
#78374=CARTESIAN_POINT('Ctrl Pts',(6.99275117104099,2.12326973212599,5.8669429898005));
#78375=CARTESIAN_POINT('Ctrl Pts',(7.1563520873638,-1.48103615659492,5.70814938826297));
#78376=CARTESIAN_POINT('Ctrl Pts',(5.57560985041754,-4.72434313861562,5.54935578672546));
#78377=CARTESIAN_POINT('Ctrl Pts',(2.63582647782784,-6.81610314433688,5.39056218518792));
#78378=CARTESIAN_POINT('Ctrl Pts',(-0.94643309124788,-7.2464548366252,5.23176858365042));
#78379=CARTESIAN_POINT('Ctrl Pts',(-4.29800193094195,-5.91050105296297,
5.07297498211289));
#78380=CARTESIAN_POINT('Ctrl Pts',(-6.60194341113072,-3.13387722983619,
4.91418138057538));
#78381=CARTESIAN_POINT('Ctrl Pts',(-7.29667748412521,0.406621430961608,
4.75538777903787));
#78382=CARTESIAN_POINT('Ctrl Pts',(-6.21286443483388,3.84800712185327,4.59659417750035));
#78383=CARTESIAN_POINT('Ctrl Pts',(-3.61468101823925,6.35145057698171,4.43780057596283));
#78384=CARTESIAN_POINT('Ctrl Pts',(-0.135428027587841,7.30674363480701,
4.27900697442531));
#78385=CARTESIAN_POINT('Ctrl Pts',(3.37683521043622,6.48103597097203,4.1202133728878));
#78386=CARTESIAN_POINT('Ctrl Pts',(6.06600320284556,4.0755917899732,3.96141977135028));
#78387=CARTESIAN_POINT('Ctrl Pts',(7.27659789067257,0.676732172240444,3.80262616981276));
#78388=CARTESIAN_POINT('Ctrl Pts',(6.71353980753754,-2.88707924173838,3.64383256827526));
#78389=CARTESIAN_POINT('Ctrl Pts',(4.51407297111273,-5.74717221829848,3.48503896673773));
#78390=CARTESIAN_POINT('Ctrl Pts',(1.21431199256477,-7.2064061556807,3.32624536520021));
#78391=CARTESIAN_POINT('Ctrl Pts',(-2.38143453615604,-6.9090963840742,3.16745176366269));
#78392=CARTESIAN_POINT('Ctrl Pts',(-5.39671227621279,-4.92771142671896,
3.00865816212518));
#78393=CARTESIAN_POINT('Ctrl Pts',(-7.09655472247411,-1.74520897437011,
2.84986456058766));
#78394=CARTESIAN_POINT('Ctrl Pts',(-7.06662947590349,1.86268385571119,2.69107095905014));
#78395=CARTESIAN_POINT('Ctrl Pts',(-5.31423074035417,5.01655209682087,2.53227735751262));
#78396=CARTESIAN_POINT('Ctrl Pts',(-2.26650138338798,6.94764814525486,2.37348375597511));
#78397=CARTESIAN_POINT('Ctrl Pts',(1.3336820929718,7.18527211938174,2.21469015443759));
#78398=CARTESIAN_POINT('Ctrl Pts',(4.6087838462063,5.67150373744236,2.05589655290007));
#78399=CARTESIAN_POINT('Ctrl Pts',(6.76050592645423,2.7753203538901,1.89710295136255));
#78400=CARTESIAN_POINT('Ctrl Pts',(7.26437135605648,-0.797340577473384,
1.73830934982504));
#78401=CARTESIAN_POINT('Ctrl Pts',(5.99756424523123,-4.17565158683848,1.57951574828752));
#78402=CARTESIAN_POINT('Ctrl Pts',(3.26886557238479,-6.5361580764171,1.42072214675001));
#78403=CARTESIAN_POINT('Ctrl Pts',(-0.256610847367315,-7.3034916889936,
1.26192854521248));
#78404=CARTESIAN_POINT('Ctrl Pts',(-3.71953933312641,-6.29061818321811,
1.10313494367497));
#78405=CARTESIAN_POINT('Ctrl Pts',(-6.27583864718436,-3.74442015813873,
0.944341342137453));
#78406=CARTESIAN_POINT('Ctrl Pts',(-7.30241904852373,-0.285532637982764,
0.785547740599942));
#78407=CARTESIAN_POINT('Ctrl Pts',(-6.54905035033283,3.24295998468523,0.626754139062419));
#78408=CARTESIAN_POINT('Ctrl Pts',(-4.19937168621273,5.98097490181152,0.467960537524906));
#78409=CARTESIAN_POINT('Ctrl Pts',(-0.826096925787518,7.26116991578662,
0.309166935987384));
#78410=CARTESIAN_POINT('Ctrl Pts',(2.74851800665292,6.77141768319735,0.15037333444987));
#78411=CARTESIAN_POINT('Ctrl Pts',(5.65322566751968,4.63125733214954,-0.00842026708764997));
#78412=CARTESIAN_POINT('Ctrl Pts',(7.17990031857721,1.36202628232418,-0.167213868625169));
#78413=CARTESIAN_POINT('Ctrl Pts',(6.95663626177777,-2.23877288639238,-0.326007470162682));
#78414=CARTESIAN_POINT('Ctrl Pts',(5.03742250863045,-5.29474283456939,-0.484801071700202));
#78415=CARTESIAN_POINT('Ctrl Pts',(2.9397676306177,-6.47024305947933,-0.590663472725211));
#78416=CARTESIAN_POINT('Ctrl Pts',(1.81369031944497,-6.77183848624123,-0.643594673237717));
#78417=CARTESIAN_POINT('Ctrl Pts',(5.59097265709334,4.82067117646242,20.2142331247627));
#78418=CARTESIAN_POINT('Ctrl Pts',(6.39273246162839,3.8908002029388,20.1612928742045));
#78419=CARTESIAN_POINT('Ctrl Pts',(7.5224104798795,1.62441863265741,20.0554214231337));
#78420=CARTESIAN_POINT('Ctrl Pts',(7.38229754968369,-2.17322098997506,19.8966187715504));
#78421=CARTESIAN_POINT('Ctrl Pts',(5.44303938139093,-5.44000303126678,19.7378251700128));
#78422=CARTESIAN_POINT('Ctrl Pts',(2.17692908499447,-7.38125096895092,19.5790315684753));
#78423=CARTESIAN_POINT('Ctrl Pts',(-1.6197397267044,-7.52310827264703,19.4202379669378));
#78424=CARTESIAN_POINT('Ctrl Pts',(-5.02163271731505,-5.83134276377425,
19.2614443654003));
#78425=CARTESIAN_POINT('Ctrl Pts',(-7.19949900213887,-2.71814276268464,
19.1026507638628));
#78426=CARTESIAN_POINT('Ctrl Pts',(-7.62251337862843,1.05756778685438,18.9438571623252));
#78427=CARTESIAN_POINT('Ctrl Pts',(-6.18755476990059,4.5755140705556,18.7850635607877));
#78428=CARTESIAN_POINT('Ctrl Pts',(-3.2443970811745,6.9781823323029,18.6262699592502));
#78429=CARTESIAN_POINT('Ctrl Pts',(0.489575463363619,7.67993982552714,18.4674763577127));
#78430=CARTESIAN_POINT('Ctrl Pts',(4.10421464975624,6.50972894048726,18.3086827561752));
#78431=CARTESIAN_POINT('Ctrl Pts',(6.71846192640929,3.75278871786083,18.1498891546376));
#78432=CARTESIAN_POINT('Ctrl Pts',(7.69510055389895,0.0811149917897368,
17.9910955531002));
#78433=CARTESIAN_POINT('Ctrl Pts',(6.7960774914506,-3.61033004963708,17.8323019515626));
#78434=CARTESIAN_POINT('Ctrl Pts',(4.24052728243949,-6.42176618888618,17.6735083500251));
#78435=CARTESIAN_POINT('Ctrl Pts',(0.651359036195312,-7.66791260589571,
17.5147147484876));
#78436=CARTESIAN_POINT('Ctrl Pts',(-3.09657637646184,-7.04502429085348,
17.3559211469501));
#78437=CARTESIAN_POINT('Ctrl Pts',(-6.08972893756129,-4.70492868047947,
17.1971275454125));
#78438=CARTESIAN_POINT('Ctrl Pts',(-7.59852510725709,-1.21801832899748,
17.038333943875));
#78439=CARTESIAN_POINT('Ctrl Pts',(-7.25519954050563,2.56578098761301,16.8795403423375));
#78440=CARTESIAN_POINT('Ctrl Pts',(-5.14343699845378,5.72417752073118,16.7207467408));
#78441=CARTESIAN_POINT('Ctrl Pts',(-1.77797438612968,7.48731991653589,16.5619531392625));
#78442=CARTESIAN_POINT('Ctrl Pts',(2.02086509308187,7.42544656722586,16.403159537725));
#78443=CARTESIAN_POINT('Ctrl Pts',(5.3271236951691,5.55363894984081,16.2443659361875));
#78444=CARTESIAN_POINT('Ctrl Pts',(7.33490904843519,2.3281455494303,16.0855723346499));
#78445=CARTESIAN_POINT('Ctrl Pts',(7.55482843002453,-1.46482758071166,15.9267787331124));
#78446=CARTESIAN_POINT('Ctrl Pts',(5.9332770335924,-4.90075260454817,15.7679851315749));
#78447=CARTESIAN_POINT('Ctrl Pts',(2.86550400865343,-7.14213128027408,15.6091915300374));
#78448=CARTESIAN_POINT('Ctrl Pts',(-0.900728543871616,-7.64263308936021,
15.4503979284999));
#78449=CARTESIAN_POINT('Ctrl Pts',(-4.4474107375985,-6.28026195149481,15.2916043269623));
#78450=CARTESIAN_POINT('Ctrl Pts',(-6.91004754406753,-3.38709246803788,
15.1328107254248));
#78451=CARTESIAN_POINT('Ctrl Pts',(-7.68837732160438,0.331672442250143,
14.9740171238873));
#78452=CARTESIAN_POINT('Ctrl Pts',(-6.59268410852166,3.96959301359157,14.8152235223498));
#78453=CARTESIAN_POINT('Ctrl Pts',(-3.89004042039568,6.63993508823676,14.6564299208123));
#78454=CARTESIAN_POINT('Ctrl Pts',(-0.239208983760499,7.69180937818906,
14.4976363192748));
#78455=CARTESIAN_POINT('Ctrl Pts',(3.46992905209301,6.86882412220246,14.3388427177373));
#78456=CARTESIAN_POINT('Ctrl Pts',(6.33328044826521,4.37157994458877,14.1800491161997));
#78457=CARTESIAN_POINT('Ctrl Pts',(7.65291037115065,0.808773948297097,14.0212555146622));
#78458=CARTESIAN_POINT('Ctrl Pts',(7.10716228502651,-2.95116870114297,13.8624619131247));
#78459=CARTESIAN_POINT('Ctrl Pts',(4.82906093851039,-5.99177126569951,13.7036683115872));
#78460=CARTESIAN_POINT('Ctrl Pts',(1.37388791050401,-7.57189437708162,13.5448747100497));
#78461=CARTESIAN_POINT('Ctrl Pts',(-2.41616690375189,-7.30638692799138,
13.3860811085121));
#78462=CARTESIAN_POINT('Ctrl Pts',(-5.61728700039421,-5.25996570364403,
13.2272875069746));
#78463=CARTESIAN_POINT('Ctrl Pts',(-7.44920725898131,-1.93144082514832,
13.0684939054371));
#78464=CARTESIAN_POINT('Ctrl Pts',(-7.46540163923577,1.86786798602179,12.9097003038996));
#78465=CARTESIAN_POINT('Ctrl Pts',(-5.66192280095226,5.21188858710221,12.7509067023621));
#78466=CARTESIAN_POINT('Ctrl Pts',(-2.47836425842699,7.28552421249568,12.5921131008245));
#78467=CARTESIAN_POINT('Ctrl Pts',(1.30928945335738,7.58333129802704,12.433319499287));
#78468=CARTESIAN_POINT('Ctrl Pts',(4.77780709333722,6.03272010184176,12.2745258977495));
#78469=CARTESIAN_POINT('Ctrl Pts',(7.08174605004928,3.01164827476927,12.115732296212));
#78470=CARTESIAN_POINT('Ctrl Pts',(7.6595268908959,-0.743505383942599,11.9569386946745));
#78471=CARTESIAN_POINT('Ctrl Pts',(6.37031696238033,-4.31743144092858,11.798145093137));
#78472=CARTESIAN_POINT('Ctrl Pts',(3.52835800170037,-6.83899424331869,11.6393514915994));
#78473=CARTESIAN_POINT('Ctrl Pts',(-0.173629510874831,-7.69356908341393,
11.4805578900619));
#78474=CARTESIAN_POINT('Ctrl Pts',(-3.83329525884111,-6.67285545376605,
11.3217642885244));
#78475=CARTESIAN_POINT('Ctrl Pts',(-6.55860475133126,-4.0256497816035,11.1629706869869));
#78476=CARTESIAN_POINT('Ctrl Pts',(-7.68527052795628,-0.397201913937679,
11.0041770854494));
#78477=CARTESIAN_POINT('Ctrl Pts',(-6.93867058724303,3.32806293961483,10.8453834839119));
#78478=CARTESIAN_POINT('Ctrl Pts',(-4.50078682149019,6.24212066815513,10.6865898823743));
#78479=CARTESIAN_POINT('Ctrl Pts',(-0.965847379808193,7.63467689474983,
10.5277962808368));
#78480=CARTESIAN_POINT('Ctrl Pts',(2.80451497616083,7.16629947719176,10.3690026792993));
#78481=CARTESIAN_POINT('Ctrl Pts',(5.89128373064334,4.95115425465278,10.2102090777618));
#78482=CARTESIAN_POINT('Ctrl Pts',(7.54206662053171,1.52917740624509,10.0514154762243));
#78483=CARTESIAN_POINT('Ctrl Pts',(7.35448939196629,-2.2655326596111,9.89262187468675));
#78484=CARTESIAN_POINT('Ctrl Pts',(5.37427353130809,-5.5080247329683,9.73382827314923));
#78485=CARTESIAN_POINT('Ctrl Pts',(2.08409176571836,-7.40794937620217,9.57503467161171));
#78486=CARTESIAN_POINT('Ctrl Pts',(-1.71408222243603,-7.50220464817096,
9.4162410700742));
#78487=CARTESIAN_POINT('Ctrl Pts',(-5.09445290069936,-5.76781605903527,
9.25744746853669));
#78488=CARTESIAN_POINT('Ctrl Pts',(-7.23306326190427,-2.62753654543564,
9.09865386699916));
#78489=CARTESIAN_POINT('Ctrl Pts',(-7.60863231043503,1.15319851409607,8.93986026546165));
#78490=CARTESIAN_POINT('Ctrl Pts',(-6.12961601793934,4.65284428290165,8.78106666392412));
#78491=CARTESIAN_POINT('Ctrl Pts',(-3.15652095423003,7.01837074496753,8.62227306238662));
#78492=CARTESIAN_POINT('Ctrl Pts',(0.585968299066983,7.67318666531695,8.46347946084909));
#78493=CARTESIAN_POINT('Ctrl Pts',(4.18562922613967,6.45768228001306,8.30468585931157));
#78494=CARTESIAN_POINT('Ctrl Pts',(6.76505336307016,3.66813378206446,8.14589225777407));
#78495=CARTESIAN_POINT('Ctrl Pts',(7.69551244471668,-0.0155132691564084,
7.98709865623654));
#78496=CARTESIAN_POINT('Ctrl Pts',(6.75020936710044,-3.69537899932045,7.82830505469903));
#78497=CARTESIAN_POINT('Ctrl Pts',(4.15955942157017,-6.47450522177069,7.6695114531615));
#78498=CARTESIAN_POINT('Ctrl Pts',(0.55502713639884,-7.67548678105631,7.51071785162399));
#78499=CARTESIAN_POINT('Ctrl Pts',(-3.18479164298584,-7.00558738715583,
7.35192425008647));
#78500=CARTESIAN_POINT('Ctrl Pts',(-6.14832532219495,-4.62809336344519,
7.19313064854895));
#78501=CARTESIAN_POINT('Ctrl Pts',(-7.61321988346879,-1.12251300850581,
7.03433704701144));
#78502=CARTESIAN_POINT('Ctrl Pts',(-7.22241089411526,2.65667712093025,6.87554344547392));
#78503=CARTESIAN_POINT('Ctrl Pts',(-5.07115708043697,5.78830876110143,6.71674984393641));
#78504=CARTESIAN_POINT('Ctrl Pts',(-1.68382124837509,7.5090544312736,6.55795624239888));
#78505=CARTESIAN_POINT('Ctrl Pts',(2.11394185586056,7.3994866226212,6.39916264086138));
#78506=CARTESIAN_POINT('Ctrl Pts',(5.39643685175506,5.48631221799571,6.24036903932385));
#78507=CARTESIAN_POINT('Ctrl Pts',(7.36356368807721,2.23586275516634,6.08157543778634));
#78508=CARTESIAN_POINT('Ctrl Pts',(7.53584005503271,-1.55957273420444,5.92278183624882));
#78509=CARTESIAN_POINT('Ctrl Pts',(5.87127401350223,-4.97486621997847,5.7639882347113));
#78510=CARTESIAN_POINT('Ctrl Pts',(2.7755994265296,-7.17754834687707,5.60519463317378));
#78511=CARTESIAN_POINT('Ctrl Pts',(-0.996620668095368,-7.63072078458088,
5.44640103163627));
#78512=CARTESIAN_POINT('Ctrl Pts',(-4.52591693538818,-6.22392387021847,
5.28760743009874));
#78513=CARTESIAN_POINT('Ctrl Pts',(-6.95203212353196,-3.30006087848231,
5.12881382856124));
#78514=CARTESIAN_POINT('Ctrl Pts',(-7.68360664515343,0.428183804998338,
4.97002022702371));
#78515=CARTESIAN_POINT('Ctrl Pts',(-6.54232101676206,4.05205974313583,4.81122662548621));
#78516=CARTESIAN_POINT('Ctrl Pts',(-3.80636079260434,6.68825612284975,4.65243302394867));
#78517=CARTESIAN_POINT('Ctrl Pts',(-0.14260952261873,7.69420658498056,4.49363942241117));
#78518=CARTESIAN_POINT('Ctrl Pts',(3.55590246642325,6.82471318793792,4.33484582087364));
#78519=CARTESIAN_POINT('Ctrl Pts',(6.38767200829543,4.29171280058643,4.17605221933613));
#78520=CARTESIAN_POINT('Ctrl Pts',(7.66246226841205,0.712618013736859,4.01725861779861));
#78521=CARTESIAN_POINT('Ctrl Pts',(7.06954626813712,-3.04017565462741,3.8584650162611));
#78522=CARTESIAN_POINT('Ctrl Pts',(4.75344581873176,-6.0519340129028,3.69967141472358));
#78523=CARTESIAN_POINT('Ctrl Pts',(1.27870468657267,-7.58854839698333,3.54087781318606));
#78524=CARTESIAN_POINT('Ctrl Pts',(-2.50771755594459,-7.27547284420542,
3.38208421164855));
#78525=CARTESIAN_POINT('Ctrl Pts',(-5.68288983550449,-5.18901874806867,
3.22329061011102));
#78526=CARTESIAN_POINT('Ctrl Pts',(-7.47287174771356,-1.83775414246081,
3.06449700857351));
#78527=CARTESIAN_POINT('Ctrl Pts',(-7.4413596212823,1.96145849706257,2.90570340703599));
#78528=CARTESIAN_POINT('Ctrl Pts',(-5.59603445805296,5.28257047275981,2.74690980549847));
#78529=CARTESIAN_POINT('Ctrl Pts',(-2.38668971302865,7.31606893318352,2.58811620396096));
#78530=CARTESIAN_POINT('Ctrl Pts',(1.40440476016309,7.56629366226348,2.42932260242343));
#78531=CARTESIAN_POINT('Ctrl Pts',(4.85317903440706,5.97225297401905,2.27052900088592));
#78532=CARTESIAN_POINT('Ctrl Pts',(7.1190029125058,2.92249040196356,2.1117353993484));
#78533=CARTESIAN_POINT('Ctrl Pts',(7.64958738353084,-0.839622057142283,
1.95294179781089));
#78534=CARTESIAN_POINT('Ctrl Pts',(6.3156038607506,-4.39707858135161,1.79414819627337));
#78535=CARTESIAN_POINT('Ctrl Pts',(3.44220740038646,-6.88275831554759,1.63535459473586));
#78536=CARTESIAN_POINT('Ctrl Pts',(-0.270218440699842,-7.69078219456233,
1.47656099319833));
#78537=CARTESIAN_POINT('Ctrl Pts',(-3.91677954782813,-6.62419790101118,
1.31776739166082));
#78538=CARTESIAN_POINT('Ctrl Pts',(-6.60863463382164,-3.94297975645974,
1.1589737901233));
#78539=CARTESIAN_POINT('Ctrl Pts',(-7.68965267397435,-0.300673899783249,
1.00018018858579));
#78540=CARTESIAN_POINT('Ctrl Pts',(-6.89633424263845,3.41492808781878,0.841386587048263));
#78541=CARTESIAN_POINT('Ctrl Pts',(-4.42205651323531,6.29813481547409,0.682592985510749));
#78542=CARTESIAN_POINT('Ctrl Pts',(-0.869903300828535,7.64621617687067,
0.523799383973227));
#78543=CARTESIAN_POINT('Ctrl Pts',(2.89426677637707,7.13049329930227,0.365005782435713));
#78544=CARTESIAN_POINT('Ctrl Pts',(5.95300565223129,4.87684424728084,0.206212180898193));
#78545=CARTESIAN_POINT('Ctrl Pts',(7.56063700490841,1.43425198886865,0.0474185793606738));
#78546=CARTESIAN_POINT('Ctrl Pts',(7.32553367271641,-2.35749082569408,-0.111375022176839));
#78547=CARTESIAN_POINT('Ctrl Pts',(5.30454760347664,-5.57551314506993,-0.27016862371436));
#78548=CARTESIAN_POINT('Ctrl Pts',(3.09565801023329,-6.81334794853324,-0.376031024739368));
#78549=CARTESIAN_POINT('Ctrl Pts',(1.9098669251939,-7.13093641674461,-0.428962225251874));
#78550=CARTESIAN_POINT('Ctrl Pts',(5.87252147387267,5.06342934200153,20.4288655727486));
#78551=CARTESIAN_POINT('Ctrl Pts',(6.71465610013426,4.08673215622288,20.3759253221903));
#78552=CARTESIAN_POINT('Ctrl Pts',(7.90122216432793,1.70622070396583,20.2700538711195));
#78553=CARTESIAN_POINT('Ctrl Pts',(7.75405346188429,-2.28265951451358,20.1112512195362));
#78554=CARTESIAN_POINT('Ctrl Pts',(5.71713861089972,-5.71394935700779,19.9524576179987));
#78555=CARTESIAN_POINT('Ctrl Pts',(2.28655434086387,-7.75295417769812,19.7936640164612));
#78556=CARTESIAN_POINT('Ctrl Pts',(-1.70130617882531,-7.90195509637086,
19.6348704149237));
#78557=CARTESIAN_POINT('Ctrl Pts',(-5.27451085437171,-6.12499607887182,
19.4760768133862));
#78558=CARTESIAN_POINT('Ctrl Pts',(-7.56204959034188,-2.85502232293436,
19.3172832118486));
#78559=CARTESIAN_POINT('Ctrl Pts',(-8.00636602006724,1.11082452361824,19.1584896103111));
#78560=CARTESIAN_POINT('Ctrl Pts',(-6.49914612100703,4.80592667525467,18.9996960087736));
#78561=CARTESIAN_POINT('Ctrl Pts',(-3.40777762609777,7.32958791044281,18.8409024072361));
#78562=CARTESIAN_POINT('Ctrl Pts',(0.514229383332149,8.0666843337605,18.6821088056986));
#78563=CARTESIAN_POINT('Ctrl Pts',(4.31089367491321,6.83754425870798,18.5233152041611));
#78564=CARTESIAN_POINT('Ctrl Pts',(7.05678856865421,3.94177072295006,18.3645216026235));
#78565=CARTESIAN_POINT('Ctrl Pts',(8.08260852233796,0.0851997604627655,
18.205728001086));
#78566=CARTESIAN_POINT('Ctrl Pts',(7.1383126791028,-3.79213815638369,18.0469343995485));
#78567=CARTESIAN_POINT('Ctrl Pts',(4.45407070540305,-6.74515190064075,17.888140798011));
#78568=CARTESIAN_POINT('Ctrl Pts',(0.684160013267999,-8.05405145038072,
17.7293471964735));
#78569=CARTESIAN_POINT('Ctrl Pts',(-3.25251300293659,-7.39979587979247,
17.570553594936));
#78570=CARTESIAN_POINT('Ctrl Pts',(-6.39639399962379,-4.94185831406292,
17.4117599933984));
#78571=CARTESIAN_POINT('Ctrl Pts',(-7.98116975326553,-1.27935499443613,
17.2529663918609));
#78572=CARTESIAN_POINT('Ctrl Pts',(-7.62055508262866,2.6949879513174,17.0941727903234));
#78573=CARTESIAN_POINT('Ctrl Pts',(-5.40244892534212,6.01243423505299,16.9353791887859));
#78574=CARTESIAN_POINT('Ctrl Pts',(-1.86750918005211,7.86436451908362,16.7765855872484));
#78575=CARTESIAN_POINT('Ctrl Pts',(2.12263131708691,7.79937536696847,16.6177919857108));
#78576=CARTESIAN_POINT('Ctrl Pts',(5.59538567125106,5.83330772503389,16.4589983841733));
#78577=CARTESIAN_POINT('Ctrl Pts',(7.70427858222301,2.4453857265756,16.3002047826358));
#78578=CARTESIAN_POINT('Ctrl Pts',(7.93527260957988,-1.53859300533986,16.1414111810983));
#78579=CARTESIAN_POINT('Ctrl Pts',(6.23206352941125,-5.1475434908152,15.9826175795608));
#78580=CARTESIAN_POINT('Ctrl Pts',(3.00980435004202,-7.50179295894329,15.8238239780233));
#78581=CARTESIAN_POINT('Ctrl Pts',(-0.94608720886968,-8.02749891421056,
15.6650303764857));
#78582=CARTESIAN_POINT('Ctrl Pts',(-4.67137234637402,-6.5965218278983,15.5062367749482));
#78583=CARTESIAN_POINT('Ctrl Pts',(-7.2580220074112,-3.55765883192241,15.3474431734107));
#78584=CARTESIAN_POINT('Ctrl Pts',(-8.07554672317612,0.348374720977148,
15.1886495718732));
#78585=CARTESIAN_POINT('Ctrl Pts',(-6.92467686255512,4.16949279572595,15.0298559703357));
#78586=CARTESIAN_POINT('Ctrl Pts',(-4.08593411273857,6.97430729540769,14.8710623687981));
#78587=CARTESIAN_POINT('Ctrl Pts',(-0.251255010538211,8.07915161041654,
14.7122687672607));
#78588=CARTESIAN_POINT('Ctrl Pts',(3.64466688016764,7.21472266667448,14.5534751657231));
#78589=CARTESIAN_POINT('Ctrl Pts',(6.65221021700204,4.5917228850651,14.3946815641856));
#78590=CARTESIAN_POINT('Ctrl Pts',(8.03829373681283,0.849501986538545,14.2358879626481));
#78591=CARTESIAN_POINT('Ctrl Pts',(7.46506300369113,-3.09978292390594,14.0770943611106));
#78592=CARTESIAN_POINT('Ctrl Pts',(5.07224159360946,-6.29350339957605,13.9183007595731));
#78593=CARTESIAN_POINT('Ctrl Pts',(1.44307381773593,-7.95319795937345,13.7595071580355));
#78594=CARTESIAN_POINT('Ctrl Pts',(-2.53783963846463,-7.67432015189977,
13.600713556498));
#78595=CARTESIAN_POINT('Ctrl Pts',(-5.90016094835825,-5.52484575421662,
13.4419199549605));
#78596=CARTESIAN_POINT('Ctrl Pts',(-7.82433259375634,-2.0287038440096,13.283126353423));
#78597=CARTESIAN_POINT('Ctrl Pts',(-7.84134248660204,1.96192961959055,13.1243327518854));
#78598=CARTESIAN_POINT('Ctrl Pts',(-5.94704450750926,5.47434758214355,12.965539150348));
#78599=CARTESIAN_POINT('Ctrl Pts',(-2.60316911212683,7.65240683694259,12.8067455488104));
#78600=CARTESIAN_POINT('Ctrl Pts',(1.37522232747844,7.96521081795215,12.6479519472729));
#78601=CARTESIAN_POINT('Ctrl Pts',(5.01840671999116,6.33651432707009,12.4891583457354));
#78602=CARTESIAN_POINT('Ctrl Pts',(7.43836686424581,3.1633081129266,12.3303647441979));
#78603=CARTESIAN_POINT('Ctrl Pts',(8.04524344962119,-0.780946643980331,
12.1715711426604));
#78604=CARTESIAN_POINT('Ctrl Pts',(6.691111806725,-4.53484758446439,12.0127775411229));
#78605=CARTESIAN_POINT('Ctrl Pts',(3.70603818035271,-7.18339062213555,11.8539839395853));
#78606=CARTESIAN_POINT('Ctrl Pts',(-0.182373102793984,-8.08099993044143,
11.6951903380478));
#78607=CARTESIAN_POINT('Ctrl Pts',(-4.02633139238815,-7.00888545655346,
11.5363967365103));
#78608=CARTESIAN_POINT('Ctrl Pts',(-6.88888134553315,-4.22837245658215,
11.3776031349728));
#78609=CARTESIAN_POINT('Ctrl Pts',(-8.07228347838272,-0.41720410957528,
11.2188095334353));
#78610=CARTESIAN_POINT('Ctrl Pts',(-7.28808644270806,3.49565670912235,11.0600159318977));
#78611=CARTESIAN_POINT('Ctrl Pts',(-4.72743632988278,6.55645983525572,10.9012223303602));
#78612=CARTESIAN_POINT('Ctrl Pts',(-1.01448528302337,8.01914206352189,10.7424287288227));
#78613=CARTESIAN_POINT('Ctrl Pts',(2.94574404695163,7.52717821193747,10.5836351272852));
#78614=CARTESIAN_POINT('Ctrl Pts',(6.18795553810953,5.20048325473668,10.4248415257477));
#78615=CARTESIAN_POINT('Ctrl Pts',(7.92186814404438,1.60618334345491,10.2660479242102));
#78616=CARTESIAN_POINT('Ctrl Pts',(7.72484494784568,-2.37961979235341,10.1072543226726));
#78617=CARTESIAN_POINT('Ctrl Pts',(5.64490986716436,-5.78539647872188,9.94846072113507));
#78618=CARTESIAN_POINT('Ctrl Pts',(2.18904194284954,-7.78099705673138,9.78966711959756));
#78619=CARTESIAN_POINT('Ctrl Pts',(-1.80039955059843,-7.87999881234902,
9.63087351806003));
#78620=CARTESIAN_POINT('Ctrl Pts',(-5.3509980985211,-6.05827031206438,9.47207991652253));
#78621=CARTESIAN_POINT('Ctrl Pts',(-7.59730407079027,-2.75985338023062,
9.31328631498499));
#78622=CARTESIAN_POINT('Ctrl Pts',(-7.99178593247863,1.21127099934486,9.15449271344749));
#78623=CARTESIAN_POINT('Ctrl Pts',(-6.43828970371974,4.88715106328761,8.99569911190997));
#78624=CARTESIAN_POINT('Ctrl Pts',(-3.31547625491016,7.37180012124203,8.83690551037245));
#78625=CARTESIAN_POINT('Ctrl Pts',(0.615476345589656,8.05959109958046,8.67811190883494));
#78626=CARTESIAN_POINT('Ctrl Pts',(4.39640810637647,6.78287664539203,8.51931830729741));
#78627=CARTESIAN_POINT('Ctrl Pts',(7.10572624534672,3.85285275485684,8.36052470575991));
#78628=CARTESIAN_POINT('Ctrl Pts',(8.08304115505151,-0.0162944825236051,
8.20173110422238));
#78629=CARTESIAN_POINT('Ctrl Pts',(7.09013473910324,-3.88146998001768,8.04293750268486));
#78630=CARTESIAN_POINT('Ctrl Pts',(4.36902548504316,-6.80054675268545,7.88414390114735));
#78631=CARTESIAN_POINT('Ctrl Pts',(0.582977055512693,-8.06200704397873,
7.72535029960982));
#78632=CARTESIAN_POINT('Ctrl Pts',(-3.3451705920107,-7.35837302226273,7.56655669807232));
#78633=CARTESIAN_POINT('Ctrl Pts',(-6.45794116648677,-4.86115374315731,
7.40776309653478));
#78634=CARTESIAN_POINT('Ctrl Pts',(-7.99660452537937,-1.17904024066161,
7.24896949499729));
#78635=CARTESIAN_POINT('Ctrl Pts',(-7.5861152737016,2.79046140961099,7.09017589345975));
#78636=CARTESIAN_POINT('Ctrl Pts',(-5.32652915310981,6.07979498054733,6.93138229192225));
#78637=CARTESIAN_POINT('Ctrl Pts',(-1.76861470189815,7.88719353513318,6.77258869038473));
#78638=CARTESIAN_POINT('Ctrl Pts',(2.22039521644045,7.77210813790092,6.61379508884721));
#78639=CARTESIAN_POINT('Ctrl Pts',(5.66818928261491,5.76259057029618,6.45500148730969));
#78640=CARTESIAN_POINT('Ctrl Pts',(7.73437620511342,2.3484557782067,6.29620788577219));
#78641=CARTESIAN_POINT('Ctrl Pts',(7.91532802270162,-1.63810931181399,6.13741428423465));
#78642=CARTESIAN_POINT('Ctrl Pts',(6.16693817658691,-5.2253893013413,5.97862068269715));
#78643=CARTESIAN_POINT('Ctrl Pts',(2.91537237523135,-7.53899354941726,5.81982708115961));
#78644=CARTESIAN_POINT('Ctrl Pts',(-1.04680824494286,-8.01498673253654,
5.66103347962212));
#78645=CARTESIAN_POINT('Ctrl Pts',(-4.7538319398344,-6.53734668747398,5.50223987808458));
#78646=CARTESIAN_POINT('Ctrl Pts',(-7.30212083593321,-3.46624452712843,
5.34344627654708));
#78647=CARTESIAN_POINT('Ctrl Pts',(-8.07053580618163,0.449746179035062,
5.18465267500954));
#78648=CARTESIAN_POINT('Ctrl Pts',(-6.87177759869027,4.25611236441841,5.02585907347205));
#78649=CARTESIAN_POINT('Ctrl Pts',(-3.99804056696941,7.02506166871776,4.86706547193452));
#78650=CARTESIAN_POINT('Ctrl Pts',(-0.149791017649627,8.08166953515412,
4.70827187039701));
#78651=CARTESIAN_POINT('Ctrl Pts',(3.73496972241026,7.16839040490381,4.54947826885948));
#78652=CARTESIAN_POINT('Ctrl Pts',(6.70934081374529,4.50783381119964,4.39068466732197));
#78653=CARTESIAN_POINT('Ctrl Pts',(8.04832664615152,0.748503855233274,4.23189106578445));
#78654=CARTESIAN_POINT('Ctrl Pts',(7.42555272873669,-3.19327206751645,4.07309746424694));
#78655=CARTESIAN_POINT('Ctrl Pts',(4.9928186663508,-6.35669580750712,3.91430386270942));
#78656=CARTESIAN_POINT('Ctrl Pts',(1.34309738058055,-7.97069063828595,3.7555102611719));
#78657=CARTESIAN_POINT('Ctrl Pts',(-2.63400057573315,-7.64184930433663,
3.59671665963439));
#78658=CARTESIAN_POINT('Ctrl Pts',(-5.96906739479618,-5.45032606941837,
3.43792305809687));
#78659=CARTESIAN_POINT('Ctrl Pts',(-7.84918877295303,-1.9302993105515,3.27912945655935));
#78660=CARTESIAN_POINT('Ctrl Pts',(-7.81608976666111,2.06023313841395,3.12033585502182));
#78661=CARTESIAN_POINT('Ctrl Pts',(-5.87783817575176,5.54858884869876,2.96154225348432));
#78662=CARTESIAN_POINT('Ctrl Pts',(-2.50687804266929,7.68448972111217,2.8027486519468));
#78663=CARTESIAN_POINT('Ctrl Pts',(1.47512742735437,7.94731520514522,2.64395505040928));
#78664=CARTESIAN_POINT('Ctrl Pts',(5.09757422260781,6.27300221059572,2.48516144887177));
#78665=CARTESIAN_POINT('Ctrl Pts',(7.47749989855737,3.06966045003703,2.32636784733424));
#78666=CARTESIAN_POINT('Ctrl Pts',(8.03480341100519,-0.88190353681118,2.16757424579673));
#78667=CARTESIAN_POINT('Ctrl Pts',(6.63364347627,-4.61850557586475,2.00878064425921));
#78668=CARTESIAN_POINT('Ctrl Pts',(3.61554922838812,-7.22935855467807,1.8499870427217));
#78669=CARTESIAN_POINT('Ctrl Pts',(-0.283826034032366,-8.07807270013105,
1.69119344118417));
#78670=CARTESIAN_POINT('Ctrl Pts',(-4.11401976252985,-6.95777761880423,
1.53239983964667));
#78671=CARTESIAN_POINT('Ctrl Pts',(-6.94143062045892,-4.14153935478073,
1.37360623810914));
#78672=CARTESIAN_POINT('Ctrl Pts',(-8.07688629942497,-0.315815161583738,
1.21481263657163));
#78673=CARTESIAN_POINT('Ctrl Pts',(-7.24361813494408,3.58689619095233,1.05601903503411));
#78674=CARTESIAN_POINT('Ctrl Pts',(-4.64474134025788,6.61529472913664,0.897225433496593));
#78675=CARTESIAN_POINT('Ctrl Pts',(-0.913709675869558,8.03126243795472,
0.73843183195907));
#78676=CARTESIAN_POINT('Ctrl Pts',(3.04001554610122,7.48956891540719,0.579638230421557));
#78677=CARTESIAN_POINT('Ctrl Pts',(6.25278563694289,5.12243116241214,0.420844628884037));
#78678=CARTESIAN_POINT('Ctrl Pts',(7.94137369123961,1.50647769541312,0.262051027346517));
#78679=CARTESIAN_POINT('Ctrl Pts',(7.69443108365505,-2.4762087649958,0.103257425809005));
#78680=CARTESIAN_POINT('Ctrl Pts',(5.57167269832283,-5.85628345557045,-0.0555361757285161));
#78681=CARTESIAN_POINT('Ctrl Pts',(3.25154838984888,-7.15645283758716,-0.161398576753524));
#78682=CARTESIAN_POINT('Ctrl Pts',(2.00604353094284,-7.49003434724797,-0.214329777266031));
#78683=CARTESIAN_POINT('Ctrl Pts',(6.15407029065202,5.30618750754062,20.6434980207344));
#78684=CARTESIAN_POINT('Ctrl Pts',(7.03657973864013,4.28266410950697,20.5905577701761));
#78685=CARTESIAN_POINT('Ctrl Pts',(8.28003384877634,1.78802277527426,20.4846863191053));
#78686=CARTESIAN_POINT('Ctrl Pts',(8.12580937408491,-2.39209803905211,20.325883667522));
#78687=CARTESIAN_POINT('Ctrl Pts',(5.9912378404085,-5.98789568274879,20.1670900659845));
#78688=CARTESIAN_POINT('Ctrl Pts',(2.39617959673327,-8.12465738644534,20.008296464447));
#78689=CARTESIAN_POINT('Ctrl Pts',(-1.78287263094621,-8.28080192009469,
19.8495028629095));
#78690=CARTESIAN_POINT('Ctrl Pts',(-5.52738899142837,-6.41864939396941,
19.6907092613719));
#78691=CARTESIAN_POINT('Ctrl Pts',(-7.92460017854491,-2.9919018831841,19.5319156598344));
#78692=CARTESIAN_POINT('Ctrl Pts',(-8.39021866150606,1.16408126038211,19.3731220582969));
#78693=CARTESIAN_POINT('Ctrl Pts',(-6.81073747211346,5.03633927995374,19.2143284567594));
#78694=CARTESIAN_POINT('Ctrl Pts',(-3.57115817102104,7.68099348858274,19.0555348552219));
#78695=CARTESIAN_POINT('Ctrl Pts',(0.538883303300684,8.45342884199385,18.8967412536844));
#78696=CARTESIAN_POINT('Ctrl Pts',(4.51757270007016,7.16535957692872,18.7379476521468));
#78697=CARTESIAN_POINT('Ctrl Pts',(7.39511521089914,4.13075272803929,18.5791540506093));
#78698=CARTESIAN_POINT('Ctrl Pts',(8.47011649077696,0.0892845291357988,
18.4203604490718));
#78699=CARTESIAN_POINT('Ctrl Pts',(7.48054786675499,-3.97394626313031,18.2615668475343));
#78700=CARTESIAN_POINT('Ctrl Pts',(4.66761412836659,-7.06853761239531,18.1027732459967));
#78701=CARTESIAN_POINT('Ctrl Pts',(0.716960990340684,-8.44019029486573,
17.9439796444593));
#78702=CARTESIAN_POINT('Ctrl Pts',(-3.40844962941133,-7.75456746873147,
17.7851860429217));
#78703=CARTESIAN_POINT('Ctrl Pts',(-6.70305906168629,-5.17878794764635,
17.6263924413842));
#78704=CARTESIAN_POINT('Ctrl Pts',(-8.36381439927396,-1.34069165987479,
17.4675988398467));
#78705=CARTESIAN_POINT('Ctrl Pts',(-7.98591062475169,2.82419491502181,17.3088052383092));
#78706=CARTESIAN_POINT('Ctrl Pts',(-5.66146085223045,6.30069094937478,17.1500116367717));
#78707=CARTESIAN_POINT('Ctrl Pts',(-1.95704397397453,8.24140912163137,16.9912180352342));
#78708=CARTESIAN_POINT('Ctrl Pts',(2.22439754109196,8.17330416671108,16.8324244336966));
#78709=CARTESIAN_POINT('Ctrl Pts',(5.86364764733302,6.11297650022698,16.6736308321591));
#78710=CARTESIAN_POINT('Ctrl Pts',(8.07364811601082,2.5626259037209,16.5148372306216));
#78711=CARTESIAN_POINT('Ctrl Pts',(8.31571678913525,-1.61235842996804,16.3560436290841));
#78712=CARTESIAN_POINT('Ctrl Pts',(6.53085002523011,-5.39433437708224,16.1972500275466));
#78713=CARTESIAN_POINT('Ctrl Pts',(3.1541046914306,-7.86145463761249,16.038456426009));
#78714=CARTESIAN_POINT('Ctrl Pts',(-0.991445873867747,-8.41236473906092,
15.8796628244715));
#78715=CARTESIAN_POINT('Ctrl Pts',(-4.89533395514954,-6.9127817043018,15.720869222934));
#78716=CARTESIAN_POINT('Ctrl Pts',(-7.60599647075488,-3.72822519580695,
15.5620756213965));
#78717=CARTESIAN_POINT('Ctrl Pts',(-8.46271612474785,0.365076999704155,
15.403282019859));
#78718=CARTESIAN_POINT('Ctrl Pts',(-7.25666961658859,4.36939257786033,15.2444884183215));
#78719=CARTESIAN_POINT('Ctrl Pts',(-4.28182780508147,7.30867950257863,15.0856948167839));
#78720=CARTESIAN_POINT('Ctrl Pts',(-0.26330103731591,8.46649384264402,14.9269012152464));
#78721=CARTESIAN_POINT('Ctrl Pts',(3.81940470824224,7.5606212111465,14.7681076137089));
#78722=CARTESIAN_POINT('Ctrl Pts',(6.97113998573889,4.81186582554143,14.6093140121714));
#78723=CARTESIAN_POINT('Ctrl Pts',(8.423677102475,0.890230024779997,14.4505204106339));
#78724=CARTESIAN_POINT('Ctrl Pts',(7.82296372235575,-3.24839714666893,14.2917268090964));
#78725=CARTESIAN_POINT('Ctrl Pts',(5.31542224870852,-6.59523553345258,14.1329332075588));
#78726=CARTESIAN_POINT('Ctrl Pts',(1.51225972496784,-8.33450154166531,13.9741396060213));
#78727=CARTESIAN_POINT('Ctrl Pts',(-2.65951237317739,-8.04225337580815,
13.8153460044838));
#78728=CARTESIAN_POINT('Ctrl Pts',(-6.18303489632227,-5.78972580478921,
13.6565524029463));
#78729=CARTESIAN_POINT('Ctrl Pts',(-8.19945792853139,-2.1259668628709,13.4977588014087));
#78730=CARTESIAN_POINT('Ctrl Pts',(-8.21728333396832,2.0559912531593,13.3389651998713));
#78731=CARTESIAN_POINT('Ctrl Pts',(-6.23216621406629,5.7368065771849,13.1801715983337));
#78732=CARTESIAN_POINT('Ctrl Pts',(-2.72797396582666,8.01928946138952,13.0213779967962));
#78733=CARTESIAN_POINT('Ctrl Pts',(1.4411552015995,8.34709033787726,12.8625843952587));
#78734=CARTESIAN_POINT('Ctrl Pts',(5.25900634664509,6.64030855229842,12.7037907937212));
#78735=CARTESIAN_POINT('Ctrl Pts',(7.79498767844233,3.31496795108393,12.5449971921837));
#78736=CARTESIAN_POINT('Ctrl Pts',(8.4309600083465,-0.81838790401807,12.3862035906461));
#78737=CARTESIAN_POINT('Ctrl Pts',(7.01190665106966,-4.75226372800019,12.2274099891087));
#78738=CARTESIAN_POINT('Ctrl Pts',(3.88371835900504,-7.52778700095242,12.0686163875711));
#78739=CARTESIAN_POINT('Ctrl Pts',(-0.191116694713139,-8.46843077746894,
11.9098227860336));
#78740=CARTESIAN_POINT('Ctrl Pts',(-4.21936752593521,-7.34491545934086,
11.7510291844961));
#78741=CARTESIAN_POINT('Ctrl Pts',(-7.21915793973503,-4.43109513156081,
11.5922355829586));
#78742=CARTESIAN_POINT('Ctrl Pts',(-8.45929642880916,-0.437206305212873,
11.4334419814211));
#78743=CARTESIAN_POINT('Ctrl Pts',(-7.63750229817309,3.66325047862986,11.2746483798835));
#78744=CARTESIAN_POINT('Ctrl Pts',(-4.95408583827537,6.87079900235633,11.115854778346));
#78745=CARTESIAN_POINT('Ctrl Pts',(-1.06312318623855,8.40360723229395,10.9570611768085));
#78746=CARTESIAN_POINT('Ctrl Pts',(3.08697311774242,7.88805694668319,10.798267575271));
#78747=CARTESIAN_POINT('Ctrl Pts',(6.48462734557574,5.44981225482057,10.6394739737334));
#78748=CARTESIAN_POINT('Ctrl Pts',(8.30166966755703,1.68318928066475,10.4806803721959));
#78749=CARTESIAN_POINT('Ctrl Pts',(8.09520050372507,-2.49370692509573,10.3218867706584));
#78750=CARTESIAN_POINT('Ctrl Pts',(5.91554620302062,-6.06276822447546,10.1630931691209));
#78751=CARTESIAN_POINT('Ctrl Pts',(2.29399211998073,-8.15404473726062,10.0042995675834));
#78752=CARTESIAN_POINT('Ctrl Pts',(-1.88671687876084,-8.25779297652708,
9.84550596604586));
#78753=CARTESIAN_POINT('Ctrl Pts',(-5.60754329634285,-6.3487245650935,9.68671236450838));
#78754=CARTESIAN_POINT('Ctrl Pts',(-7.96154487967629,-2.8921702150256,9.52791876297083));
#78755=CARTESIAN_POINT('Ctrl Pts',(-8.37493955452223,1.26934348459364,9.36912516143335));
#78756=CARTESIAN_POINT('Ctrl Pts',(-6.74696338950016,5.12145784367357,9.2103315598958));
#78757=CARTESIAN_POINT('Ctrl Pts',(-3.47443155559029,7.72522949751655,9.05153795835831));
#78758=CARTESIAN_POINT('Ctrl Pts',(0.644984392112331,8.44599553384399,8.89274435682078));
#78759=CARTESIAN_POINT('Ctrl Pts',(4.60718698661326,7.10807101077098,8.73395075528327));
#78760=CARTESIAN_POINT('Ctrl Pts',(7.44639912762328,4.03757172764921,8.57515715374574));
#78761=CARTESIAN_POINT('Ctrl Pts',(8.47056986538634,-0.0170756958908047,
8.41636355220823));
#78762=CARTESIAN_POINT('Ctrl Pts',(7.43006011110603,-4.06756096071491,8.2575699506707));
#78763=CARTESIAN_POINT('Ctrl Pts',(4.57849154851613,-7.12658828360019,8.09877634913321));
#78764=CARTESIAN_POINT('Ctrl Pts',(0.610926974626544,-8.44852730690116,
7.93998274759565));
#78765=CARTESIAN_POINT('Ctrl Pts',(-3.50554954103556,-7.71115865736963,
7.78118914605817));
#78766=CARTESIAN_POINT('Ctrl Pts',(-6.76755701077859,-5.09421412286944,
7.62239554452063));
#78767=CARTESIAN_POINT('Ctrl Pts',(-8.37998916728995,-1.23556747281741,
7.46360194298313));
#78768=CARTESIAN_POINT('Ctrl Pts',(-7.94981965328795,2.92424569829173,7.30480834144559));
#78769=CARTESIAN_POINT('Ctrl Pts',(-5.58190122578267,6.37128119999322,7.14601473990809));
#78770=CARTESIAN_POINT('Ctrl Pts',(-1.8534081554212,8.26533263899277,6.98722113837056));
#78771=CARTESIAN_POINT('Ctrl Pts',(2.32684857702034,8.14472965318062,6.82842753683306));
#78772=CARTESIAN_POINT('Ctrl Pts',(5.93994171347475,6.03886892259665,6.66963393529553));
#78773=CARTESIAN_POINT('Ctrl Pts',(8.10518872214963,2.46104880124704,6.51084033375802));
#78774=CARTESIAN_POINT('Ctrl Pts',(8.29481599037053,-1.71664588942351,6.3520467322205));
#78775=CARTESIAN_POINT('Ctrl Pts',(6.46260233967159,-5.47591238270415,6.19325313068298));
#78776=CARTESIAN_POINT('Ctrl Pts',(3.0551453239331,-7.90043875195744,6.03445952914546));
#78777=CARTESIAN_POINT('Ctrl Pts',(-1.09699582179035,-8.39925268049223,
5.87566592760795));
#78778=CARTESIAN_POINT('Ctrl Pts',(-4.98174694428061,-6.85076950472949,
5.71687232607043));
#78779=CARTESIAN_POINT('Ctrl Pts',(-7.65220954833444,-3.63242817577456,
5.55807872453291));
#78780=CARTESIAN_POINT('Ctrl Pts',(-8.45746496720986,0.471308553071791,
5.3992851229954));
#78781=CARTESIAN_POINT('Ctrl Pts',(-7.20123418061844,4.46016498570097,5.24049152145787));
#78782=CARTESIAN_POINT('Ctrl Pts',(-4.18972034133451,7.36186721458578,5.08169791992036));
#78783=CARTESIAN_POINT('Ctrl Pts',(-0.156972512680516,8.46913248532767,
4.92290431838285));
#78784=CARTESIAN_POINT('Ctrl Pts',(3.91403697839729,7.51206762186971,4.76411071684532));
#78785=CARTESIAN_POINT('Ctrl Pts',(7.03100961919515,4.72395482181285,4.60531711530781));
#78786=CARTESIAN_POINT('Ctrl Pts',(8.434191023891,0.78438969672969,4.44652351377029));
#78787=CARTESIAN_POINT('Ctrl Pts',(7.78155918933625,-3.34636848040548,4.28772991223278));
#78788=CARTESIAN_POINT('Ctrl Pts',(5.23219151396984,-6.66145760211143,4.12893631069526));
#78789=CARTESIAN_POINT('Ctrl Pts',(1.40749007458845,-8.3528328795886,3.97014270915774));
#78790=CARTESIAN_POINT('Ctrl Pts',(-2.7602835955217,-8.00822576446783,3.81134910762023));
#78791=CARTESIAN_POINT('Ctrl Pts',(-6.25524495408788,-5.7116333907681,3.65255550608271));
#78792=CARTESIAN_POINT('Ctrl Pts',(-8.22550579819248,-2.02284447864219,
3.49376190454519));
#78793=CARTESIAN_POINT('Ctrl Pts',(-8.19081991203992,2.15900777976532,3.33496830300767));
#78794=CARTESIAN_POINT('Ctrl Pts',(-6.15964189345056,5.81460722463769,3.17617470147015));
#78795=CARTESIAN_POINT('Ctrl Pts',(-2.62706637230996,8.05291050904083,3.01738109993264));
#78796=CARTESIAN_POINT('Ctrl Pts',(1.54585009454566,8.32833674802694,2.85858749839512));
#78797=CARTESIAN_POINT('Ctrl Pts',(5.34196941080857,6.57375144717241,2.6997938968576));
#78798=CARTESIAN_POINT('Ctrl Pts',(7.83599688460893,3.21683049811048,2.54100029532008));
#78799=CARTESIAN_POINT('Ctrl Pts',(8.42001943847956,-0.924185016480067,
2.38220669378257));
#78800=CARTESIAN_POINT('Ctrl Pts',(6.95168309178937,-4.8399325703779,2.22341309224505));
#78801=CARTESIAN_POINT('Ctrl Pts',(3.78889105638979,-7.57595879380855,2.06461949070754));
#78802=CARTESIAN_POINT('Ctrl Pts',(-0.297433627364896,-8.46536320569979,
1.90582588917001));
#78803=CARTESIAN_POINT('Ctrl Pts',(-4.31125997723156,-7.29135733659727,
1.74703228763251));
#78804=CARTESIAN_POINT('Ctrl Pts',(-7.27422660709621,-4.34009895310173,
1.58823868609498));
#78805=CARTESIAN_POINT('Ctrl Pts',(-8.46411992487559,-0.33095642338422,
1.42944508455747));
#78806=CARTESIAN_POINT('Ctrl Pts',(-7.5909020272497,3.75886429408588,1.27065148301995));
#78807=CARTESIAN_POINT('Ctrl Pts',(-4.86742616728046,6.93245464279921,1.11185788148243));
#78808=CARTESIAN_POINT('Ctrl Pts',(-0.957516050910578,8.41630869903879,
0.953064279944913));
#78809=CARTESIAN_POINT('Ctrl Pts',(3.18576431582538,7.8486445315121,0.7942706784074));
#78810=CARTESIAN_POINT('Ctrl Pts',(6.55256562165449,5.36801807754346,0.635477076869881));
#78811=CARTESIAN_POINT('Ctrl Pts',(8.32211037757082,1.57870340195759,0.476683475332361));
#78812=CARTESIAN_POINT('Ctrl Pts',(8.06332849459369,-2.5949267042975,0.317889873794848));
#78813=CARTESIAN_POINT('Ctrl Pts',(5.83879779316903,-6.13705376607098,0.159096272257328));
#78814=CARTESIAN_POINT('Ctrl Pts',(3.40743876946447,-7.49955772664107,0.0532338712323191));
#78815=CARTESIAN_POINT('Ctrl Pts',(2.10222013669177,-7.84913227775134,0.000302670719812688));
#78816=CARTESIAN_POINT('',(5.31060265091893,4.57808054062544,-0.000178101097113292));
#78817=CARTESIAN_POINT('Ctrl Pts',(2.10208451021607,-7.84862588447237,0.));
#78818=CARTESIAN_POINT('Ctrl Pts',(2.29937946956078,-7.78117163610351,1.31601965385565E-15));
#78819=CARTESIAN_POINT('Ctrl Pts',(2.49362179095633,-7.70610038324866,-7.24771166142834E-15));
#78820=CARTESIAN_POINT('Ctrl Pts',(2.68444863542622,-7.6237268130433,-1.66533453693773E-15));
#78821=CARTESIAN_POINT('Ctrl Pts',(2.87762389604612,-7.54033951008384,3.98574227512031E-15));
#78822=CARTESIAN_POINT('Ctrl Pts',(3.06729970067492,-7.44946870591119,-1.02390292508958E-15));
#78823=CARTESIAN_POINT('Ctrl Pts',(3.25307750518592,-7.35139244187101,3.99680288865056E-15));
#78824=CARTESIAN_POINT('Ctrl Pts',(3.43854675272667,-7.25347907196647,9.00916984954207E-15));
#78825=CARTESIAN_POINT('Ctrl Pts',(3.62013148795847,-7.14838371410984,-3.77592803097428E-15));
#78826=CARTESIAN_POINT('Ctrl Pts',(3.79740460673799,-7.03634117918246,-3.77475828372553E-15));
#78827=CARTESIAN_POINT('Ctrl Pts',(3.97213881931131,-6.92590331781892,-3.77360528960083E-15));
#78828=CARTESIAN_POINT('Ctrl Pts',(4.14268447199419,-6.80871537035203,-2.49906849866478E-16));
#78829=CARTESIAN_POINT('Ctrl Pts',(4.30859563250671,-6.68496847023835,-4.10782519111308E-15));
#78830=CARTESIAN_POINT('Ctrl Pts',(4.45093652015492,-6.57880175094424,-7.41766594848549E-15));
#78831=CARTESIAN_POINT('Ctrl Pts',(4.5898657756993,-6.46780662798986,3.44670256380473E-15));
#78832=CARTESIAN_POINT('Ctrl Pts',(4.7250759146848,-6.35208741176991,-4.55191440096314E-15));
#78833=CARTESIAN_POINT('Ctrl Pts',(4.74406958653759,-6.33583173126817,-6.88917332012633E-15));
#78834=CARTESIAN_POINT('Ctrl Pts',(4.76298982572575,-6.31948280724091,4.34243815445731E-15));
#78835=CARTESIAN_POINT('Ctrl Pts',(4.78183573755202,-6.30304090823604,2.77555756156289E-15));
#78836=CARTESIAN_POINT('Ctrl Pts',(4.79992876259441,-6.28725585664597,1.83748770952108E-16));
#78837=CARTESIAN_POINT('Ctrl Pts',(4.81794637150894,-6.27139112825568,1.2337470547172E-15));
#78838=CARTESIAN_POINT('Ctrl Pts',(4.83588620584108,-6.25544870534714,5.55111512312578E-16));
#78839=CARTESIAN_POINT('Ctrl Pts',(4.98981908389951,-6.11865463043536,9.29425087228634E-16));
#78840=CARTESIAN_POINT('Ctrl Pts',(5.1380716025988,-5.97610601005547,-9.7440776070667E-15));
#78841=CARTESIAN_POINT('Ctrl Pts',(5.28026270051223,-5.82804960322368,-8.32667268468867E-16));
#78842=CARTESIAN_POINT('Ctrl Pts',(5.3246867667692,-5.78179306731262,-3.31589168886096E-15));
#78843=CARTESIAN_POINT('Ctrl Pts',(5.36851891763432,-5.73499864303366,8.03106703488735E-17));
#78844=CARTESIAN_POINT('Ctrl Pts',(5.41174677480464,-5.68767313410808,2.16493489801906E-15));
#78845=CARTESIAN_POINT('Ctrl Pts',(5.55047476155044,-5.53579485457413,1.98172015419112E-16));
#78846=CARTESIAN_POINT('Ctrl Pts',(5.68298237898118,-5.37844899954852,4.23059200690762E-15));
#78847=CARTESIAN_POINT('Ctrl Pts',(5.80904637428058,-5.2160751247644,1.18238752122579E-14));
#78848=CARTESIAN_POINT('Ctrl Pts',(5.93507004847681,-5.05375318466423,3.32743196074342E-15));
#78849=CARTESIAN_POINT('Ctrl Pts',(6.05465451261215,-4.8864057750382,-6.33296793918175E-15));
#78850=CARTESIAN_POINT('Ctrl Pts',(6.16753013306389,-4.71444913744807,2.66453525910038E-15));
#78851=CARTESIAN_POINT('Ctrl Pts',(6.27942834154928,-4.54398150585057,1.15841273260136E-14));
#78852=CARTESIAN_POINT('Ctrl Pts',(6.3847336068269,-4.36898347249209,-4.56776605346051E-15));
#78853=CARTESIAN_POINT('Ctrl Pts',(6.48313375932835,-4.18984791395913,-1.08246744900953E-14));
#78854=CARTESIAN_POINT('Ctrl Pts',(6.52516299014066,-4.11333451896046,-1.34971606821353E-14));
#78855=CARTESIAN_POINT('Ctrl Pts',(6.56593183983806,-4.03606618794043,-3.37372497907E-15));
#78856=CARTESIAN_POINT('Ctrl Pts',(6.60541304448959,-3.95807326746694,3.49720252756924E-15));
#78857=CARTESIAN_POINT('Ctrl Pts',(6.62089391761463,-3.92749166497638,6.19134415573078E-15));
#78858=CARTESIAN_POINT('Ctrl Pts',(6.63617853869402,-3.8967948930452,4.15509497561339E-15));
#78859=CARTESIAN_POINT('Ctrl Pts',(6.65125079271779,-3.86601480613085,3.71924713249427E-15));
#78860=CARTESIAN_POINT('Ctrl Pts',(6.74017131234314,-3.68442409526434,1.14791197408907E-15));
#78861=CARTESIAN_POINT('Ctrl Pts',(6.82181117015341,-3.49972844317531,1.40770594749215E-15));
#78862=CARTESIAN_POINT('Ctrl Pts',(6.89596686685091,-3.31234655293863,-1.88737914186277E-15));
#78863=CARTESIAN_POINT('Ctrl Pts',(6.96963536814041,-3.1261957427205,-5.16081585629826E-15));
#78864=CARTESIAN_POINT('Ctrl Pts',(7.03591792826469,-2.93739321795531,8.91671270961761E-15));
#78865=CARTESIAN_POINT('Ctrl Pts',(7.09456670151815,-2.74633316537145,6.66133814775094E-16));
#78866=CARTESIAN_POINT('Ctrl Pts',(7.13773030830017,-2.60571912480418,-5.40602632405713E-15));
#78867=CARTESIAN_POINT('Ctrl Pts',(7.17675810666365,-2.46388192110481,-5.8964836676042E-15));
#78868=CARTESIAN_POINT('Ctrl Pts',(7.21153340893003,-2.32097605948004,-5.38458166943201E-15));
#78869=CARTESIAN_POINT('Ctrl Pts',(7.25901043149182,-2.12587366282507,-3.21840629948907E-15));
#78870=CARTESIAN_POINT('Ctrl Pts',(7.29856300119499,-1.928778789233,-3.33446677566107E-15));
#78871=CARTESIAN_POINT('Ctrl Pts',(7.33014868626891,-1.73017913744427,-1.66533453693773E-16));
#78872=CARTESIAN_POINT('Ctrl Pts',(7.35985712442043,-1.54338295245514,2.81311859258955E-15));
#78873=CARTESIAN_POINT('Ctrl Pts',(7.38251706409064,-1.35525506107842,-1.0991374320194E-14));
#78874=CARTESIAN_POINT('Ctrl Pts',(7.39805220869348,-1.16621087705598,-8.82627304576999E-15));
#78875=CARTESIAN_POINT('Ctrl Pts',(7.40002531232882,-1.14220055875708,-9.18622245425996E-15));
#78876=CARTESIAN_POINT('Ctrl Pts',(7.40188343167553,-1.11817547822278,-1.11028146407842E-14));
#78877=CARTESIAN_POINT('Ctrl Pts',(7.40362636499328,-1.09413650426559,-1.23789867245705E-14));
#78878=CARTESIAN_POINT('Ctrl Pts',(7.40526549208637,-1.07152925182423,-8.27837043642381E-15));
#78879=CARTESIAN_POINT('Ctrl Pts',(7.4068020798626,-1.04891882611431,9.35859446300662E-16));
#78880=CARTESIAN_POINT('Ctrl Pts',(7.40823612148754,-1.02630740886741,-4.9960036108132E-16));
#78881=CARTESIAN_POINT('Ctrl Pts',(7.42081956607134,-0.827896490427196,
-1.45086831496663E-15));
#78882=CARTESIAN_POINT('Ctrl Pts',(7.42551437130127,-0.629371956630587,
1.87479693411711E-15));
#78883=CARTESIAN_POINT('Ctrl Pts',(7.42235848357616,-0.431206060649004,
3.19189119579733E-15));
#78884=CARTESIAN_POINT('Ctrl Pts',(7.41922110448639,-0.234202367072023,
4.50126096931357E-15));
#78885=CARTESIAN_POINT('Ctrl Pts',(7.40832471147218,-0.0375524031725907,
-2.23129519337553E-15));
#78886=CARTESIAN_POINT('Ctrl Pts',(7.38965476442135,0.158275945628522,-1.30451205393456E-15));
#78887=CARTESIAN_POINT('Ctrl Pts',(7.37081960531058,0.355837197303689,-3.69527726178446E-16));
#78888=CARTESIAN_POINT('Ctrl Pts',(7.34407270537559,0.552562969772611,-9.04532103063896E-15));
#78889=CARTESIAN_POINT('Ctrl Pts',(7.30934707767143,0.747957904919255,-1.04916075827077E-14));
#78890=CARTESIAN_POINT('Ctrl Pts',(7.27462144996726,0.943352840065898,-1.19378941347765E-14));
#78891=CARTESIAN_POINT('Ctrl Pts',(7.231917026481,1.13741766010537,-9.36028213032184E-15));
#78892=CARTESIAN_POINT('Ctrl Pts',(7.18111561966283,1.32963115094122,-1.04638520070921E-14));
#78893=CARTESIAN_POINT('Ctrl Pts',(7.17837256944882,1.34000982527717,-1.04344473399599E-14));
#78894=CARTESIAN_POINT('Ctrl Pts',(7.17560590005785,1.35038309419168,-8.87834579902764E-15));
#78895=CARTESIAN_POINT('Ctrl Pts',(7.17281558869492,1.36075087284441,-9.57567358739198E-15));
#78896=CARTESIAN_POINT('Ctrl Pts',(7.14346945585713,1.46979039209583,-1.09940822433459E-14));
#78897=CARTESIAN_POINT('Ctrl Pts',(7.11150861106633,1.57822295528145,-1.49401620285407E-15));
#78898=CARTESIAN_POINT('Ctrl Pts',(7.07696325132472,1.68595868374967,-1.19626530903361E-14));
#78899=CARTESIAN_POINT('Ctrl Pts',(7.06510387588707,1.72294421412221,-9.56354954911704E-15));
#78900=CARTESIAN_POINT('Ctrl Pts',(7.05293843640282,1.7598514332514,-1.40814083866707E-14));
#78901=CARTESIAN_POINT('Ctrl Pts',(7.04047968047903,1.796643391524,-1.33226762955019E-14));
#78902=CARTESIAN_POINT('Ctrl Pts',(6.97810874276675,1.98083103849048,-9.52431694982914E-15));
#78903=CARTESIAN_POINT('Ctrl Pts',(6.90833674176368,2.16230548123818,-2.00936910819825E-14));
#78904=CARTESIAN_POINT('Ctrl Pts',(6.83140645991705,2.3406495722722,-1.18377530000657E-14));
#78905=CARTESIAN_POINT('Ctrl Pts',(6.7547604043449,2.5183347540269,-3.61231726997968E-15));
#78906=CARTESIAN_POINT('Ctrl Pts',(6.67100842573644,2.69291325589164,-1.08516979078709E-14));
#78907=CARTESIAN_POINT('Ctrl Pts',(6.58034816210955,2.86394370118305,-8.18789480661053E-15));
#78908=CARTESIAN_POINT('Ctrl Pts',(6.5107253472596,2.99528703231687,-6.1422194170154E-15));
#78909=CARTESIAN_POINT('Ctrl Pts',(6.43702745650996,3.12453738507979,1.75858176966081E-14));
#78910=CARTESIAN_POINT('Ctrl Pts',(6.35932929176472,3.25148000052063,3.38618022510673E-15));
#78911=CARTESIAN_POINT('Ctrl Pts',(6.34415551430166,3.27627079195817,7.2328019561982E-15));
#78912=CARTESIAN_POINT('Ctrl Pts',(6.32882961100114,3.30097264814734,1.79741789374078E-15));
#78913=CARTESIAN_POINT('Ctrl Pts',(6.31335914601642,3.3255730433318,4.9960036108132E-16));
#78914=CARTESIAN_POINT('Ctrl Pts',(6.21150098685578,3.48754302746538,5.53132638240168E-15));
#78915=CARTESIAN_POINT('Ctrl Pts',(6.10330153910545,3.64524546448351,6.66685612455958E-15));
#78916=CARTESIAN_POINT('Ctrl Pts',(5.98896545356102,3.79825919093505,4.9960036108132E-15));
#78917=CARTESIAN_POINT('Ctrl Pts',(5.87621798675758,3.94914690028266,1.33293757130128E-14));
#78918=CARTESIAN_POINT('Ctrl Pts',(5.75750276055192,4.09547574709246,-2.11923734512429E-15));
#78919=CARTESIAN_POINT('Ctrl Pts',(5.63298215922921,4.23680466115335,-8.91647866652079E-16));
#78920=CARTESIAN_POINT('Ctrl Pts',(5.56848507749013,4.31000782934764,-2.55801764930648E-16));
#78921=CARTESIAN_POINT('Ctrl Pts',(5.50242998150509,4.38186893166116,5.78872423977802E-15));
#78922=CARTESIAN_POINT('Ctrl Pts',(5.43483639892989,4.4523220498536,6.67695065903473E-15));
#78923=CARTESIAN_POINT('Ctrl Pts',(5.39406123916706,4.49482219617873,6.59768912781167E-15));
#78924=CARTESIAN_POINT('Ctrl Pts',(5.35272618362371,4.53680991131998,5.15696403806271E-15));
#78925=CARTESIAN_POINT('Ctrl Pts',(5.31084235969185,4.57827599247481,6.81887272341308E-15));
#78926=CARTESIAN_POINT('Ctrl Pts',(5.31037376991264,4.57794244025893,20.));
#78927=CARTESIAN_POINT('Ctrl Pts',(5.44258499059786,4.44692576935788,20.));
#78928=CARTESIAN_POINT('Ctrl Pts',(5.56920635744265,4.3107893129539,20.));
#78929=CARTESIAN_POINT('Ctrl Pts',(5.69011135105436,4.17000439600832,20.));
#78930=CARTESIAN_POINT('Ctrl Pts',(5.81400769402978,4.02573627411689,20.));
#78931=CARTESIAN_POINT('Ctrl Pts',(5.9319017845614,3.87658649463656,20.));
#78932=CARTESIAN_POINT('Ctrl Pts',(6.04363170607624,3.7230137251186,20.));
#78933=CARTESIAN_POINT('Ctrl Pts',(6.1562476207376,3.56822315808105,20.));
#78934=CARTESIAN_POINT('Ctrl Pts',(6.26260167109238,3.40893866919477,20.));
#78935=CARTESIAN_POINT('Ctrl Pts',(6.36249517847558,3.24558783962327,20.));
#78936=CARTESIAN_POINT('Ctrl Pts',(6.46242012910578,3.08218559249104,20.));
#78937=CARTESIAN_POINT('Ctrl Pts',(6.55588089924594,2.91471387316095,20.));
#78938=CARTESIAN_POINT('Ctrl Pts',(6.6426392681944,2.74356691388431,20.));
#78939=CARTESIAN_POINT('Ctrl Pts',(6.70659897553043,2.61739453928274,20.));
#78940=CARTESIAN_POINT('Ctrl Pts',(6.76691522639903,2.48922397464942,20.));
#78941=CARTESIAN_POINT('Ctrl Pts',(6.82347677867138,2.35920420123498,20.));
#78942=CARTESIAN_POINT('Ctrl Pts',(6.83289078394379,2.33756393884352,20.));
#78943=CARTESIAN_POINT('Ctrl Pts',(6.84220167879346,2.31587022651507,20.));
#78944=CARTESIAN_POINT('Ctrl Pts',(6.85140588189888,2.29413090399489,20.));
#78945=CARTESIAN_POINT('Ctrl Pts',(6.92787028024333,2.11353034598004,20.));
#78946=CARTESIAN_POINT('Ctrl Pts',(6.99681396504024,1.93016810899366,20.));
#78947=CARTESIAN_POINT('Ctrl Pts',(7.05806564428657,1.74450976178054,20.));
#78948=CARTESIAN_POINT('Ctrl Pts',(7.08071894120841,1.67584595178894,20.));
#78949=CARTESIAN_POINT('Ctrl Pts',(7.10231976439282,1.60686769755636,20.));
#78950=CARTESIAN_POINT('Ctrl Pts',(7.12285814961541,1.53759730827682,20.));
#78951=CARTESIAN_POINT('Ctrl Pts',(7.17789437546803,1.35197508199331,20.));
#78952=CARTESIAN_POINT('Ctrl Pts',(7.22530500077645,1.16425705287924,20.));
#78953=CARTESIAN_POINT('Ctrl Pts',(7.2651668680032,0.974923813898792,20.));
#78954=CARTESIAN_POINT('Ctrl Pts',(7.30539082871382,0.78387072743286,20.));
#78955=CARTESIAN_POINT('Ctrl Pts',(7.33792842648121,0.591172314156727,20.));
#78956=CARTESIAN_POINT('Ctrl Pts',(7.36281005306225,0.397300196653284,20.));
#78957=CARTESIAN_POINT('Ctrl Pts',(7.38777115856543,0.202808797010905,20.));
#78958=CARTESIAN_POINT('Ctrl Pts',(7.40502742979251,0.00713548946427733,
20.));
#78959=CARTESIAN_POINT('Ctrl Pts',(7.41455881759031,-0.189255710324768,
20.));
#78960=CARTESIAN_POINT('Ctrl Pts',(7.41891526848925,-0.279018988980004,
20.));
#78961=CARTESIAN_POINT('Ctrl Pts',(7.421657226845,-0.368932343342073,20.));
#78962=CARTESIAN_POINT('Ctrl Pts',(7.42277915309801,-0.458951694386215,
20.));
#78963=CARTESIAN_POINT('Ctrl Pts',(7.42308605705979,-0.483576570930439,
20.));
#78964=CARTESIAN_POINT('Ctrl Pts',(7.42327160494634,-0.508201841411565,
20.));
#78965=CARTESIAN_POINT('Ctrl Pts',(7.42333592375777,-0.532819998670914,
20.));
#78966=CARTESIAN_POINT('Ctrl Pts',(7.42385714235562,-0.732317488160773,
20.));
#78967=CARTESIAN_POINT('Ctrl Pts',(7.41642303419139,-0.93148134030672,20.));
#78968=CARTESIAN_POINT('Ctrl Pts',(7.40111949060241,-1.12981386430432,20.));
#78969=CARTESIAN_POINT('Ctrl Pts',(7.38567034974055,-1.33003331563027,20.));
#78970=CARTESIAN_POINT('Ctrl Pts',(7.36220146956873,-1.52940623904774,20.));
#78971=CARTESIAN_POINT('Ctrl Pts',(7.33075071423941,-1.72743673897839,20.));
#78972=CARTESIAN_POINT('Ctrl Pts',(7.30904615534814,-1.86410005923912,20.));
#78973=CARTESIAN_POINT('Ctrl Pts',(7.28353913344292,-2.00012438495812,20.));
#78974=CARTESIAN_POINT('Ctrl Pts',(7.25422772630418,-2.13534847915567,20.));
#78975=CARTESIAN_POINT('Ctrl Pts',(7.21189212614094,-2.33065787379803,20.));
#78976=CARTESIAN_POINT('Ctrl Pts',(7.16162247429041,-2.52429848791992,20.));
#78977=CARTESIAN_POINT('Ctrl Pts',(7.10366596787394,-2.71587264560239,20.));
#78978=CARTESIAN_POINT('Ctrl Pts',(7.0459594755488,-2.90662038634025,20.));
#78979=CARTESIAN_POINT('Ctrl Pts',(6.98063203506653,-3.09532008764642,20.));
#78980=CARTESIAN_POINT('Ctrl Pts',(6.90787782849201,-3.28156683212074,20.));
#78981=CARTESIAN_POINT('Ctrl Pts',(6.89581151404611,-3.31245592966111,20.));
#78982=CARTESIAN_POINT('Ctrl Pts',(6.88353870682705,-3.34328252123178,20.));
#78983=CARTESIAN_POINT('Ctrl Pts',(6.87107234116059,-3.37401523348661,20.));
#78984=CARTESIAN_POINT('Ctrl Pts',(6.79527663912565,-3.56087061404549,20.));
#78985=CARTESIAN_POINT('Ctrl Pts',(6.71226278618979,-3.74443472774651,20.));
#78986=CARTESIAN_POINT('Ctrl Pts',(6.62235335551551,-3.92432447229519,20.));
#78987=CARTESIAN_POINT('Ctrl Pts',(6.53088269512199,-4.10733790713164,20.));
#78988=CARTESIAN_POINT('Ctrl Pts',(6.4322747831017,-4.28654890171632,20.));
#78989=CARTESIAN_POINT('Ctrl Pts',(6.32681586246644,-4.46154936748218,20.));
#78990=CARTESIAN_POINT('Ctrl Pts',(6.22105095057789,-4.63705760074199,20.));
#78991=CARTESIAN_POINT('Ctrl Pts',(6.10839496565391,-4.80833150317585,20.));
#78992=CARTESIAN_POINT('Ctrl Pts',(5.98908635398953,-4.9749448495409,20.));
#78993=CARTESIAN_POINT('Ctrl Pts',(5.87055983530591,-5.14046601046456,20.));
#78994=CARTESIAN_POINT('Ctrl Pts',(5.74546730794022,-5.30138815195256,20.));
#78995=CARTESIAN_POINT('Ctrl Pts',(5.61399733100531,-5.45726932553109,20.));
#78996=CARTESIAN_POINT('Ctrl Pts',(5.59056995179115,-5.48504667402474,20.));
#78997=CARTESIAN_POINT('Ctrl Pts',(5.56693995540417,-5.51266387690693,20.));
#78998=CARTESIAN_POINT('Ctrl Pts',(5.54310826839702,-5.54011832860014,20.));
#78999=CARTESIAN_POINT('Ctrl Pts',(5.48873752541245,-5.60275421905749,20.));
#79000=CARTESIAN_POINT('Ctrl Pts',(5.4333170502013,-5.66454305419315,20.));
#79001=CARTESIAN_POINT('Ctrl Pts',(5.37687176772693,-5.72546775434948,20.));
#79002=CARTESIAN_POINT('Ctrl Pts',(5.34692970249771,-5.75778597947273,20.));
#79003=CARTESIAN_POINT('Ctrl Pts',(5.31669957407756,-5.78986069271576,20.));
#79004=CARTESIAN_POINT('Ctrl Pts',(5.28618389754254,-5.82169036550656,20.));
#79005=CARTESIAN_POINT('Ctrl Pts',(5.26222541995964,-5.8466804882441,20.));
#79006=CARTESIAN_POINT('Ctrl Pts',(5.23809317649021,-5.87151706999867,20.));
#79007=CARTESIAN_POINT('Ctrl Pts',(5.21380409728959,-5.8961838900846,20.));
#79008=CARTESIAN_POINT('Ctrl Pts',(5.06917294826217,-6.04306432562574,20.));
#79009=CARTESIAN_POINT('Ctrl Pts',(4.91885274484368,-6.18406632260094,20.));
#79010=CARTESIAN_POINT('Ctrl Pts',(4.76330525902998,-6.31898881110124,20.));
#79011=CARTESIAN_POINT('Ctrl Pts',(4.60608464123105,-6.4553625807319,20.));
#79012=CARTESIAN_POINT('Ctrl Pts',(4.44352323643732,-6.58552582901827,20.));
#79013=CARTESIAN_POINT('Ctrl Pts',(4.27605405044702,-6.70924078257424,20.));
#79014=CARTESIAN_POINT('Ctrl Pts',(4.18911861719913,-6.77346282451606,20.));
#79015=CARTESIAN_POINT('Ctrl Pts',(4.10085996926207,-6.83594665435447,20.));
#79016=CARTESIAN_POINT('Ctrl Pts',(4.01133472131358,-6.89665519792269,20.));
#79017=CARTESIAN_POINT('Ctrl Pts',(3.96858583980601,-6.92564391780859,20.));
#79018=CARTESIAN_POINT('Ctrl Pts',(3.92554812122795,-6.95422780963465,20.));
#79019=CARTESIAN_POINT('Ctrl Pts',(3.88222753925519,-6.98240260462403,20.));
#79020=CARTESIAN_POINT('Ctrl Pts',(3.83688314264079,-7.01189364607243,20.));
#79021=CARTESIAN_POINT('Ctrl Pts',(3.79122247495776,-7.04094023216963,20.));
#79022=CARTESIAN_POINT('Ctrl Pts',(3.74529296566859,-7.06951255916912,20.));
#79023=CARTESIAN_POINT('Ctrl Pts',(3.66342765985698,-7.12044021600156,20.));
#79024=CARTESIAN_POINT('Ctrl Pts',(3.5806901914544,-7.16987375606264,20.));
#79025=CARTESIAN_POINT('Ctrl Pts',(3.49712247540394,-7.21779315037648,20.));
#79026=CARTESIAN_POINT('Ctrl Pts',(3.30484647767293,-7.32804804051606,20.));
#79027=CARTESIAN_POINT('Ctrl Pts',(3.10818162093266,-7.43028820260646,20.));
#79028=CARTESIAN_POINT('Ctrl Pts',(2.90763049540401,-7.524222843759,20.));
#79029=CARTESIAN_POINT('Ctrl Pts',(2.70707936987535,-7.61815748491155,20.));
#79030=CARTESIAN_POINT('Ctrl Pts',(2.50264126591493,-7.70378717616298,20.));
#79031=CARTESIAN_POINT('Ctrl Pts',(2.2947819056922,-7.78077036713514,20.));
#79032=CARTESIAN_POINT('Ctrl Pts',(2.23095378491342,-7.80440987226034,20.));
#79033=CARTESIAN_POINT('Ctrl Pts',(2.16680283827967,-7.82723366713653,20.));
#79034=CARTESIAN_POINT('Ctrl Pts',(2.10234503241322,-7.84924105753589,20.));
#79035=CARTESIAN_POINT('Ctrl Pts',(5.31040305176835,4.57790847333905,-0.000178101097112471));
#79036=CARTESIAN_POINT('Ctrl Pts',(5.30882975752663,4.57973350470244,-0.00011873406474153));
#79037=CARTESIAN_POINT('Ctrl Pts',(5.30725552246937,4.58155772502242,-5.93670323709406E-5));
#79038=CARTESIAN_POINT('Ctrl Pts',(5.30568034743329,4.58338113332943,0.));
#79039=CARTESIAN_POINT('Ctrl Pts',(-2.10222011176618,-7.84913218468459,
19.999697384906));
#79040=CARTESIAN_POINT('Ctrl Pts',(-3.40743872906296,-7.49955763771916,
19.9467661843935));
#79041=CARTESIAN_POINT('Ctrl Pts',(-5.83879819321471,-6.13705586876475,
19.8409037833685));
#79042=CARTESIAN_POINT('Ctrl Pts',(-8.063328137307,-2.59492553977183,19.6821101818309));
#79043=CARTESIAN_POINT('Ctrl Pts',(-8.32211031922223,1.57870274228667,19.5233165802935));
#79044=CARTESIAN_POINT('Ctrl Pts',(-6.55256548103476,5.3680183485327,19.3645229787559));
#79045=CARTESIAN_POINT('Ctrl Pts',(-3.18576426764331,7.8486441896436,19.2057293772185));
#79046=CARTESIAN_POINT('Ctrl Pts',(0.957516033830517,8.41630867132718,19.0469357756809));
#79047=CARTESIAN_POINT('Ctrl Pts',(4.8674260860221,6.93245445843938,18.8881421741434));
#79048=CARTESIAN_POINT('Ctrl Pts',(7.59090189466519,3.75886426572798,18.7293485726058));
#79049=CARTESIAN_POINT('Ctrl Pts',(8.46411978115432,-0.330956437631908,
18.5705549710684));
#79050=CARTESIAN_POINT('Ctrl Pts',(7.27422648106118,-4.34009886765195,18.4117613695308));
#79051=CARTESIAN_POINT('Ctrl Pts',(4.31125990388258,-7.2913572173132,18.2529677679934));
#79052=CARTESIAN_POINT('Ctrl Pts',(0.297433621833983,-8.46536305708804,
18.0941741664558));
#79053=CARTESIAN_POINT('Ctrl Pts',(-3.78889099106759,-7.57595866543456,
17.9353805649183));
#79054=CARTESIAN_POINT('Ctrl Pts',(-6.95168297254158,-4.8399324863166,17.7765869633808));
#79055=CARTESIAN_POINT('Ctrl Pts',(-8.42001929378617,-0.924185001110069,
17.6177933618432));
#79056=CARTESIAN_POINT('Ctrl Pts',(-7.83599675007498,3.21683044313197,17.4589997603057));
#79057=CARTESIAN_POINT('Ctrl Pts',(-5.34196931903587,6.57375133412712,17.3002061587682));
#79058=CARTESIAN_POINT('Ctrl Pts',(-1.54585006801036,8.32833660506733,17.1414125572307));
#79059=CARTESIAN_POINT('Ctrl Pts',(2.62706632719926,8.05291037069421,16.9826189556932));
#79060=CARTESIAN_POINT('Ctrl Pts',(6.15964178765682,5.81460712479525,16.8238253541557));
#79061=CARTESIAN_POINT('Ctrl Pts',(8.19081977136801,2.15900774267334,16.6650317526181));
#79062=CARTESIAN_POINT('Ctrl Pts',(8.22550565692099,-2.02284444389487,16.5062381510806));
#79063=CARTESIAN_POINT('Ctrl Pts',(6.25524484665678,-5.71163329267625,16.3474445495431));
#79064=CARTESIAN_POINT('Ctrl Pts',(2.76028354811421,-8.00822562692782,16.1886509480056));
#79065=CARTESIAN_POINT('Ctrl Pts',(-1.40749005041534,-8.35283273613254,
16.0298573464681));
#79066=CARTESIAN_POINT('Ctrl Pts',(-5.23219142410912,-6.66145748770267,
15.8710637449305));
#79067=CARTESIAN_POINT('Ctrl Pts',(-7.7815590556908,-3.34636842293283,15.712270143393));
#79068=CARTESIAN_POINT('Ctrl Pts',(-8.43419087903681,0.784389683258458,
15.5534765418555));
#79069=CARTESIAN_POINT('Ctrl Pts',(-7.03100949843993,4.72395474068076,15.394682940318));
#79070=CARTESIAN_POINT('Ctrl Pts',(-3.91403691117488,7.51206749285283,15.2358893387805));
#79071=CARTESIAN_POINT('Ctrl Pts',(0.156972509984872,8.46913233987333,15.077095737243));
#79072=CARTESIAN_POINT('Ctrl Pts',(4.18972026937783,7.36186708814822,14.9183021357054));
#79073=CARTESIAN_POINT('Ctrl Pts',(7.20123405694,4.46016490909898,14.7595085341679));
#79074=CARTESIAN_POINT('Ctrl Pts',(8.45746482195596,0.471308544976929,14.6007149326304));
#79075=CARTESIAN_POINT('Ctrl Pts',(7.65220941691035,-3.63242811338918,14.4419213310929));
#79076=CARTESIAN_POINT('Ctrl Pts',(4.98174685872065,-6.85076938707017,14.2831277295554));
#79077=CARTESIAN_POINT('Ctrl Pts',(1.09699580294953,-8.39925253623812,14.1243341280179));
#79078=CARTESIAN_POINT('Ctrl Pts',(-3.05514527146234,-7.90043861627013,
13.9655405264804));
#79079=CARTESIAN_POINT('Ctrl Pts',(-6.46260222867888,-5.47591228865712,
13.8067469249428));
#79080=CARTESIAN_POINT('Ctrl Pts',(-8.2948158479101,-1.71664585994049,13.6479533234053));
#79081=CARTESIAN_POINT('Ctrl Pts',(-8.10518858294586,2.46104875897965,13.4891597218678));
#79082=CARTESIAN_POINT('Ctrl Pts',(-5.93994161145822,6.03886881888142,13.3303661203303));
#79083=CARTESIAN_POINT('Ctrl Pts',(-2.32684853705731,8.14472951329788,13.1715725187928));
#79084=CARTESIAN_POINT('Ctrl Pts',(1.85340812358983,8.2653324970386,13.0127789172552));
#79085=CARTESIAN_POINT('Ctrl Pts',(5.58190112991571,6.37128109056859,12.8539853157177));
#79086=CARTESIAN_POINT('Ctrl Pts',(7.94981951675275,2.92424564806863,12.6951917141802));
#79087=CARTESIAN_POINT('Ctrl Pts',(8.3799890233666,-1.23556745159722,12.5363981126427));
#79088=CARTESIAN_POINT('Ctrl Pts',(6.76755689454807,-5.09421403537837,12.3776045111052));
#79089=CARTESIAN_POINT('Ctrl Pts',(3.50554948082876,-7.71115852493337,12.2188109095677));
#79090=CARTESIAN_POINT('Ctrl Pts',(-0.610926964134399,-8.44852716180073,
12.0600173080301));
#79091=CARTESIAN_POINT('Ctrl Pts',(-4.57849146988245,-7.12658816120343,
11.9012237064926));
#79092=CARTESIAN_POINT('Ctrl Pts',(-7.43005998349757,-4.06756089085575,
11.7424301049551));
#79093=CARTESIAN_POINT('Ctrl Pts',(-8.47056971990735,-0.0170756955972321,
11.5836365034176));
#79094=CARTESIAN_POINT('Ctrl Pts',(-7.44639899973391,4.03757165830562,11.4248429018801));
#79095=CARTESIAN_POINT('Ctrl Pts',(-4.60718690748627,7.10807088869254,11.2660493003426));
#79096=CARTESIAN_POINT('Ctrl Pts',(-0.644984381034744,8.44599538878707,
11.107255698805));
#79097=CARTESIAN_POINT('Ctrl Pts',(3.47443149591835,7.72522936483841,10.9484620972675));
#79098=CARTESIAN_POINT('Ctrl Pts',(6.74696327362364,5.1214577557142,10.78966849573));
#79099=CARTESIAN_POINT('Ctrl Pts',(8.37493941068567,1.26934346279288,10.6308748941925));
#79100=CARTESIAN_POINT('Ctrl Pts',(7.96154474293954,-2.89217016535385,10.472081292655));
#79101=CARTESIAN_POINT('Ctrl Pts',(5.60754320003511,-6.34872445605661,10.3132876911175));
#79102=CARTESIAN_POINT('Ctrl Pts',(1.88671684635692,-8.2577928347025,10.1544940895799));
#79103=CARTESIAN_POINT('Ctrl Pts',(-2.29399208058248,-8.15404459721776,
9.99570048804245));
#79104=CARTESIAN_POINT('Ctrl Pts',(-5.91554610142342,-6.06276812034943,
9.83690688650493));
#79105=CARTESIAN_POINT('Ctrl Pts',(-8.09520036469299,-2.49370688226696,
9.67811328496741));
#79106=CARTESIAN_POINT('Ctrl Pts',(-8.30166952497879,1.68318925175681,9.5193196834299));
#79107=CARTESIAN_POINT('Ctrl Pts',(-6.48462723420443,5.4498121612222,9.36052608189237));
#79108=CARTESIAN_POINT('Ctrl Pts',(-3.08697306472453,7.88805681120873,9.20173248035486));
#79109=CARTESIAN_POINT('Ctrl Pts',(1.06312316798005,8.40360708796499,9.04293887881735));
#79110=CARTESIAN_POINT('Ctrl Pts',(4.95408575319091,6.87079888435267,8.88414527727982));
#79111=CARTESIAN_POINT('Ctrl Pts',(7.63750216700183,3.66325041571465,8.72535167574231));
#79112=CARTESIAN_POINT('Ctrl Pts',(8.45929628352375,-0.437206297704228,
8.56655807420478));
#79113=CARTESIAN_POINT('Ctrl Pts',(7.2191578157485,-4.43109505545849,8.40776447266728));
#79114=CARTESIAN_POINT('Ctrl Pts',(4.21936745346892,-7.34491533319468,8.24897087112975));
#79115=CARTESIAN_POINT('Ctrl Pts',(0.191116691430598,-8.46843063202667,
8.09017726959224));
#79116=CARTESIAN_POINT('Ctrl Pts',(-3.88371829230374,-7.52778687166532,
7.93138366805473));
#79117=CARTESIAN_POINT('Ctrl Pts',(-7.01190653064279,-4.75226364638159,
7.7725900665172));
#79118=CARTESIAN_POINT('Ctrl Pts',(-8.43095986354782,-0.818387889962332,
7.61379646497969));
#79119=CARTESIAN_POINT('Ctrl Pts',(-7.79498754456611,3.31496789415078,7.45500286344217));
#79120=CARTESIAN_POINT('Ctrl Pts',(-5.25900625632336,6.64030843825366,7.29620926190465));
#79121=CARTESIAN_POINT('Ctrl Pts',(-1.44115517684792,8.34709019451903,7.13741566036713));
#79122=CARTESIAN_POINT('Ctrl Pts',(2.72797391897493,8.01928932366103,6.97862205882962));
#79123=CARTESIAN_POINT('Ctrl Pts',(6.23216610703123,5.73680647865712,6.8198284572921));
#79124=CARTESIAN_POINT('Ctrl Pts',(8.21728319283949,2.05599121784817,6.66103485575458));
#79125=CARTESIAN_POINT('Ctrl Pts',(8.19945778770858,-2.12596682635838,6.50224125421707));
#79126=CARTESIAN_POINT('Ctrl Pts',(6.18303479013073,-5.7897257053529,6.34344765267954));
#79127=CARTESIAN_POINT('Ctrl Pts',(2.65951232750101,-8.04225323768542,6.18465405114204));
#79128=CARTESIAN_POINT('Ctrl Pts',(-1.51225969899553,-8.33450139852319,
6.02586044960451));
#79129=CARTESIAN_POINT('Ctrl Pts',(-5.3154221574182,-6.59523542018167,5.867066848067));
#79130=CARTESIAN_POINT('Ctrl Pts',(-7.82296358799924,-3.24839709087868,
5.70827324652947));
#79131=CARTESIAN_POINT('Ctrl Pts',(-8.42367695780134,0.890230009490827,
5.54947964499197));
#79132=CARTESIAN_POINT('Ctrl Pts',(-6.97113986601195,4.81186574289953,5.39068604345444));
#79133=CARTESIAN_POINT('Ctrl Pts',(-3.81940464264517,7.56062108129564,5.23189244191693));
#79134=CARTESIAN_POINT('Ctrl Pts',(0.263301032793999,8.46649369723502,5.07309884037941));
#79135=CARTESIAN_POINT('Ctrl Pts',(4.28182773154276,7.30867937705459,4.9143052388419));
#79136=CARTESIAN_POINT('Ctrl Pts',(7.25666949195797,4.36939250281743,4.75551163730438));
#79137=CARTESIAN_POINT('Ctrl Pts',(8.46271597940375,0.365076993433917,4.59671803576686));
#79138=CARTESIAN_POINT('Ctrl Pts',(7.60599634012455,-3.7282251317762,4.43792443422934));
#79139=CARTESIAN_POINT('Ctrl Pts',(4.89533387107377,-6.91278158557734,4.27913083269182));
#79140=CARTESIAN_POINT('Ctrl Pts',(0.991445856839866,-8.41236459458163,
4.12033723115431));
#79141=CARTESIAN_POINT('Ctrl Pts',(-3.15410463726016,-7.8614545025947,3.96154362961679));
#79142=CARTESIAN_POINT('Ctrl Pts',(-6.53084991306519,-5.39433428443648,
3.80275002807927));
#79143=CARTESIAN_POINT('Ctrl Pts',(-8.31571664631593,-1.61235840227592,
3.64395642654176));
#79144=CARTESIAN_POINT('Ctrl Pts',(-8.07364797734855,2.56262585970849,3.48516282500424));
#79145=CARTESIAN_POINT('Ctrl Pts',(-5.86364754662715,6.11297639523982,3.32636922346672));
#79146=CARTESIAN_POINT('Ctrl Pts',(-2.22439750288786,8.17330402633597,3.16757562192921));
#79147=CARTESIAN_POINT('Ctrl Pts',(1.957043940362,8.24140898009109,3.00878202039168));
#79148=CARTESIAN_POINT('Ctrl Pts',(5.66146075499942,6.3006908411568,2.84998841885417));
#79149=CARTESIAN_POINT('Ctrl Pts',(7.98591048759216,2.8241948665278,2.69119481731665));
#79150=CARTESIAN_POINT('Ctrl Pts',(8.36381425563696,-1.34069163686942,2.53240121577913));
#79151=CARTESIAN_POINT('Ctrl Pts',(6.7030589465472,-5.17878785866461,2.37360761424162));
#79152=CARTESIAN_POINT('Ctrl Pts',(3.40844957090335,-7.75456733562105,2.2148140127041));
#79153=CARTESIAN_POINT('Ctrl Pts',(-0.716960978086715,-8.44019014977505,
2.05602041116658));
#79154=CARTESIAN_POINT('Ctrl Pts',(-4.66761404808927,-7.06853749124428,
1.89722680962907));
#79155=CARTESIAN_POINT('Ctrl Pts',(-7.480547738494,-3.97394619441689,1.73843320809155));
#79156=CARTESIAN_POINT('Ctrl Pts',(-8.47011634489816,0.0892845267466103,
1.57963960655403));
#79157=CARTESIAN_POINT('Ctrl Pts',(-7.39511508466361,4.13075265867455,1.42084600501651));
#79158=CARTESIAN_POINT('Ctrl Pts',(-4.51757262101829,7.16535945096504,1.262052403479));
#79159=CARTESIAN_POINT('Ctrl Pts',(-0.53888329681407,8.45342870211286,1.10325880194148));
#79160=CARTESIAN_POINT('Ctrl Pts',(3.57115811491559,7.68099334702474,0.944465200403969));
#79161=CARTESIAN_POINT('Ctrl Pts',(6.81073734528766,5.03633921085957,0.785671598866447));
#79162=CARTESIAN_POINT('Ctrl Pts',(8.39021853594661,1.16408120921888,0.626877997328932));
#79163=CARTESIAN_POINT('Ctrl Pts',(7.92460000763248,-2.9919017765053,0.468084395791413));
#79164=CARTESIAN_POINT('Ctrl Pts',(5.52738896171523,-6.41864938067256,0.309290794253898));
#79165=CARTESIAN_POINT('Ctrl Pts',(1.78287247840694,-8.28080161037312,0.150497192716378));
#79166=CARTESIAN_POINT('Ctrl Pts',(-2.39617932800353,-8.12465753133514,
-0.00829640882114185));
#79167=CARTESIAN_POINT('Ctrl Pts',(-5.99123816337043,-5.9878951045908,-0.167090010358655));
#79168=CARTESIAN_POINT('Ctrl Pts',(-8.1258084234525,-2.39209880067588,-0.325883611896176));
#79169=CARTESIAN_POINT('Ctrl Pts',(-8.28003535986636,1.78802420893543,-0.484686260456206));
#79170=CARTESIAN_POINT('Ctrl Pts',(-7.03657972594842,4.28266391599147,-0.590557708503744));
#79171=CARTESIAN_POINT('Ctrl Pts',(-6.15407036887642,5.3061872692741,-0.64349795603877));
#79172=CARTESIAN_POINT('Ctrl Pts',(-2.00604353560581,-7.49003436465715,
20.2143297668606));
#79173=CARTESIAN_POINT('Ctrl Pts',(-3.25154839740679,-7.15645285422094,
20.1613985663481));
#79174=CARTESIAN_POINT('Ctrl Pts',(-5.57167315907976,-5.85628554511544,
20.0555361653231));
#79175=CARTESIAN_POINT('Ctrl Pts',(-7.69443085183093,-2.47620768886292,
19.8967425637855));
#79176=CARTESIAN_POINT('Ctrl Pts',(-7.94137374817917,1.5064770872859,19.737948962248));
#79177=CARTESIAN_POINT('Ctrl Pts',(-6.25278559142888,5.12243149364616,19.5791553607105));
#79178=CARTESIAN_POINT('Ctrl Pts',(-3.04001554323474,7.48956869539067,19.420361759173));
#79179=CARTESIAN_POINT('Ctrl Pts',(0.913709672528465,8.03126252540434,19.2615681576355));
#79180=CARTESIAN_POINT('Ctrl Pts',(4.64474132858538,6.61529464702449,19.102774556098));
#79181=CARTESIAN_POINT('Ctrl Pts',(7.24361811114894,3.58689621475851,18.9439809545604));
#79182=CARTESIAN_POINT('Ctrl Pts',(8.07688627681936,-0.315815179658241,
18.7851873530229));
#79183=CARTESIAN_POINT('Ctrl Pts',(6.94143059862823,-4.14153933197253,18.6263937514854));
#79184=CARTESIAN_POINT('Ctrl Pts',(4.11401975087856,-6.95777760364743,18.4676001499479));
#79185=CARTESIAN_POINT('Ctrl Pts',(0.283826032779512,-8.07807267287554,
18.3088065484104));
#79186=CARTESIAN_POINT('Ctrl Pts',(-3.61554921732747,-7.22935853469858,
18.1500129468728));
#79187=CARTESIAN_POINT('Ctrl Pts',(-6.63364345655119,-4.61850556114549,
17.9912193453353));
#79188=CARTESIAN_POINT('Ctrl Pts',(-8.03480338687517,-0.881903534650851,
17.8324257437978));
#79189=CARTESIAN_POINT('Ctrl Pts',(-7.47749987621871,3.06966044110543,17.6736321422603));
#79190=CARTESIAN_POINT('Ctrl Pts',(-5.09757420732374,6.27300219168134,17.5148385407228));
#79191=CARTESIAN_POINT('Ctrl Pts',(-1.47512742295223,7.94731518142893,17.3560449391853));
#79192=CARTESIAN_POINT('Ctrl Pts',(2.5068780351731,7.68448969807065,17.1972513376478));
#79193=CARTESIAN_POINT('Ctrl Pts',(5.87783815815324,5.54858883211008,17.0384577361102));
#79194=CARTESIAN_POINT('Ctrl Pts',(7.81608974326692,2.06023313223562,16.8796641345727));
#79195=CARTESIAN_POINT('Ctrl Pts',(7.84918874945609,-1.93029930476795,16.7208705330352));
#79196=CARTESIAN_POINT('Ctrl Pts',(5.96906737692894,-5.45032605310672,16.5620769314977));
#79197=CARTESIAN_POINT('Ctrl Pts',(2.634000567848,-7.64184928146013,16.4032833299602));
#79198=CARTESIAN_POINT('Ctrl Pts',(-1.34309737656017,-7.97069061442744,
16.2444897284227));
#79199=CARTESIAN_POINT('Ctrl Pts',(-4.99281865140567,-6.35669578847852,
16.0856961268851));
#79200=CARTESIAN_POINT('Ctrl Pts',(-7.4255527065092,-3.19327205795779,15.9269025253476));
#79201=CARTESIAN_POINT('Ctrl Pts',(-8.04832662205982,0.748503852993082,
15.7681089238101));
#79202=CARTESIAN_POINT('Ctrl Pts',(-6.70934079366152,4.5078337977061,15.6093153222726));
#79203=CARTESIAN_POINT('Ctrl Pts',(-3.73496971122986,7.16839038344626,15.4505217207351));
#79204=CARTESIAN_POINT('Ctrl Pts',(0.149791017201536,8.08166951096257,15.2917281191975));
#79205=CARTESIAN_POINT('Ctrl Pts',(3.998040555002,7.02506164768895,15.13293451766));
#79206=CARTESIAN_POINT('Ctrl Pts',(6.87177757812056,4.25611235167798,14.9741409161225));
#79207=CARTESIAN_POINT('Ctrl Pts',(8.07053578202346,0.449746177688511,14.815347314585));
#79208=CARTESIAN_POINT('Ctrl Pts',(7.30212081407504,-3.46624451675291,14.6565537130475));
#79209=CARTESIAN_POINT('Ctrl Pts',(4.75383192560413,-6.53734666790537,14.49776011151));
#79210=CARTESIAN_POINT('Ctrl Pts',(1.04680824180907,-8.01498670854467,14.3389665099724));
#79211=CARTESIAN_POINT('Ctrl Pts',(-2.91537236650478,-7.53899352685007,
14.180172908435));
#79212=CARTESIAN_POINT('Ctrl Pts',(-6.16693815812707,-5.22538928569952,
14.0213793068974));
#79213=CARTESIAN_POINT('Ctrl Pts',(-7.91532799900807,-1.63810930691027,
13.8625857053599));
#79214=CARTESIAN_POINT('Ctrl Pts',(-7.73437618196141,2.34845577117709,13.7037921038224));
#79215=CARTESIAN_POINT('Ctrl Pts',(-5.66818926564769,5.76259055304671,13.5449985022848));
#79216=CARTESIAN_POINT('Ctrl Pts',(-2.22039520979373,7.77210811463608,13.3862049007473));
#79217=CARTESIAN_POINT('Ctrl Pts',(1.76861469660425,7.88719351152376,13.2274112992098));
#79218=CARTESIAN_POINT('Ctrl Pts',(5.32652913716566,6.07979496234801,13.0686176976723));
#79219=CARTESIAN_POINT('Ctrl Pts',(7.58611525099355,2.79046140125786,12.9098240961348));
#79220=CARTESIAN_POINT('Ctrl Pts',(7.99660450144244,-1.17904023713253,12.7510304945973));
#79221=CARTESIAN_POINT('Ctrl Pts',(6.45794114715554,-4.86115372860623,12.5922368930598));
#79222=CARTESIAN_POINT('Ctrl Pts',(3.34517058199709,-7.35837300023643,12.4334432915223));
#79223=CARTESIAN_POINT('Ctrl Pts',(-0.582977053767915,-8.06200701984604,
12.2746496899847));
#79224=CARTESIAN_POINT('Ctrl Pts',(-4.36902547196524,-6.80054673232866,
12.1158560884472));
#79225=CARTESIAN_POINT('Ctrl Pts',(-7.0901347178799,-3.8814699683987,11.9570624869097));
#79226=CARTESIAN_POINT('Ctrl Pts',(-8.08304113085587,-0.0162944824745385,
11.7982688853722));
#79227=CARTESIAN_POINT('Ctrl Pts',(-7.10572622407645,3.85285274332402,11.6394752838346));
#79228=CARTESIAN_POINT('Ctrl Pts',(-4.39640809321612,6.7828766250884,11.4806816822971));
#79229=CARTESIAN_POINT('Ctrl Pts',(-0.615476343747107,8.05959107545505,
11.3218880807596));
#79230=CARTESIAN_POINT('Ctrl Pts',(3.31547624498585,7.37180009917534,11.1630944792221));
#79231=CARTESIAN_POINT('Ctrl Pts',(6.43828968444762,4.88715104865834,11.0043008776846));
#79232=CARTESIAN_POINT('Ctrl Pts',(7.99178590855619,1.21127099571882,10.845507276147));
#79233=CARTESIAN_POINT('Ctrl Pts',(7.59730404804857,-2.75985337196954,10.6867136746096));
#79234=CARTESIAN_POINT('Ctrl Pts',(5.35099808250333,-6.05827029392982,10.527920073072));
#79235=CARTESIAN_POINT('Ctrl Pts',(1.80039954520892,-7.87999878876122,10.3691264715345));
#79236=CARTESIAN_POINT('Ctrl Pts',(-2.18904193629713,-7.78099703343982,
10.210332869997));
#79237=CARTESIAN_POINT('Ctrl Pts',(-5.64490985026715,-5.78539646140382,
10.0515392684595));
#79238=CARTESIAN_POINT('Ctrl Pts',(-7.72484492472234,-2.37961978523008,
9.89274566692192));
#79239=CARTESIAN_POINT('Ctrl Pts',(-7.92186812033116,1.60618333864722,9.7339520653844));
#79240=CARTESIAN_POINT('Ctrl Pts',(-6.18795551958646,5.20048323916983,9.57515846384689));
#79241=CARTESIAN_POINT('Ctrl Pts',(-2.94574403813367,7.52717818940584,9.41636486230936));
#79242=CARTESIAN_POINT('Ctrl Pts',(1.01448527998687,8.0191420395175,9.25757126077186));
#79243=CARTESIAN_POINT('Ctrl Pts',(4.72743631573194,6.55645981562959,9.09877765923432));
#79244=CARTESIAN_POINT('Ctrl Pts',(7.28808642089212,3.49565669865832,8.93998405769683));
#79245=CARTESIAN_POINT('Ctrl Pts',(8.07228345421928,-0.417204108326629,
8.78119045615929));
#79246=CARTESIAN_POINT('Ctrl Pts',(6.88888132491199,-4.22837244392516,8.6223968546218));
#79247=CARTESIAN_POINT('Ctrl Pts',(4.02633138033566,-7.00888543557329,8.46360325308425));
#79248=CARTESIAN_POINT('Ctrl Pts',(0.182373102247894,-8.0809999062519,8.30480965154676));
#79249=CARTESIAN_POINT('Ctrl Pts',(-3.70603816925928,-7.18339060063285,
8.14601605000923));
#79250=CARTESIAN_POINT('Ctrl Pts',(-6.69111178669606,-4.53484757088968,
7.98722244847172));
#79251=CARTESIAN_POINT('Ctrl Pts',(-8.04524342553875,-0.780946641642448,
7.8284288469342));
#79252=CARTESIAN_POINT('Ctrl Pts',(-7.43836684197983,3.16330810345782,7.66963524539667));
#79253=CARTESIAN_POINT('Ctrl Pts',(-5.01840670496898,6.33651430810264,7.51084164385916));
#79254=CARTESIAN_POINT('Ctrl Pts',(-1.37522232336164,7.96521079410926,7.35204804232165));
#79255=CARTESIAN_POINT('Ctrl Pts',(2.60316910433477,7.65240681403595,7.19325444078413));
#79256=CARTESIAN_POINT('Ctrl Pts',(5.94704448970765,5.47434756575656,7.03446083924661));
#79257=CARTESIAN_POINT('Ctrl Pts',(7.84134246312996,1.96192961371753,6.87566723770909));
#79258=CARTESIAN_POINT('Ctrl Pts',(7.82433257033507,-2.02870383793711,6.71687363617158));
#79259=CARTESIAN_POINT('Ctrl Pts',(5.90016093069667,-5.52484573767879,6.55808003463406));
#79260=CARTESIAN_POINT('Ctrl Pts',(2.53783963086772,-7.67432012892767,6.39928643309655));
#79261=CARTESIAN_POINT('Ctrl Pts',(-1.44307381341645,-7.95319793556645,
6.24049283155902));
#79262=CARTESIAN_POINT('Ctrl Pts',(-5.07224157842644,-6.29350338073708,
6.08169923002151));
#79263=CARTESIAN_POINT('Ctrl Pts',(-7.46506298134543,-3.09978291462693,
5.92290562848398));
#79264=CARTESIAN_POINT('Ctrl Pts',(-8.03829371275112,0.849501983995867,
5.76411202694648));
#79265=CARTESIAN_POINT('Ctrl Pts',(-6.65221019708932,4.59172287132047,5.60531842540895));
#79266=CARTESIAN_POINT('Ctrl Pts',(-3.64466686925759,7.21472264507814,5.44652482387144));
#79267=CARTESIAN_POINT('Ctrl Pts',(0.251255009786289,8.07915158623255,5.28773122233392));
#79268=CARTESIAN_POINT('Ctrl Pts',(4.08593410050795,6.97430727453083,5.1289376207964));
#79269=CARTESIAN_POINT('Ctrl Pts',(6.92467684182701,4.16949278324492,4.9701440192589));
#79270=CARTESIAN_POINT('Ctrl Pts',(8.07554669900292,0.348374719934165,4.81135041772136));
#79271=CARTESIAN_POINT('Ctrl Pts',(7.2580219856851,-3.55765882127316,4.65255681618386));
#79272=CARTESIAN_POINT('Ctrl Pts',(4.67137233239066,-6.59652180815247,4.49376321464633));
#79273=CARTESIAN_POINT('Ctrl Pts',(0.946087206037529,-8.02749889018125,
4.33496961310882));
#79274=CARTESIAN_POINT('Ctrl Pts',(-3.00980434103269,-7.50179293648743,
4.1761760115713));
#79275=CARTESIAN_POINT('Ctrl Pts',(-6.23206351075639,-5.14754347540663,
4.01738241003379));
#79276=CARTESIAN_POINT('Ctrl Pts',(-7.9352725858267,-1.53859300073383,3.85858880849627));
#79277=CARTESIAN_POINT('Ctrl Pts',(-7.70427855916092,2.44538571925539,3.69979520695874));
#79278=CARTESIAN_POINT('Ctrl Pts',(-5.59538565450209,5.83330770757355,3.54100160542123));
#79279=CARTESIAN_POINT('Ctrl Pts',(-2.12263131073224,7.79937534362048,3.38220800388371));
#79280=CARTESIAN_POINT('Ctrl Pts',(1.86750917446099,7.86436449554542,3.22341440234619));
#79281=CARTESIAN_POINT('Ctrl Pts',(5.40244890917294,6.01243421704986,3.06462080080868));
#79282=CARTESIAN_POINT('Ctrl Pts',(7.62055505981324,2.69498794326032,2.90582719927116));
#79283=CARTESIAN_POINT('Ctrl Pts',(7.98116972938295,-1.27935499062613,2.74703359773365));
#79284=CARTESIAN_POINT('Ctrl Pts',(6.39639398046123,-4.94185829923385,2.58823999619613));
#79285=CARTESIAN_POINT('Ctrl Pts',(3.25251299323007,-7.39979585771028,2.42944639465861));
#79286=CARTESIAN_POINT('Ctrl Pts',(-0.6841600112769,-8.05405142614452,2.27065279312109));
#79287=CARTESIAN_POINT('Ctrl Pts',(-4.45407069196273,-6.74515188068711,
2.11185919158358));
#79288=CARTESIAN_POINT('Ctrl Pts',(-7.13831265794001,-3.79213814459122,
1.95306559004606));
#79289=CARTESIAN_POINT('Ctrl Pts',(-8.08260849775468,0.0851997593911264,
1.79427198850854));
#79290=CARTESIAN_POINT('Ctrl Pts',(-7.05678854826809,3.94177071265802,1.63547838697102));
#79291=CARTESIAN_POINT('Ctrl Pts',(-4.31089366061186,6.83754423547215,1.47668478543351));
#79292=CARTESIAN_POINT('Ctrl Pts',(-0.514229384434719,8.0666843146748,1.31789118389599));
#79293=CARTESIAN_POINT('Ctrl Pts',(3.40777762088571,7.32958787930388,1.15909758235848));
#79294=CARTESIAN_POINT('Ctrl Pts',(6.49914609214958,4.80592667747565,1.00030398082096));
#79295=CARTESIAN_POINT('Ctrl Pts',(8.00636601379248,1.11082449054863,0.841510379283439));
#79296=CARTESIAN_POINT('Ctrl Pts',(7.56204953448809,-2.85502226162395,0.682716777745918));
#79297=CARTESIAN_POINT('Ctrl Pts',(5.27451090081715,-6.12499615304347,0.523923176208404));
#79298=CARTESIAN_POINT('Ctrl Pts',(1.70130605739136,-7.90195491287871,0.365129574670885));
#79299=CARTESIAN_POINT('Ctrl Pts',(-2.28655411685474,-7.75295442590588,
0.206335973133365));
#79300=CARTESIAN_POINT('Ctrl Pts',(-5.71713900016235,-5.71394888633152,
0.0475423715958508));
#79301=CARTESIAN_POINT('Ctrl Pts',(-7.75405266470557,-2.28266027366405,
-0.111251229941669));
#79302=CARTESIAN_POINT('Ctrl Pts',(-7.90122371833486,1.70622209623335,-0.270053878501701));
#79303=CARTESIAN_POINT('Ctrl Pts',(-6.71465618324548,4.08673202951572,-0.375925326549237));
#79304=CARTESIAN_POINT('Ctrl Pts',(-5.87252163179806,5.0634291864415,-0.428865574084263));
#79305=CARTESIAN_POINT('Ctrl Pts',(-1.90986695944544,-7.13093654462969,
20.4289621488151));
#79306=CARTESIAN_POINT('Ctrl Pts',(-3.09565806575062,-6.81334807072271,
20.3760309483026));
#79307=CARTESIAN_POINT('Ctrl Pts',(-5.30454812494481,-5.57551522146613,
20.2701685472776));
#79308=CARTESIAN_POINT('Ctrl Pts',(-7.32553356635487,-2.35748983795403,
20.11137494574));
#79309=CARTESIAN_POINT('Ctrl Pts',(-7.56063717713609,1.43425143228512,19.9525813442025));
#79310=CARTESIAN_POINT('Ctrl Pts',(-5.953005701823,4.87684463875962,19.793787742665));
#79311=CARTESIAN_POINT('Ctrl Pts',(-2.89426681882617,7.13049320113776,19.6349941411275));
#79312=CARTESIAN_POINT('Ctrl Pts',(0.869903311226413,7.6462163794815,19.47620053959));
#79313=CARTESIAN_POINT('Ctrl Pts',(4.42205657114865,6.2981348356096,19.3174069380524));
#79314=CARTESIAN_POINT('Ctrl Pts',(6.89633432763268,3.41492816378902,19.1586133365149));
#79315=CARTESIAN_POINT('Ctrl Pts',(7.6896527724844,-0.300673921684578,18.9998197349774));
#79316=CARTESIAN_POINT('Ctrl Pts',(6.60863471619527,-3.9429797962931,18.8410261334399));
#79317=CARTESIAN_POINT('Ctrl Pts',(3.91677959787454,-6.62419798998166,18.6822325319024));
#79318=CARTESIAN_POINT('Ctrl Pts',(0.270218443725032,-7.69078228866305,
18.5234389303648));
#79319=CARTESIAN_POINT('Ctrl Pts',(-3.44220744358733,-6.8827584039626,18.3646453288273));
#79320=CARTESIAN_POINT('Ctrl Pts',(-6.31560394056081,-4.39707863597438,
18.2058517272898));
#79321=CARTESIAN_POINT('Ctrl Pts',(-7.64958747996416,-0.839622068191634,
18.0470581257523));
#79322=CARTESIAN_POINT('Ctrl Pts',(-7.11900300236244,2.92249043907889,17.8882645242148));
#79323=CARTESIAN_POINT('Ctrl Pts',(-4.85317909561161,5.97225304923554,17.7294709226773));
#79324=CARTESIAN_POINT('Ctrl Pts',(-1.4044047778941,7.56629375779054,17.5706773211398));
#79325=CARTESIAN_POINT('Ctrl Pts',(2.38668974314694,7.31606902544708,17.4118837196022));
#79326=CARTESIAN_POINT('Ctrl Pts',(5.59603452864965,5.28257053942491,17.2530901180647));
#79327=CARTESIAN_POINT('Ctrl Pts',(7.44135971516583,1.9614585217979,17.0942965165272));
#79328=CARTESIAN_POINT('Ctrl Pts',(7.47287184199119,-1.83775416564101,16.9355029149897));
#79329=CARTESIAN_POINT('Ctrl Pts',(5.6828899072011,-5.1890188135372,16.7767093134522));
#79330=CARTESIAN_POINT('Ctrl Pts',(2.50771758758178,-7.2754729359924,16.6179157119147));
#79331=CARTESIAN_POINT('Ctrl Pts',(-1.27870470270501,-7.58854849272236,
16.4591221103771));
#79332=CARTESIAN_POINT('Ctrl Pts',(-4.75344587870222,-6.05193408925435,
16.3003285088396));
#79333=CARTESIAN_POINT('Ctrl Pts',(-7.06954635732759,-3.04017569298274,
16.1415349073021));
#79334=CARTESIAN_POINT('Ctrl Pts',(-7.66246236508284,0.712618022727699,
15.9827413057646));
#79335=CARTESIAN_POINT('Ctrl Pts',(-6.3876720888831,4.29171285473144,15.8239477042271));
#79336=CARTESIAN_POINT('Ctrl Pts',(-3.55590251128483,6.82471327403968,15.6651541026895));
#79337=CARTESIAN_POINT('Ctrl Pts',(0.142609524418191,7.69420668205179,15.506360501152));
#79338=CARTESIAN_POINT('Ctrl Pts',(3.8063608406262,6.68825620722965,15.3475668996145));
#79339=CARTESIAN_POINT('Ctrl Pts',(6.5423210993011,4.05205979425698,15.188773298077));
#79340=CARTESIAN_POINT('Ctrl Pts',(7.68360674209098,0.428183810400089,15.0299796965395));
#79341=CARTESIAN_POINT('Ctrl Pts',(6.95203221123971,-3.30006092011662,14.871186095002));
#79342=CARTESIAN_POINT('Ctrl Pts',(4.52591699248759,-6.22392394874059,14.7123924934644));
#79343=CARTESIAN_POINT('Ctrl Pts',(0.996620680668604,-7.63072088085122,
14.5535988919269));
#79344=CARTESIAN_POINT('Ctrl Pts',(-2.77559946154721,-7.17754843743,14.3948052903894));
#79345=CARTESIAN_POINT('Ctrl Pts',(-5.87127408757524,-4.97486628274192,
14.2360116888519));
#79346=CARTESIAN_POINT('Ctrl Pts',(-7.53584015010604,-1.55957275388004,
14.0772180873144));
#79347=CARTESIAN_POINT('Ctrl Pts',(-7.36356378097696,2.23586278337454,13.9184244857769));
#79348=CARTESIAN_POINT('Ctrl Pts',(-5.39643691983716,5.48631228721201,13.7596308842393));
#79349=CARTESIAN_POINT('Ctrl Pts',(-2.11394188253015,7.39948671597428,13.6008372827018));
#79350=CARTESIAN_POINT('Ctrl Pts',(1.68382126961865,7.50905452600891,13.4420436811643));
#79351=CARTESIAN_POINT('Ctrl Pts',(5.0711571444156,5.78830883412743,13.2832500796268));
#79352=CARTESIAN_POINT('Ctrl Pts',(7.22241098523436,2.65667715444709,13.1244564780893));
#79353=CARTESIAN_POINT('Ctrl Pts',(7.61321997951827,-1.12251302266783,12.9656628765518));
#79354=CARTESIAN_POINT('Ctrl Pts',(6.14832539976301,-4.6280934218341,12.8068692750142));
#79355=CARTESIAN_POINT('Ctrl Pts',(3.18479168316541,-7.00558747553948,12.6480756734767));
#79356=CARTESIAN_POINT('Ctrl Pts',(-0.555027143401427,-7.67548687789136,
12.4892820719392));
#79357=CARTESIAN_POINT('Ctrl Pts',(-4.15955947404802,-6.47450530345387,
12.3304884704017));
#79358=CARTESIAN_POINT('Ctrl Pts',(-6.75020945226223,-3.69537904594167,
12.1716948688642));
#79359=CARTESIAN_POINT('Ctrl Pts',(-7.69551254180441,-0.0155132693518444,
12.0129012673267));
#79360=CARTESIAN_POINT('Ctrl Pts',(-6.76505344841895,3.6681338283424,11.8541076657891));
#79361=CARTESIAN_POINT('Ctrl Pts',(-4.18562927894601,6.45768236148427,11.6953140642516));
#79362=CARTESIAN_POINT('Ctrl Pts',(-0.585968306459459,7.67318676212303,
11.5365204627141));
#79363=CARTESIAN_POINT('Ctrl Pts',(3.15652099405334,7.01837083351226,11.3777268611766));
#79364=CARTESIAN_POINT('Ctrl Pts',(6.12961609527162,4.65284434160248,11.2189332596391));
#79365=CARTESIAN_POINT('Ctrl Pts',(7.6086324064267,1.15319852864476,11.0601396581015));
#79366=CARTESIAN_POINT('Ctrl Pts',(7.23306335315761,-2.62753657858524,10.901346056564));
#79367=CARTESIAN_POINT('Ctrl Pts',(5.09445296497157,-5.76781613180305,10.7425524550265));
#79368=CARTESIAN_POINT('Ctrl Pts',(1.71408224406093,-7.50220474281994,10.583758853489));
#79369=CARTESIAN_POINT('Ctrl Pts',(-2.08409179201178,-7.40794946966191,
10.4249652519515));
#79370=CARTESIAN_POINT('Ctrl Pts',(-5.37427359911089,-5.50802480245821,
10.266171650414));
#79371=CARTESIAN_POINT('Ctrl Pts',(-7.35448948475168,-2.26553268819318,
10.1073780488764));
#79372=CARTESIAN_POINT('Ctrl Pts',(-7.54206671568352,1.52917742553764,9.9485844473389));
#79373=CARTESIAN_POINT('Ctrl Pts',(-5.8912838049685,4.95115431711746,9.78979084580139));
#79374=CARTESIAN_POINT('Ctrl Pts',(-2.8045150115428,7.16629956760294,9.63099724426387));
#79375=CARTESIAN_POINT('Ctrl Pts',(0.965847391993691,7.63467699107004,9.47220364272635));
#79376=CARTESIAN_POINT('Ctrl Pts',(4.50078687827297,6.24212074690652,9.31341004118883));
#79377=CARTESIAN_POINT('Ctrl Pts',(6.9386706747824,3.32806298160199,9.15461643965132));
#79378=CARTESIAN_POINT('Ctrl Pts',(7.6852706249148,-0.397201918949031,8.9958228381138));
#79379=CARTESIAN_POINT('Ctrl Pts',(6.5586048340755,-4.02564983239184,8.83702923657629));
#79380=CARTESIAN_POINT('Ctrl Pts',(3.83329530720239,-6.67285553795188,8.67823563503877));
#79381=CARTESIAN_POINT('Ctrl Pts',(0.173629513065194,-7.69356918047714,
8.51944203350125));
#79382=CARTESIAN_POINT('Ctrl Pts',(-3.52835804621482,-6.83899432960039,
8.36064843196373));
#79383=CARTESIAN_POINT('Ctrl Pts',(-6.37031704274931,-4.31743149539779,
8.20185483042622));
#79384=CARTESIAN_POINT('Ctrl Pts',(-7.65952698752967,-0.743505393322568,
8.0430612288887));
#79385=CARTESIAN_POINT('Ctrl Pts',(-7.08174613939356,3.01164831276487,7.88426762735118));
#79386=CARTESIAN_POINT('Ctrl Pts',(-4.77780715361458,6.0327201779516,7.72547402581366));
#79387=CARTESIAN_POINT('Ctrl Pts',(-1.30928946987534,7.58333139369951,7.56668042427615));
#79388=CARTESIAN_POINT('Ctrl Pts',(2.47836428969461,7.28552430441087,7.40788682273863));
#79389=CARTESIAN_POINT('Ctrl Pts',(5.66192287238406,5.211888652856,7.24909322120111));
#79390=CARTESIAN_POINT('Ctrl Pts',(7.46540173342043,1.8678680095869,7.0902996196636));
#79391=CARTESIAN_POINT('Ctrl Pts',(7.44920735296156,-1.93144084951585,6.93150601812608));
#79392=CARTESIAN_POINT('Ctrl Pts',(5.61728707126261,-5.25996577000468,6.77271241658856));
#79393=CARTESIAN_POINT('Ctrl Pts',(2.41616693423443,-7.30638702016992,6.61391881505104));
#79394=CARTESIAN_POINT('Ctrl Pts',(-1.37388792783737,-7.57189447260971,
6.45512521351352));
#79395=CARTESIAN_POINT('Ctrl Pts',(-4.82906099943468,-5.99177134129249,
6.29633161197601));
#79396=CARTESIAN_POINT('Ctrl Pts',(-7.10716237469161,-2.95116873837517,
6.1375380104385));
#79397=CARTESIAN_POINT('Ctrl Pts',(-7.65291046770089,0.8087739585009,5.97874440890097));
#79398=CARTESIAN_POINT('Ctrl Pts',(-6.33328052816671,4.37157999974144,5.81995080736346));
#79399=CARTESIAN_POINT('Ctrl Pts',(-3.46992909587,6.86882420886064,5.66115720582594));
#79400=CARTESIAN_POINT('Ctrl Pts',(0.239208986778566,7.69180947523007,5.50236360428843));
#79401=CARTESIAN_POINT('Ctrl Pts',(3.89004046947315,6.63993517200708,5.34357000275091));
#79402=CARTESIAN_POINT('Ctrl Pts',(6.59268419169601,3.96959306367241,5.18477640121339));
#79403=CARTESIAN_POINT('Ctrl Pts',(7.6883774186021,0.331672446434416,5.02598279967587));
#79404=CARTESIAN_POINT('Ctrl Pts',(6.91004763124565,-3.3870925107701,4.86718919813835));
#79405=CARTESIAN_POINT('Ctrl Pts',(4.44741079370755,-6.28026203072761,4.70839559660083));
#79406=CARTESIAN_POINT('Ctrl Pts',(0.900728555235199,-7.64263318578086,
4.54960199506332));
#79407=CARTESIAN_POINT('Ctrl Pts',(-2.86550404480521,-7.14213137038015,
4.3908083935258));
#79408=CARTESIAN_POINT('Ctrl Pts',(-5.93327710844758,-4.9007526663768,4.23201479198829));
#79409=CARTESIAN_POINT('Ctrl Pts',(-7.55482852533749,-1.46482759919173,
4.07322119045077));
#79410=CARTESIAN_POINT('Ctrl Pts',(-7.33490914097327,2.32814557880231,3.91442758891325));
#79411=CARTESIAN_POINT('Ctrl Pts',(-5.32712376237705,5.55363901990728,3.75563398737573));
#79412=CARTESIAN_POINT('Ctrl Pts',(-2.02086511857661,7.42544666090499,3.59684038583822));
#79413=CARTESIAN_POINT('Ctrl Pts',(1.77797440855997,7.48732001099973,3.4380467843007));
#79414=CARTESIAN_POINT('Ctrl Pts',(5.14343706334645,5.72417759294292,3.27925318276318));
#79415=CARTESIAN_POINT('Ctrl Pts',(7.25519963203433,2.56578101999284,3.12045958122566));
#79416=CARTESIAN_POINT('Ctrl Pts',(7.59852520312894,-1.21801834438284,2.96166597968815));
#79417=CARTESIAN_POINT('Ctrl Pts',(6.08972901437527,-4.7049287398031,2.80287237815062));
#79418=CARTESIAN_POINT('Ctrl Pts',(3.09657641555679,-7.04502437979951,2.64407877661313));
#79419=CARTESIAN_POINT('Ctrl Pts',(-0.651359044467085,-7.66791270251401,
2.48528517507559));
#79420=CARTESIAN_POINT('Ctrl Pts',(-4.2405273358362,-6.42176627012995,2.32649157353808));
#79421=CARTESIAN_POINT('Ctrl Pts',(-6.79607757738601,-3.61033009476553,
2.16769797200056));
#79422=CARTESIAN_POINT('Ctrl Pts',(-7.69510065061119,0.0811149920356376,
2.00890437046304));
#79423=CARTESIAN_POINT('Ctrl Pts',(-6.7184620118726,3.75278876664151,1.85011076892552));
#79424=CARTESIAN_POINT('Ctrl Pts',(-4.10421470020542,6.50972901997924,1.69131716738801));
#79425=CARTESIAN_POINT('Ctrl Pts',(-0.489575472055369,7.67993992723675,
1.53252356585049));
#79426=CARTESIAN_POINT('Ctrl Pts',(3.24439712685584,6.97818241158302,1.37372996431298));
#79427=CARTESIAN_POINT('Ctrl Pts',(6.18755483901151,4.57551414409174,1.21493636277546));
#79428=CARTESIAN_POINT('Ctrl Pts',(7.62251349163834,1.05756777187836,1.05614276123794));
#79429=CARTESIAN_POINT('Ctrl Pts',(7.1994990613437,-2.71814274674258,0.897349159700425));
#79430=CARTESIAN_POINT('Ctrl Pts',(5.02163283991908,-5.83134292541437,0.73855555816291));
#79431=CARTESIAN_POINT('Ctrl Pts',(1.61973963637579,-7.52310821538431,0.579761956625391));
#79432=CARTESIAN_POINT('Ctrl Pts',(-2.17692890570593,-7.38125132047662,
0.42096835508787));
#79433=CARTESIAN_POINT('Ctrl Pts',(-5.44303983695429,-5.44000266807223,
0.262174753550357));
#79434=CARTESIAN_POINT('Ctrl Pts',(-7.38229690595861,-2.17322174665223,
0.103381152012836));
#79435=CARTESIAN_POINT('Ctrl Pts',(-7.52241207680334,1.62441998353129,-0.0554214965471939));
#79436=CARTESIAN_POINT('Ctrl Pts',(-6.39273264054252,3.89080014303998,-0.16129294459473));
#79437=CARTESIAN_POINT('Ctrl Pts',(-5.59097289471971,4.82067110360889,-0.214233192129757));
#79438=CARTESIAN_POINT('Ctrl Pts',(-1.81369038328508,-6.77183872460225,
20.6435945307695));
#79439=CARTESIAN_POINT('Ctrl Pts',(-2.93976773409445,-6.47024328722449,
20.590663330257));
#79440=CARTESIAN_POINT('Ctrl Pts',(-5.03742309080986,-5.29474489781683,
20.484800929232));
#79441=CARTESIAN_POINT('Ctrl Pts',(-6.95663628087881,-2.23877198704513,
20.3260073276945));
#79442=CARTESIAN_POINT('Ctrl Pts',(-7.17990060609302,1.36202577728435,20.167213726157));
#79443=CARTESIAN_POINT('Ctrl Pts',(-5.65322581221712,4.63125778387307,20.0084201246195));
#79444=CARTESIAN_POINT('Ctrl Pts',(-2.7485180944176,6.77141770688483,19.8496265230819));
#79445=CARTESIAN_POINT('Ctrl Pts',(0.826096949924359,7.26117023355868,19.6908329215445));
#79446=CARTESIAN_POINT('Ctrl Pts',(4.19937181371192,5.98097502419469,19.5320393200069));
#79447=CARTESIAN_POINT('Ctrl Pts',(6.54905054411643,3.24296011281956,19.3732457184694));
#79448=CARTESIAN_POINT('Ctrl Pts',(7.30241926814944,-0.285532663710926,
19.2144521169319));
#79449=CARTESIAN_POINT('Ctrl Pts',(6.27583883376233,-3.74442026061367,19.0556585153944));
#79450=CARTESIAN_POINT('Ctrl Pts',(3.71953944487051,-6.29061837631592,18.8968649138569));
#79451=CARTESIAN_POINT('Ctrl Pts',(0.256610854670558,-7.30349190445053,
18.7380713123193));
#79452=CARTESIAN_POINT('Ctrl Pts',(-3.26886566984719,-6.53615827322664,
18.5792777107818));
#79453=CARTESIAN_POINT('Ctrl Pts',(-5.99756442457044,-4.17565171080327,
18.4204841092443));
#79454=CARTESIAN_POINT('Ctrl Pts',(-7.26437157305314,-0.79734060173242,
18.2616905077068));
#79455=CARTESIAN_POINT('Ctrl Pts',(-6.76050612850616,2.77532043705234,18.1028969061693));
#79456=CARTESIAN_POINT('Ctrl Pts',(-4.60878398389947,5.67150390678975,17.9441033046317));
#79457=CARTESIAN_POINT('Ctrl Pts',(-1.33368213283598,7.18527233415214,17.7853097030942));
#79458=CARTESIAN_POINT('Ctrl Pts',(2.26650145112079,6.94764835282353,17.6265161015567));
#79459=CARTESIAN_POINT('Ctrl Pts',(5.31423089914606,5.01655224673973,17.4677225000192));
#79460=CARTESIAN_POINT('Ctrl Pts',(7.06662968706476,1.86268391136018,17.3089288984817));
#79461=CARTESIAN_POINT('Ctrl Pts',(7.09655493452627,-1.74520902651409,17.1501352969442));
#79462=CARTESIAN_POINT('Ctrl Pts',(5.39671243747327,-4.92771157396768,16.9913416954066));
#79463=CARTESIAN_POINT('Ctrl Pts',(2.38143460731556,-6.90909659052469,16.8325480938691));
#79464=CARTESIAN_POINT('Ctrl Pts',(-1.21431202884984,-7.20640637101727,
16.6737544923316));
#79465=CARTESIAN_POINT('Ctrl Pts',(-4.51407310599876,-5.74717239003019,
16.5149608907941));
#79466=CARTESIAN_POINT('Ctrl Pts',(-6.71354000814598,-2.88707932800769,
16.3561672892566));
#79467=CARTESIAN_POINT('Ctrl Pts',(-7.27659810810584,0.676732192462313,
16.1973736877191));
#79468=CARTESIAN_POINT('Ctrl Pts',(-6.06600338410468,4.07559191175679,16.0385800861815));
#79469=CARTESIAN_POINT('Ctrl Pts',(-3.3768353113398,6.4810361646331,15.879786484644));
#79470=CARTESIAN_POINT('Ctrl Pts',(0.135428031634848,7.30674385314103,15.7209928831065));
#79471=CARTESIAN_POINT('Ctrl Pts',(3.61468112625038,6.35145076677037,15.562199281569));
#79472=CARTESIAN_POINT('Ctrl Pts',(6.21286462048166,3.84800723683599,15.4034056800315));
#79473=CARTESIAN_POINT('Ctrl Pts',(7.2966777021585,0.406621443111669,15.244612078494));
#79474=CARTESIAN_POINT('Ctrl Pts',(6.60194360840439,-3.13387732348034,15.0858184769564));
#79475=CARTESIAN_POINT('Ctrl Pts',(4.29800205937108,-5.91050122957581,14.9270248754189));
#79476=CARTESIAN_POINT('Ctrl Pts',(0.94643311952814,-7.24645505315777,14.7682312738814));
#79477=CARTESIAN_POINT('Ctrl Pts',(-2.63582655658965,-6.81610334800993,
14.6094376723439));
#79478=CARTESIAN_POINT('Ctrl Pts',(-5.57561001702343,-4.72434327978433,
14.4506440708064));
#79479=CARTESIAN_POINT('Ctrl Pts',(-7.15635230120401,-1.4810362008498,14.2918504692689));
#79480=CARTESIAN_POINT('Ctrl Pts',(-6.9927513799925,2.12326979557197,14.1330568677313));
#79481=CARTESIAN_POINT('Ctrl Pts',(-5.12468457402663,5.2100340213773,13.9742632661938));
#79482=CARTESIAN_POINT('Ctrl Pts',(-2.00748855526656,7.02686531731248,13.8154696646563));
#79483=CARTESIAN_POINT('Ctrl Pts',(1.59902784263307,7.13091554049405,13.6566760631188));
#79484=CARTESIAN_POINT('Ctrl Pts',(4.81578515166555,5.49682270590684,13.4978824615813));
#79485=CARTESIAN_POINT('Ctrl Pts',(6.85870671947516,2.52289290763632,13.3390888600438));
#79486=CARTESIAN_POINT('Ctrl Pts',(7.22983545759411,-1.06598580820313,13.1802952585062));
#79487=CARTESIAN_POINT('Ctrl Pts',(5.83870965237047,-4.39503311506197,13.0215016569687));
#79488=CARTESIAN_POINT('Ctrl Pts',(3.02441278433374,-6.65280195084252,12.8627080554312));
#79489=CARTESIAN_POINT('Ctrl Pts',(-0.527077233034936,-7.2889667359367,
12.7039144538937));
#79490=CARTESIAN_POINT('Ctrl Pts',(-3.95009347613082,-6.14846387457909,
12.5451208523562));
#79491=CARTESIAN_POINT('Ctrl Pts',(-6.41028418664454,-3.50928812348463,
12.3863272508187));
#79492=CARTESIAN_POINT('Ctrl Pts',(-7.30798395275296,-0.0147320562291548,
12.2275336492811));
#79493=CARTESIAN_POINT('Ctrl Pts',(-6.42438067276146,3.4834149133608,12.0687400477436));
#79494=CARTESIAN_POINT('Ctrl Pts',(-3.97485046467588,6.13248809788012,11.9099464462061));
#79495=CARTESIAN_POINT('Ctrl Pts',(-0.55646026917181,7.28678244879102,11.7511528446686));
#79496=CARTESIAN_POINT('Ctrl Pts',(2.99756574312083,6.66494156784918,11.592359243131));
#79497=CARTESIAN_POINT('Ctrl Pts',(5.82094250609562,4.41853763454662,11.4335656415936));
#79498=CARTESIAN_POINT('Ctrl Pts',(7.22547890429721,1.0951260615707,11.274772040056));
#79499=CARTESIAN_POINT('Ctrl Pts',(6.86882265826663,-2.49521978520095,11.1159784385185));
#79500=CARTESIAN_POINT('Ctrl Pts',(4.83790784743979,-5.47736196967628,10.957184836981));
#79501=CARTESIAN_POINT('Ctrl Pts',(1.62776494291293,-7.12441069687865,10.7983912354435));
#79502=CARTESIAN_POINT('Ctrl Pts',(-1.97914164772644,-7.03490190588398,
10.639597633906));
#79503=CARTESIAN_POINT('Ctrl Pts',(-5.10363734795463,-5.23065314351258,
10.4808040323684));
#79504=CARTESIAN_POINT('Ctrl Pts',(-6.98413404478104,-2.15144559115629,
10.3220104308309));
#79505=CARTESIAN_POINT('Ctrl Pts',(-7.16226531103587,1.45217151242805,10.1632168292934));
#79506=CARTESIAN_POINT('Ctrl Pts',(-5.59461209035054,4.70182539506509,10.0044232277559));
#79507=CARTESIAN_POINT('Ctrl Pts',(-2.66328598495193,6.80542094580004,9.84562962621837));
#79508=CARTESIAN_POINT('Ctrl Pts',(0.917209504000515,7.25021194262256,9.68683602468087));
#79509=CARTESIAN_POINT('Ctrl Pts',(4.274137440814,5.92778167818344,9.52804242314334));
#79510=CARTESIAN_POINT('Ctrl Pts',(6.58925492867272,3.16046926454566,9.36924882160583));
#79511=CARTESIAN_POINT('Ctrl Pts',(7.2982577956103,-0.377199729571435,9.21045522006831));
#79512=CARTESIAN_POINT('Ctrl Pts',(6.22832834323901,-3.8229272208585,9.05166161853079));
#79513=CARTESIAN_POINT('Ctrl Pts',(3.64025923406912,-6.33682564033049,8.89286801699328));
#79514=CARTESIAN_POINT('Ctrl Pts',(0.1648859238825,-7.30613845470238,8.73407441545576));
#79515=CARTESIAN_POINT('Ctrl Pts',(-3.35067792317036,-6.49459805856793,
8.57528081391825));
#79516=CARTESIAN_POINT('Ctrl Pts',(-6.04952229880255,-4.10001541990588,
8.41648721238073));
#79517=CARTESIAN_POINT('Ctrl Pts',(-7.2738105495206,-0.706064145002688,
8.25769361084321));
#79518=CARTESIAN_POINT('Ctrl Pts',(-6.72512543680727,2.85998852207193,8.0989000093057));
#79519=CARTESIAN_POINT('Ctrl Pts',(-4.53720760226019,5.72892604780056,7.94010640776816));
#79520=CARTESIAN_POINT('Ctrl Pts',(-1.24335661638905,7.20145199328975,7.78131280623066));
#79521=CARTESIAN_POINT('Ctrl Pts',(2.35355947505446,6.91864179478579,7.62251920469314));
#79522=CARTESIAN_POINT('Ctrl Pts',(5.37680125506048,4.94942973995545,7.46372560315563));
#79523=CARTESIAN_POINT('Ctrl Pts',(7.08946100371092,1.77380640545626,7.30493200161811));
#79524=CARTESIAN_POINT('Ctrl Pts',(7.07408213558805,-1.83417786109458,7.14613840008059));
#79525=CARTESIAN_POINT('Ctrl Pts',(5.33441321182856,-4.99508580233056,6.98734479854307));
#79526=CARTESIAN_POINT('Ctrl Pts',(2.29449423760114,-6.93845391141215,6.82855119700556));
#79527=CARTESIAN_POINT('Ctrl Pts',(-1.30470204225829,-7.19059100965299,
6.66975759546803));
#79528=CARTESIAN_POINT('Ctrl Pts',(-4.58588042044292,-5.69003930184789,
6.51096399393052));
#79529=CARTESIAN_POINT('Ctrl Pts',(-6.74926176803779,-2.80255456212341,
6.352170392393));
#79530=CARTESIAN_POINT('Ctrl Pts',(-7.26752722265067,0.768045933005938,
6.19337679085548));
#79531=CARTESIAN_POINT('Ctrl Pts',(-6.0143508592441,4.15143712816239,6.03458318931797));
#79532=CARTESIAN_POINT('Ctrl Pts',(-3.29519132248241,6.52292577264314,5.87578958778045));
#79533=CARTESIAN_POINT('Ctrl Pts',(0.227162963770855,7.30446736422759,5.71699598624294));
#79534=CARTESIAN_POINT('Ctrl Pts',(3.69414683843833,6.30556306948332,5.55820238470542));
#79535=CARTESIAN_POINT('Ctrl Pts',(6.26069154156504,3.7696933440999,5.39940878316791));
#79536=CARTESIAN_POINT('Ctrl Pts',(7.30120813820126,0.314970172934666,5.24061518163038));
#79537=CARTESIAN_POINT('Ctrl Pts',(6.56207327680621,-3.21652620026706,5.08182158009287));
#79538=CARTESIAN_POINT('Ctrl Pts',(4.22344925502444,-5.96400225330274,4.92302797855534));
#79539=CARTESIAN_POINT('Ctrl Pts',(0.85536990443287,-7.25776748138049,4.76423437701783));
#79540=CARTESIAN_POINT('Ctrl Pts',(-2.72120374857774,-6.78246980427286,
4.60544077548031));
#79541=CARTESIAN_POINT('Ctrl Pts',(-5.63449070613878,-4.65396185734695,
4.4466471739428));
#79542=CARTESIAN_POINT('Ctrl Pts',(-7.17438446484828,-1.39106219764965,
4.28785357240528));
#79543=CARTESIAN_POINT('Ctrl Pts',(-6.96553972278562,2.21090543834923,4.12905997086776));
#79544=CARTESIAN_POINT('Ctrl Pts',(-5.05886187025201,5.27397033224099,3.97026636933025));
#79545=CARTESIAN_POINT('Ctrl Pts',(-1.91909892642098,7.05151797818953,3.81147276779273));
#79546=CARTESIAN_POINT('Ctrl Pts',(1.68843964265895,7.11027552645404,3.6526791662552));
#79547=CARTESIAN_POINT('Ctrl Pts',(4.88442521751996,5.43592096883599,3.4938855647177));
#79548=CARTESIAN_POINT('Ctrl Pts',(6.88984420425543,2.43657409672536,3.33509196318017));
#79549=CARTESIAN_POINT('Ctrl Pts',(7.21588067687493,-1.15668169813955,3.17629836164266));
#79550=CARTESIAN_POINT('Ctrl Pts',(5.7830640482893,-4.46799918037234,3.01750476010513));
#79551=CARTESIAN_POINT('Ctrl Pts',(2.94063983788352,-6.69025290188873,2.85871115856763));
#79552=CARTESIAN_POINT('Ctrl Pts',(-0.618558077657272,-7.28177397888349,
2.6999175570301));
#79553=CARTESIAN_POINT('Ctrl Pts',(-4.02698397970966,-6.09838065957278,
2.54112395549259));
#79554=CARTESIAN_POINT('Ctrl Pts',(-6.45384249683203,-3.42852204493986,
2.38233035395507));
#79555=CARTESIAN_POINT('Ctrl Pts',(-7.3075928034677,0.0770302246801563,
2.22353675241756));
#79556=CARTESIAN_POINT('Ctrl Pts',(-6.38013547547711,3.56380682062498,2.06474315088003));
#79557=CARTESIAN_POINT('Ctrl Pts',(-3.89753573979897,6.18191380448636,1.90594954934252));
#79558=CARTESIAN_POINT('Ctrl Pts',(-0.464921559676021,7.29319553979868,
1.747155947805));
#79559=CARTESIAN_POINT('Ctrl Pts',(3.08101663282597,6.62677694386218,1.58836234626749));
#79560=CARTESIAN_POINT('Ctrl Pts',(5.87596358587343,4.34510161070782,1.42956874472997));
#79561=CARTESIAN_POINT('Ctrl Pts',(7.23866096948422,1.00431105320811,1.27077514319245));
#79562=CARTESIAN_POINT('Ctrl Pts',(6.8369485881993,-2.58126323186122,1.11198154165493));
#79563=CARTESIAN_POINT('Ctrl Pts',(4.768754779021,-5.53768969778528,0.953187940117417));
#79564=CARTESIAN_POINT('Ctrl Pts',(1.53817321536023,-7.14426151788992,0.794394338579897));
#79565=CARTESIAN_POINT('Ctrl Pts',(-2.06730369455713,-7.00954821504736,
0.635600737042377));
#79566=CARTESIAN_POINT('Ctrl Pts',(-5.16894067374621,-5.16605644981294,
0.476807135504864));
#79567=CARTESIAN_POINT('Ctrl Pts',(-7.01054114721167,-2.06378321964041,
0.318013533967343));
#79568=CARTESIAN_POINT('Ctrl Pts',(-7.14360043527182,1.54261787082922,0.159210885407313));
#79569=CARTESIAN_POINT('Ctrl Pts',(-6.07080909783958,3.69486825656423,0.0533394373597762));
#79570=CARTESIAN_POINT('Ctrl Pts',(-5.30942415764135,4.57791302077629,0.000399189824749598));
#79571=CARTESIAN_POINT('Ctrl Pts',(-5.31037376991248,4.57794244025912,-1.11022302462516E-16));
#79572=CARTESIAN_POINT('Ctrl Pts',(-5.44252110837334,4.44698907439619,1.26508291621284E-16));
#79573=CARTESIAN_POINT('Ctrl Pts',(-5.56908400938008,4.31092088233243,4.32413578291971E-15));
#79574=CARTESIAN_POINT('Ctrl Pts',(-5.68993613636022,4.17020851221304,1.99840144432528E-15));
#79575=CARTESIAN_POINT('Ctrl Pts',(-5.81376161366555,4.02603416602499,-3.84553425878751E-16));
#79576=CARTESIAN_POINT('Ctrl Pts',(-5.93159233267655,3.87698397375777,-9.83144615789292E-15));
#79577=CARTESIAN_POINT('Ctrl Pts',(-6.04326669365349,3.72351578252423,-8.21565038222616E-15));
#79578=CARTESIAN_POINT('Ctrl Pts',(-6.15586096386687,3.56878340848829,-6.58654460912372E-15));
#79579=CARTESIAN_POINT('Ctrl Pts',(-6.26219748724818,3.40955944596802,-1.19427616521068E-14));
#79580=CARTESIAN_POINT('Ctrl Pts',(-6.36207781039616,3.24627111619497,-9.10382880192628E-15));
#79581=CARTESIAN_POINT('Ctrl Pts',(-6.46207486290856,3.08279195260851,-6.26157811278843E-15));
#79582=CARTESIAN_POINT('Ctrl Pts',(-6.55560105221217,2.91523834903128,1.65940183112773E-14));
#79583=CARTESIAN_POINT('Ctrl Pts',(-6.64241781295179,2.7440052051437,9.99200722162641E-15));
#79584=CARTESIAN_POINT('Ctrl Pts',(-6.69138001066649,2.64743455478877,6.2686596844429E-15));
#79585=CARTESIAN_POINT('Ctrl Pts',(-6.73820743199069,2.54969301070825,-5.70522088311913E-15));
#79586=CARTESIAN_POINT('Ctrl Pts',(-6.7828509533718,2.4508477193249,-6.21724893790088E-15));
#79587=CARTESIAN_POINT('Ctrl Pts',(-6.79660110048274,2.42040349683309,-6.92406093104009E-15));
#79588=CARTESIAN_POINT('Ctrl Pts',(-6.81014404104715,2.38985455306603,7.73134273691482E-16));
#79589=CARTESIAN_POINT('Ctrl Pts',(-6.82347824501989,2.35920280883552,1.99840144432528E-15));
#79590=CARTESIAN_POINT('Ctrl Pts',(-6.83289223867303,2.33756257247543,2.6022547736133E-15));
#79591=CARTESIAN_POINT('Ctrl Pts',(-6.84220312213329,2.31586888580966,6.65976333931259E-16));
#79592=CARTESIAN_POINT('Ctrl Pts',(-6.85140731350048,2.29412958992203,-3.33066907387547E-16));
#79593=CARTESIAN_POINT('Ctrl Pts',(-6.92787174140525,2.11352895301797,1.48312058419164E-15));
#79594=CARTESIAN_POINT('Ctrl Pts',(-6.9968154363246,1.93016662573821,-4.84967905120705E-15));
#79595=CARTESIAN_POINT('Ctrl Pts',(-7.05806709983238,1.74450817174022,-7.38298311375729E-15));
#79596=CARTESIAN_POINT('Ctrl Pts',(-7.08072012930876,1.6758451152598,-8.31988846971198E-15));
#79597=CARTESIAN_POINT('Ctrl Pts',(-7.10232070581907,1.60686761954515,-1.29953418837246E-14));
#79598=CARTESIAN_POINT('Ctrl Pts',(-7.12285886516232,1.53759799276406,-1.52655665885959E-14));
#79599=CARTESIAN_POINT('Ctrl Pts',(-7.17789503540859,1.35197595581785,-1.15950958872121E-14));
#79600=CARTESIAN_POINT('Ctrl Pts',(-7.2253056020522,1.16425810273759,-1.12411624720764E-15));
#79601=CARTESIAN_POINT('Ctrl Pts',(-7.26516741253555,0.974925030014523,
-2.38697950294409E-15));
#79602=CARTESIAN_POINT('Ctrl Pts',(-7.30539133219011,0.783872034357297,
-3.66131475057827E-15));
#79603=CARTESIAN_POINT('Ctrl Pts',(-7.33792888466284,0.591173700608657,
-1.51778296889488E-15));
#79604=CARTESIAN_POINT('Ctrl Pts',(-7.36281046690392,0.397301655480222,
1.66533453693773E-15));
#79605=CARTESIAN_POINT('Ctrl Pts',(-7.38777154345532,0.202810207438947,
4.85862180321062E-15));
#79606=CARTESIAN_POINT('Ctrl Pts',(-7.40502777710334,0.00713684282182964,
4.74315758813333E-15));
#79607=CARTESIAN_POINT('Ctrl Pts',(-7.41455912394538,-0.189254417725043,
1.94289029309402E-15));
#79608=CARTESIAN_POINT('Ctrl Pts',(-7.41891547422354,-0.279016036590548,
6.63013963776067E-16));
#79609=CARTESIAN_POINT('Ctrl Pts',(-7.42165739195025,-0.368927726290736,
-8.85908993222617E-15));
#79610=CARTESIAN_POINT('Ctrl Pts',(-7.42277933840189,-0.458945409812431,
5.55111512312578E-16));
#79611=CARTESIAN_POINT('Ctrl Pts',(-7.42308627605976,-0.48357209044044,
-2.85004532978439E-15));
#79612=CARTESIAN_POINT('Ctrl Pts',(-7.42327183994005,-0.508199168176247,
4.55160162443761E-15));
#79613=CARTESIAN_POINT('Ctrl Pts',(-7.42333615702577,-0.532819130412786,
9.04831765069503E-15));
#79614=CARTESIAN_POINT('Ctrl Pts',(-7.4238573231957,-0.732316531096511,
5.3206392005416E-15));
#79615=CARTESIAN_POINT('Ctrl Pts',(-7.41642317468771,-0.931480295265724,
2.0508515330919E-15));
#79616=CARTESIAN_POINT('Ctrl Pts',(-7.40111960803424,-1.12981272812747,
-3.88578058618805E-15));
#79617=CARTESIAN_POINT('Ctrl Pts',(-7.38567043395387,-1.3300322162014,1.32328955243151E-15));
#79618=CARTESIAN_POINT('Ctrl Pts',(-7.36220152785829,-1.52940517206027,
-1.20070939886438E-14));
#79619=CARTESIAN_POINT('Ctrl Pts',(-7.33075075935929,-1.72743569513311,
-6.99440505513849E-15));
#79620=CARTESIAN_POINT('Ctrl Pts',(-7.30904612801572,-1.86409943033589,
-3.61599122083957E-15));
#79621=CARTESIAN_POINT('Ctrl Pts',(-7.28353901753502,-2.00012416283928,
4.47127839975347E-15));
#79622=CARTESIAN_POINT('Ctrl Pts',(-7.25422750746073,-2.13534865261956,
6.77236045021345E-15));
#79623=CARTESIAN_POINT('Ctrl Pts',(-7.21194426750884,-2.33041637633158,
3.05948464044368E-15));
#79624=CARTESIAN_POINT('Ctrl Pts',(-7.16174660423667,-2.52381943143324,
-4.47725060636341E-15));
#79625=CARTESIAN_POINT('Ctrl Pts',(-7.10388082685099,-2.71516162535246,
-5.55111512312578E-15));
#79626=CARTESIAN_POINT('Ctrl Pts',(-7.0646932418533,-2.84474147075709,-9.08304634261343E-15));
#79627=CARTESIAN_POINT('Ctrl Pts',(-7.02198779033188,-2.97337609690067,
5.42360386022428E-15));
#79628=CARTESIAN_POINT('Ctrl Pts',(-6.97582777173374,-3.10093944226419,
-9.10382880192628E-15));
#79629=CARTESIAN_POINT('Ctrl Pts',(-6.95395173385994,-3.16139393641793,
1.05087312514034E-15));
#79630=CARTESIAN_POINT('Ctrl Pts',(-6.93129965751152,-3.22160777669937,
-3.3264548240337E-15));
#79631=CARTESIAN_POINT('Ctrl Pts',(-6.90787748303903,-3.28156724782363,
-4.38538094726937E-15));
#79632=CARTESIAN_POINT('Ctrl Pts',(-6.89397770438652,-3.31714991235063,
5.87276203710888E-15));
#79633=CARTESIAN_POINT('Ctrl Pts',(-6.8798046872329,-3.35264758566453,1.41800447596743E-14));
#79634=CARTESIAN_POINT('Ctrl Pts',(-6.86537571403821,-3.38801888857102,
1.18793863634892E-14));
#79635=CARTESIAN_POINT('Ctrl Pts',(-6.78527926138308,-3.58436798773231,
-8.91763310105958E-16));
#79636=CARTESIAN_POINT('Ctrl Pts',(-6.69720860879802,-3.77706587145206,
1.31933643606969E-14));
#79637=CARTESIAN_POINT('Ctrl Pts',(-6.60153595221269,-3.96566681700067,
7.7715611723761E-15));
#79638=CARTESIAN_POINT('Ctrl Pts',(-6.50894990986814,-4.14818307351552,
2.52467750159629E-15));
#79639=CARTESIAN_POINT('Ctrl Pts',(-6.40924387087696,-4.32686313181129,
2.03372667533341E-14));
#79640=CARTESIAN_POINT('Ctrl Pts',(-6.30270053211344,-4.50129762818047,
1.2712053631958E-14));
#79641=CARTESIAN_POINT('Ctrl Pts',(-6.1908293138171,-4.68445501603969,4.70552885474135E-15));
#79642=CARTESIAN_POINT('Ctrl Pts',(-6.07142002024269,-4.86293253556795,
7.3181577952022E-15));
#79643=CARTESIAN_POINT('Ctrl Pts',(-5.94474116946604,-5.03623808905791,
7.46624984060418E-15));
#79644=CARTESIAN_POINT('Ctrl Pts',(-5.82468128040108,-5.20048843865281,
7.60660408626838E-15));
#79645=CARTESIAN_POINT('Ctrl Pts',(-5.69809095197815,-5.36009364644713,
2.44554910442882E-14));
#79646=CARTESIAN_POINT('Ctrl Pts',(-5.56515303095831,-5.51460913021791,
5.27355936696949E-16));
#79647=CARTESIAN_POINT('Ctrl Pts',(-5.55782409690619,-5.52312764609283,
-7.91814115371847E-16));
#79648=CARTESIAN_POINT('Ctrl Pts',(-5.55047585952526,-5.5316306845626,5.34033577522075E-15));
#79649=CARTESIAN_POINT('Ctrl Pts',(-5.54310834577199,-5.54011816828261,
4.46864767411626E-15));
#79650=CARTESIAN_POINT('Ctrl Pts',(-5.46343909916247,-5.63189830690586,
1.04620899136104E-14));
#79651=CARTESIAN_POINT('Ctrl Pts',(-5.38151618195913,-5.72185994455588,
-5.7452322777736E-15));
#79652=CARTESIAN_POINT('Ctrl Pts',(-5.29741727864766,-5.80994862150633,
3.10862446895044E-15));
#79653=CARTESIAN_POINT('Ctrl Pts',(-5.27398864270865,-5.83448874582851,
-2.19216472326236E-15));
#79654=CARTESIAN_POINT('Ctrl Pts',(-5.2503884899981,-5.8588860528994,1.27922499778416E-14));
#79655=CARTESIAN_POINT('Ctrl Pts',(-5.22663715390791,-5.88312049455735,
1.47937218031302E-14));
#79656=CARTESIAN_POINT('Ctrl Pts',(-5.08244539987714,-6.0302451294557,6.10094433106069E-15));
#79657=CARTESIAN_POINT('Ctrl Pts',(-4.93255824560136,-6.17150517691054,
4.5988494700527E-15));
#79658=CARTESIAN_POINT('Ctrl Pts',(-4.77743786746376,-6.30670076408454,
6.46704911844154E-15));
#79659=CARTESIAN_POINT('Ctrl Pts',(-4.62024030664534,-6.44370672546966,
8.36026541519431E-15));
#79660=CARTESIAN_POINT('Ctrl Pts',(-4.4576680003625,-6.57448521633667,2.56788104009255E-14));
#79661=CARTESIAN_POINT('Ctrl Pts',(-4.29015760295661,-6.69879808025457,
1.60982338570648E-14));
#79662=CARTESIAN_POINT('Ctrl Pts',(-4.16413488960682,-6.79232209224324,
8.89050066431821E-15));
#79663=CARTESIAN_POINT('Ctrl Pts',(-4.03531626522646,-6.88218600290244,
8.03682837398228E-15));
#79664=CARTESIAN_POINT('Ctrl Pts',(-3.90387378481224,-6.96827480951185,
-1.36002320516582E-15));
#79665=CARTESIAN_POINT('Ctrl Pts',(-3.87679878053257,-6.98600769769256,
-2.77050060624404E-15));
#79666=CARTESIAN_POINT('Ctrl Pts',(-3.84961241206961,-7.00358036772389,
5.09502761441384E-15));
#79667=CARTESIAN_POINT('Ctrl Pts',(-3.82231612917412,-7.02099174562584,
6.86950496486816E-15));
#79668=CARTESIAN_POINT('Ctrl Pts',(-3.79414288534319,-7.03896250732048,
3.1539969567683E-15));
#79669=CARTESIAN_POINT('Ctrl Pts',(-3.7658597368087,-7.05675683475663,-6.31539703715498E-15));
#79670=CARTESIAN_POINT('Ctrl Pts',(-3.73747339603306,-7.07437079137119,
-9.56179579958416E-15));
#79671=CARTESIAN_POINT('Ctrl Pts',(-3.55786207395122,-7.18582108570944,
-4.03029781972554E-15));
#79672=CARTESIAN_POINT('Ctrl Pts',(-3.37406099776166,-7.29009223339221,
-7.83203303092207E-15));
#79673=CARTESIAN_POINT('Ctrl Pts',(-3.18652216952045,-7.38694978403964,
-6.44623243672982E-15));
#79674=CARTESIAN_POINT('Ctrl Pts',(-2.99883762064898,-7.48388259453305,
-5.05935505359788E-15));
#79675=CARTESIAN_POINT('Ctrl Pts',(-2.80740895502159,-7.57339073115159,
-1.95077283645645E-15));
#79676=CARTESIAN_POINT('Ctrl Pts',(-2.61265463314995,-7.65520051975289,
-4.70110061989715E-15));
#79677=CARTESIAN_POINT('Ctrl Pts',(-2.50764369183966,-7.69931211032946,
-7.77693376164546E-15));
#79678=CARTESIAN_POINT('Ctrl Pts',(-2.40166532647539,-7.74118482989975,
-1.74561535473132E-14));
#79679=CARTESIAN_POINT('Ctrl Pts',(-2.2947818331751,-7.78077040809537,-1.54546514474774E-14));
#79680=CARTESIAN_POINT('Ctrl Pts',(-2.23095371052338,-7.80440991558425,
-1.29169104133784E-14));
#79681=CARTESIAN_POINT('Ctrl Pts',(-2.16680276244212,-7.82723371232969,
-4.1499230043281E-15));
#79682=CARTESIAN_POINT('Ctrl Pts',(-2.10234495552166,-7.84924110414384,
5.60532523175006E-16));
#79683=CARTESIAN_POINT('Ctrl Pts',(-2.10208451021637,-7.84862588447229,
20.));
#79684=CARTESIAN_POINT('Ctrl Pts',(-2.29993845398409,-7.78098052187409,
20.));
#79685=CARTESIAN_POINT('Ctrl Pts',(-2.49472245171096,-7.70567498120029,
20.));
#79686=CARTESIAN_POINT('Ctrl Pts',(-2.68607054417264,-7.62302655375222,
20.));
#79687=CARTESIAN_POINT('Ctrl Pts',(-2.87904124585084,-7.53967727740421,
20.));
#79688=CARTESIAN_POINT('Ctrl Pts',(-3.06851811319142,-7.44885967635279,
20.));
#79689=CARTESIAN_POINT('Ctrl Pts',(-3.25410368317141,-7.35085088042121,
20.));
#79690=CARTESIAN_POINT('Ctrl Pts',(-3.43972446834445,-7.25282348714573,
20.));
#79691=CARTESIAN_POINT('Ctrl Pts',(-3.62145303987379,-7.14760173869536,
20.));
#79692=CARTESIAN_POINT('Ctrl Pts',(-3.79886106473171,-7.03542097986013,
20.));
#79693=CARTESIAN_POINT('Ctrl Pts',(-3.97379582767289,-6.92480414350723,
20.));
#79694=CARTESIAN_POINT('Ctrl Pts',(-4.14453011452454,-6.80742049724289,
20.));
#79695=CARTESIAN_POINT('Ctrl Pts',(-4.3106161353842,-6.68346179753878,20.));
#79696=CARTESIAN_POINT('Ctrl Pts',(-4.40985285404803,-6.60939623473704,
20.));
#79697=CARTESIAN_POINT('Ctrl Pts',(-4.50742935975488,-6.53298270634048,
20.));
#79698=CARTESIAN_POINT('Ctrl Pts',(-4.60324267526068,-6.4542572598369,20.));
#79699=CARTESIAN_POINT('Ctrl Pts',(-4.64330692333192,-6.42133828817218,
20.));
#79700=CARTESIAN_POINT('Ctrl Pts',(-4.68306280802542,-6.38801504068871,
20.));
#79701=CARTESIAN_POINT('Ctrl Pts',(-4.72250247928215,-6.35428998788552,
20.));
#79702=CARTESIAN_POINT('Ctrl Pts',(-4.74163073925796,-6.337933320673,20.));
#79703=CARTESIAN_POINT('Ctrl Pts',(-4.76068461484216,-6.32148213722302,
20.));
#79704=CARTESIAN_POINT('Ctrl Pts',(-4.77966319360128,-6.3049367117326,20.));
#79705=CARTESIAN_POINT('Ctrl Pts',(-4.79836161285379,-6.28863552783164,
20.));
#79706=CARTESIAN_POINT('Ctrl Pts',(-4.8169807385683,-6.27224825184192,20.));
#79707=CARTESIAN_POINT('Ctrl Pts',(-4.83551632979225,-6.25577849640647,
20.));
#79708=CARTESIAN_POINT('Ctrl Pts',(-4.90102249955029,-6.19757314528533,
20.));
#79709=CARTESIAN_POINT('Ctrl Pts',(-4.96549967896505,-6.1383253473394,20.));
#79710=CARTESIAN_POINT('Ctrl Pts',(-5.02891936957257,-6.07805489113583,
20.));
#79711=CARTESIAN_POINT('Ctrl Pts',(-5.16122131629022,-5.95232266808482,
20.));
#79712=CARTESIAN_POINT('Ctrl Pts',(-5.2889225499224,-5.8221413942123,20.));
#79713=CARTESIAN_POINT('Ctrl Pts',(-5.41174699713132,-5.6876741775399,20.));
#79714=CARTESIAN_POINT('Ctrl Pts',(-5.55047495102833,-5.5357959296903,20.));
#79715=CARTESIAN_POINT('Ctrl Pts',(-5.68298253274711,-5.37845008269323,
20.));
#79716=CARTESIAN_POINT('Ctrl Pts',(-5.80904649119039,-5.21607619935368,
20.));
#79717=CARTESIAN_POINT('Ctrl Pts',(-5.93507016833321,-5.05375419944903,
20.));
#79718=CARTESIAN_POINT('Ctrl Pts',(-6.05465463020608,-4.88640671026504,
20.));
#79719=CARTESIAN_POINT('Ctrl Pts',(-6.16753024467367,-4.71444998079642,
20.));
#79720=CARTESIAN_POINT('Ctrl Pts',(-6.2794284648384,-4.54398223128607,20.));
#79721=CARTESIAN_POINT('Ctrl Pts',(-6.38473373606294,-4.36898406647204,
20.));
#79722=CARTESIAN_POINT('Ctrl Pts',(-6.48313389007494,-4.18984837043746,
20.));
#79723=CARTESIAN_POINT('Ctrl Pts',(-6.51307646148177,-4.13533846215649,
20.));
#79724=CARTESIAN_POINT('Ctrl Pts',(-6.54237929342843,-4.08044538787204,
20.));
#79725=CARTESIAN_POINT('Ctrl Pts',(-6.57103262208241,-4.02518012273521,
20.));
#79726=CARTESIAN_POINT('Ctrl Pts',(-6.58804424164497,-3.99236886799811,
20.));
#79727=CARTESIAN_POINT('Ctrl Pts',(-6.60482744441781,-3.95942536090239,
20.));
#79728=CARTESIAN_POINT('Ctrl Pts',(-6.62137866989648,-3.92635476092985,
20.));
#79729=CARTESIAN_POINT('Ctrl Pts',(-6.63484032288851,-3.8994573603934,20.));
#79730=CARTESIAN_POINT('Ctrl Pts',(-6.64814497160758,-3.87248289700163,
20.));
#79731=CARTESIAN_POINT('Ctrl Pts',(-6.66128676665324,-3.84544327824432,
20.));
#79732=CARTESIAN_POINT('Ctrl Pts',(-6.74965857407903,-3.66361575975182,
20.));
#79733=CARTESIAN_POINT('Ctrl Pts',(-6.83074267432777,-3.47869940087201,
20.));
#79734=CARTESIAN_POINT('Ctrl Pts',(-6.90433376409663,-3.29111212276483,
20.));
#79735=CARTESIAN_POINT('Ctrl Pts',(-6.97742456607799,-3.10480010263551,
20.));
#79736=CARTESIAN_POINT('Ctrl Pts',(-7.04312408996378,-2.91585269867224,
20.));
#79737=CARTESIAN_POINT('Ctrl Pts',(-7.10118275135911,-2.72466342156463,
20.));
#79738=CARTESIAN_POINT('Ctrl Pts',(-7.14172675958846,-2.5911505323915,20.));
#79739=CARTESIAN_POINT('Ctrl Pts',(-7.17854360492222,-2.45654402833867,
20.));
#79740=CARTESIAN_POINT('Ctrl Pts',(-7.21153332547604,-2.32097579245235,
20.));
#79741=CARTESIAN_POINT('Ctrl Pts',(-7.25901033828673,-2.12587335557664,
20.));
#79742=CARTESIAN_POINT('Ctrl Pts',(-7.29856290209612,-1.92877846178032,
20.));
#79743=CARTESIAN_POINT('Ctrl Pts',(-7.33014858423521,-1.730178804948,20.));
#79744=CARTESIAN_POINT('Ctrl Pts',(-7.35985701969858,-1.54338261476073,
20.));
#79745=CARTESIAN_POINT('Ctrl Pts',(-7.38251695926489,-1.35525473159528,
20.));
#79746=CARTESIAN_POINT('Ctrl Pts',(-7.39805210559582,-1.16621056513693,
20.));
#79747=CARTESIAN_POINT('Ctrl Pts',(-7.40002520954372,-1.14220024793611,
20.));
#79748=CARTESIAN_POINT('Ctrl Pts',(-7.40188332922168,-1.11817516864935,
20.));
#79749=CARTESIAN_POINT('Ctrl Pts',(-7.40362626288781,-1.09413619608073,
20.));
#79750=CARTESIAN_POINT('Ctrl Pts',(-7.4091558560377,-1.01787067856313,20.));
#79751=CARTESIAN_POINT('Ctrl Pts',(-7.41351801792253,-0.941576962387156,
20.));
#79752=CARTESIAN_POINT('Ctrl Pts',(-7.41671582489737,-0.865287042356737,
20.));
#79753=CARTESIAN_POINT('Ctrl Pts',(-7.4249990299845,-0.667675035545347,
20.));
#79754=CARTESIAN_POINT('Ctrl Pts',(-7.42547448855069,-0.470077078890568,
20.));
#79755=CARTESIAN_POINT('Ctrl Pts',(-7.41816552412071,-0.272959537946737,
20.));
#79756=CARTESIAN_POINT('Ctrl Pts',(-7.41087952338355,-0.0764613113672781,
20.));
#79757=CARTESIAN_POINT('Ctrl Pts',(-7.3958578295149,0.119560215190561,20.));
#79758=CARTESIAN_POINT('Ctrl Pts',(-7.37307242525166,0.314636346146562,
20.));
#79759=CARTESIAN_POINT('Ctrl Pts',(-7.35064888899275,0.506614361774566,
20.));
#79760=CARTESIAN_POINT('Ctrl Pts',(-7.32070608982365,0.697677381348684,
20.));
#79761=CARTESIAN_POINT('Ctrl Pts',(-7.28317013661821,0.887362522537855,
20.));
#79762=CARTESIAN_POINT('Ctrl Pts',(-7.25381516542289,1.03570568103745,20.));
#79763=CARTESIAN_POINT('Ctrl Pts',(-7.21981527655707,1.18320590660905,20.));
#79764=CARTESIAN_POINT('Ctrl Pts',(-7.18111555074975,1.32963115529216,20.));
#79765=CARTESIAN_POINT('Ctrl Pts',(-7.17837251511031,1.34000977341598,20.));
#79766=CARTESIAN_POINT('Ctrl Pts',(-7.17560586053976,1.35038298620668,20.));
#79767=CARTESIAN_POINT('Ctrl Pts',(-7.17281556424333,1.36075070882595,20.));
#79768=CARTESIAN_POINT('Ctrl Pts',(-7.15343328756475,1.4327681747096,20.));
#79769=CARTESIAN_POINT('Ctrl Pts',(-7.13291033139403,1.50452079254417,20.));
#79770=CARTESIAN_POINT('Ctrl Pts',(-7.11125559528035,1.57598286207429,20.));
#79771=CARTESIAN_POINT('Ctrl Pts',(-7.09847134652633,1.6181717333011,20.));
#79772=CARTESIAN_POINT('Ctrl Pts',(-7.08529281884788,1.66025871253416,20.));
#79773=CARTESIAN_POINT('Ctrl Pts',(-7.07172104727107,1.70224044505357,20.));
#79774=CARTESIAN_POINT('Ctrl Pts',(-7.06082391348468,1.73594868669759,20.));
#79775=CARTESIAN_POINT('Ctrl Pts',(-7.04967416834453,1.76958585825288,20.));
#79776=CARTESIAN_POINT('Ctrl Pts',(-7.03828051620722,1.80312734962223,20.));
#79777=CARTESIAN_POINT('Ctrl Pts',(-6.97573795221415,1.98724486041761,20.));
#79778=CARTESIAN_POINT('Ctrl Pts',(-6.9057979512053,2.16864460803966,20.));
#79779=CARTESIAN_POINT('Ctrl Pts',(-6.82870273039878,2.34690919602424,20.));
#79780=CARTESIAN_POINT('Ctrl Pts',(-6.75168682671949,2.52499038178417,20.));
#79781=CARTESIAN_POINT('Ctrl Pts',(-6.66752999543998,2.69994345768324,20.));
#79782=CARTESIAN_POINT('Ctrl Pts',(-6.57643092848617,2.87132309777343,20.));
#79783=CARTESIAN_POINT('Ctrl Pts',(-6.53499184911887,2.94928014766549,20.));
#79784=CARTESIAN_POINT('Ctrl Pts',(-6.49211576930227,3.02649734441682,20.));
#79785=CARTESIAN_POINT('Ctrl Pts',(-6.4478188151391,3.10293025460452,20.));
#79786=CARTESIAN_POINT('Ctrl Pts',(-6.41797151466939,3.15443077149655,20.));
#79787=CARTESIAN_POINT('Ctrl Pts',(-6.38747890509194,3.20557549284086,20.));
#79788=CARTESIAN_POINT('Ctrl Pts',(-6.35634612436391,3.25634942223226,20.));
#79789=CARTESIAN_POINT('Ctrl Pts',(-6.3377211957493,3.2867245056101,20.));
#79790=CARTESIAN_POINT('Ctrl Pts',(-6.31886976855288,3.31696247069953,20.));
#79791=CARTESIAN_POINT('Ctrl Pts',(-6.29980107815861,3.34704799429116,20.));
#79792=CARTESIAN_POINT('Ctrl Pts',(-6.19740680540357,3.50860000677472,20.));
#79793=CARTESIAN_POINT('Ctrl Pts',(-6.08868419402615,3.66586865351991,20.));
#79794=CARTESIAN_POINT('Ctrl Pts',(-5.97383605057998,3.81843153287768,20.));
#79795=CARTESIAN_POINT('Ctrl Pts',(-5.86059869604879,3.96885465979773,20.));
#79796=CARTESIAN_POINT('Ctrl Pts',(-5.74140596609826,4.11470355191866,20.));
#79797=CARTESIAN_POINT('Ctrl Pts',(-5.61641870165742,4.25553580582496,20.));
#79798=CARTESIAN_POINT('Ctrl Pts',(-5.55718805385751,4.32227529058214,20.));
#79799=CARTESIAN_POINT('Ctrl Pts',(-5.49665565046419,4.38788757250809,20.));
#79800=CARTESIAN_POINT('Ctrl Pts',(-5.43483636697226,4.45232211452012,20.));
#79801=CARTESIAN_POINT('Ctrl Pts',(-5.39406120686288,4.49482226364363,20.));
#79802=CARTESIAN_POINT('Ctrl Pts',(-5.35272615103,4.53680998101336,20.));
#79803=CARTESIAN_POINT('Ctrl Pts',(-5.3108423268622,4.57827606387112,20.));
#79804=CARTESIAN_POINT('Origin',(0.,0.,20.));
#79805=CARTESIAN_POINT('',(-60.,43.,20.));
#79806=CARTESIAN_POINT('',(-60.,-40.,20.));
#79807=CARTESIAN_POINT('',(-60.,40.,20.));
#79808=CARTESIAN_POINT('',(60.,-40.,20.));
#79809=CARTESIAN_POINT('',(-60.,-40.,20.));
#79810=CARTESIAN_POINT('',(60.,43.,20.));
#79811=CARTESIAN_POINT('',(60.,-40.,20.));
#79812=CARTESIAN_POINT('',(30.,43.,20.));
#79813=CARTESIAN_POINT('',(29.,7.34788079488412E-16,20.));
#79814=CARTESIAN_POINT('Origin',(35.,0.,20.));
#79815=CARTESIAN_POINT('',(-41.,7.34788079488412E-16,20.));
#79816=CARTESIAN_POINT('Origin',(-35.,0.,20.));
#79817=CARTESIAN_POINT('Origin',(-35.,0.,10.));
#79818=CARTESIAN_POINT('',(-41.,7.34788079488412E-16,0.));
#79819=CARTESIAN_POINT('',(-41.,7.34788079488412E-16,10.));
#79820=CARTESIAN_POINT('Origin',(-35.,0.,0.));
#79821=CARTESIAN_POINT('Origin',(35.,0.,10.));
#79822=CARTESIAN_POINT('',(29.,7.34788079488412E-16,0.));
#79823=CARTESIAN_POINT('',(29.,7.34788079488412E-16,10.));
#79824=CARTESIAN_POINT('Origin',(35.,0.,0.));
#79825=CARTESIAN_POINT('Origin',(60.,43.,0.));
#79826=CARTESIAN_POINT('',(60.,43.,0.));
#79827=CARTESIAN_POINT('',(-60.,43.,0.));
#79828=CARTESIAN_POINT('',(30.,43.,0.));
#79829=CARTESIAN_POINT('',(-60.,43.,0.));
#79830=CARTESIAN_POINT('',(60.,43.,0.));
#79831=CARTESIAN_POINT('Origin',(60.,-40.,0.));
#79832=CARTESIAN_POINT('',(60.,-40.,0.));
#79833=CARTESIAN_POINT('',(60.,-40.,0.));
#79834=CARTESIAN_POINT('',(60.,-40.,0.));
#79835=CARTESIAN_POINT('Origin',(-60.,-40.,0.));
#79836=CARTESIAN_POINT('',(-60.,-40.,0.));
#79837=CARTESIAN_POINT('',(-60.,-40.,0.));
#79838=CARTESIAN_POINT('',(-60.,-40.,0.));
#79839=CARTESIAN_POINT('Origin',(-60.,40.,0.));
#79840=CARTESIAN_POINT('',(-60.,40.,0.));
#79841=CARTESIAN_POINT('Origin',(0.,0.,0.));
#79842=CARTESIAN_POINT('',(0.,0.,0.));
#79843=CARTESIAN_POINT('Origin',(15.,0.,8.20842344717745));
#79844=CARTESIAN_POINT('',(16.8723108164276,2.43738680900022,0.437234123991138));
#79845=CARTESIAN_POINT('',(16.8725886476928,2.43775122616105,0.354313353567125));
#79846=CARTESIAN_POINT('',(16.8723108164276,2.43738680900022,8.20842344717745));
#79847=CARTESIAN_POINT('',(15.7937992825328,-2.9692229537457,0.));
#79848=CARTESIAN_POINT('Ctrl Pts',(16.8725886476925,2.43775122616123,0.354313353567141));
#79849=CARTESIAN_POINT('Ctrl Pts',(17.0693981870995,2.2896606486941,0.341559014872585));
#79850=CARTESIAN_POINT('Ctrl Pts',(17.9852366821766,1.41166315331641,0.276129619930782));
#79851=CARTESIAN_POINT('Ctrl Pts',(18.4440669366553,-1.13346924859543,0.158025168741733));
#79852=CARTESIAN_POINT('Ctrl Pts',(16.7765145099754,-2.70650147589442,0.052675056247244));
#79853=CARTESIAN_POINT('Ctrl Pts',(15.7937992825328,-2.9692229537457,-1.11022302462516E-15));
#79854=CARTESIAN_POINT('',(14.2061995950377,-2.96922265367245,2.23034764090801E-5));
#79855=CARTESIAN_POINT('Origin',(15.,0.,0.));
#79856=CARTESIAN_POINT('Ctrl Pts',(16.8723108164276,2.43738680900022,0.437234123991137));
#79857=CARTESIAN_POINT('Ctrl Pts',(16.9486000539327,2.37878422526983,0.432252120409439));
#79858=CARTESIAN_POINT('Ctrl Pts',(17.0222149233757,2.3165352990722,0.427270116827742));
#79859=CARTESIAN_POINT('Ctrl Pts',(17.0927910606528,2.25091710785889,0.422288113246044));
#79860=CARTESIAN_POINT('Ctrl Pts',(17.1633209527764,2.18534191309508,0.417309374132041));
#79861=CARTESIAN_POINT('Ctrl Pts',(17.2308157490115,2.11640214016536,0.412330635018037));
#79862=CARTESIAN_POINT('Ctrl Pts',(17.2949445180178,2.0444148085015,0.407351895904035));
#79863=CARTESIAN_POINT('Ctrl Pts',(17.3590525920387,1.97245070785851,0.402374763478175));
#79864=CARTESIAN_POINT('Ctrl Pts',(17.4197965046981,1.89744133072467,0.397397631052316));
#79865=CARTESIAN_POINT('Ctrl Pts',(17.4768832401704,1.81973944963634,0.392420498626455));
#79866=CARTESIAN_POINT('Ctrl Pts',(17.5339672179588,1.74204132208603,0.387443606630499));
#79867=CARTESIAN_POINT('Ctrl Pts',(17.5873941096951,1.66165130397085,0.382466714634545));
#79868=CARTESIAN_POINT('Ctrl Pts',(17.6369128106088,1.57895315929483,0.377489822638589));
#79869=CARTESIAN_POINT('Ctrl Pts',(17.6864427073912,1.49623631708526,0.372511805398464));
#79870=CARTESIAN_POINT('Ctrl Pts',(17.7320624324359,1.4112106892341,0.367533788158336));
#79871=CARTESIAN_POINT('Ctrl Pts',(17.7735661748459,1.32428581648768,0.362555770918211));
#79872=CARTESIAN_POINT('Ctrl Pts',(17.8151160151883,1.23726439685972,0.357572224627246));
#79873=CARTESIAN_POINT('Ctrl Pts',(17.8525405583626,1.14833991940812,0.35258867833628));
#79874=CARTESIAN_POINT('Ctrl Pts',(17.8856817322189,1.05794290504634,0.347605132045315));
#79875=CARTESIAN_POINT('Ctrl Pts',(17.9188438701762,0.967488708276125,0.342618433314177));
#79876=CARTESIAN_POINT('Ctrl Pts',(17.9477171132732,0.875560539500225,0.337631734583041));
#79877=CARTESIAN_POINT('Ctrl Pts',(17.9721935807742,0.782603072064333,0.332645035851904));
#79878=CARTESIAN_POINT('Ctrl Pts',(17.9967089243288,0.689497959978504,0.327650416730842));
#79879=CARTESIAN_POINT('Ctrl Pts',(18.0168134609883,0.595360715303609,0.32265579760978));
#79880=CARTESIAN_POINT('Ctrl Pts',(18.0324506333514,0.500644990274309,0.317661178488717));
#79881=CARTESIAN_POINT('Ctrl Pts',(18.0393042270298,0.459132172020722,0.31547209409165));
#79882=CARTESIAN_POINT('Ctrl Pts',(18.0453003284032,0.417508278592077,0.313283009694582));
#79883=CARTESIAN_POINT('Ctrl Pts',(18.0504373294725,0.375811587049335,0.311093925297515));
#79884=CARTESIAN_POINT('Ctrl Pts',(18.0621939245159,0.280384097254954,0.306083963565994));
#79885=CARTESIAN_POINT('Ctrl Pts',(18.0694885112601,0.184240555982924,0.301074001834474));
#79886=CARTESIAN_POINT('Ctrl Pts',(18.0722447249927,0.0878327943001572,
0.296064040102953));
#79887=CARTESIAN_POINT('Ctrl Pts',(18.0749972100634,-0.00844454500551578,
0.291060855949365));
#79888=CARTESIAN_POINT('Ctrl Pts',(18.0732235131107,-0.104984961100177,
0.286057671795777));
#79889=CARTESIAN_POINT('Ctrl Pts',(18.0668988426675,-0.201329925357491,
0.281054487642189));
#79890=CARTESIAN_POINT('Ctrl Pts',(18.0605808432663,-0.297573268304245,
0.276056580672879));
#79891=CARTESIAN_POINT('Ctrl Pts',(18.0497214423724,-0.393621135526973,
0.27105867370357));
#79892=CARTESIAN_POINT('Ctrl Pts',(18.034347895094,-0.489014418538606,0.26606076673426));
#79893=CARTESIAN_POINT('Ctrl Pts',(18.0189855206538,-0.584338373782033,
0.261066492030504));
#79894=CARTESIAN_POINT('Ctrl Pts',(17.9991155921472,-0.679008260532783,
0.256072217326748));
#79895=CARTESIAN_POINT('Ctrl Pts',(17.9748171546814,-0.772570479770897,
0.251077942622992));
#79896=CARTESIAN_POINT('Ctrl Pts',(17.9505277471661,-0.86609792878083,0.246085523925564));
#79897=CARTESIAN_POINT('Ctrl Pts',(17.9218132108177,-0.958518105804558,
0.241093105228137));
#79898=CARTESIAN_POINT('Ctrl Pts',(17.888803417088,-1.04938890189513,0.236100686530709));
#79899=CARTESIAN_POINT('Ctrl Pts',(17.8557969816939,-1.14025045301321,0.231108775749746));
#79900=CARTESIAN_POINT('Ctrl Pts',(17.8184963072286,-1.22956252603547,0.226116864968781));
#79901=CARTESIAN_POINT('Ctrl Pts',(17.7770803885989,-1.3169004386282,0.221124954187818));
#79902=CARTESIAN_POINT('Ctrl Pts',(17.7356575060978,-1.40425303663708,0.216132204042997));
#79903=CARTESIAN_POINT('Ctrl Pts',(17.6901181924538,-1.48963042019004,0.211139453898177));
#79904=CARTESIAN_POINT('Ctrl Pts',(17.6406881541377,-1.57263101921493,0.206146703753356));
#79905=CARTESIAN_POINT('Ctrl Pts',(17.5912068526544,-1.65571769694263,0.201148775700653));
#79906=CARTESIAN_POINT('Ctrl Pts',(17.5378269948197,-1.73642229307496,0.19615084764795));
#79907=CARTESIAN_POINT('Ctrl Pts',(17.4808184105717,-1.81437103806483,0.191152919595247));
#79908=CARTESIAN_POINT('Ctrl Pts',(17.4237770906029,-1.89236454312705,0.186152121610241));
#79909=CARTESIAN_POINT('Ctrl Pts',(17.3631031686193,-1.96759870545471,0.181151323625236));
#79910=CARTESIAN_POINT('Ctrl Pts',(17.299106357257,-2.03973336689388,0.17615052564023));
#79911=CARTESIAN_POINT('Ctrl Pts',(17.2350100731102,-2.11198015010117,0.171141954716378));
#79912=CARTESIAN_POINT('Ctrl Pts',(17.1675808912483,-2.18111749990926,0.166133383792525));
#79913=CARTESIAN_POINT('Ctrl Pts',(17.0971648279345,-2.24684265903837,0.161124812868673));
#79914=CARTESIAN_POINT('Ctrl Pts',(17.0594111599379,-2.28208129238432,0.158439460764373));
#79915=CARTESIAN_POINT('Ctrl Pts',(17.0207994536887,-2.3163397556618,0.155754108660072));
#79916=CARTESIAN_POINT('Ctrl Pts',(16.9813866277332,-2.34957640468239,0.153068756555772));
#79917=CARTESIAN_POINT('Ctrl Pts',(16.9083021280413,-2.41120821631254,0.14808921981155));
#79918=CARTESIAN_POINT('Ctrl Pts',(16.8322081567229,-2.46953728502221,0.14310968306733));
#79919=CARTESIAN_POINT('Ctrl Pts',(16.7534369591403,-2.52425455933447,0.138130146323109));
#79920=CARTESIAN_POINT('Ctrl Pts',(16.6747707605681,-2.57889889760119,0.133157247111975));
#79921=CARTESIAN_POINT('Ctrl Pts',(16.5934347875804,-2.62994075769122,0.128184347900842));
#79922=CARTESIAN_POINT('Ctrl Pts',(16.5097952239559,-2.67711050046874,0.123211448689709));
#79923=CARTESIAN_POINT('Ctrl Pts',(16.4234649138133,-2.72579772869974,0.118078567639155));
#79924=CARTESIAN_POINT('Ctrl Pts',(16.3346806322611,-2.77035914660608,0.112945686588602));
#79925=CARTESIAN_POINT('Ctrl Pts',(16.2438787989889,-2.81054581592722,0.107812805538048));
#79926=CARTESIAN_POINT('Ctrl Pts',(16.1560574750195,-2.84941338476941,0.102848407866847));
#79927=CARTESIAN_POINT('Ctrl Pts',(16.066349421105,-2.88418872496296,0.097884010195645));
#79928=CARTESIAN_POINT('Ctrl Pts',(15.9751742796223,-2.91469335854789,0.0929196125244438));
#79929=CARTESIAN_POINT('Ctrl Pts',(15.884027995866,-2.94518833715058,0.0879567861283488));
#79930=CARTESIAN_POINT('Ctrl Pts',(15.7914159666675,-2.97141515424664,0.0829939597322541));
#79931=CARTESIAN_POINT('Ctrl Pts',(15.6977757461357,-2.99324426970216,0.0780311333361592));
#79932=CARTESIAN_POINT('Ctrl Pts',(15.6041390697955,-3.0150725589468,0.0730684947782371));
#79933=CARTESIAN_POINT('Ctrl Pts',(15.5094747109312,-3.0325033776651,0.0681058562203135));
#79934=CARTESIAN_POINT('Ctrl Pts',(15.4142321453266,-3.0454579261218,0.0631432176623914));
#79935=CARTESIAN_POINT('Ctrl Pts',(15.3189666441661,-3.05841559418966,0.0581793840413839));
#79936=CARTESIAN_POINT('Ctrl Pts',(15.2231230984729,-3.0668947920386,0.0532155504203748));
#79937=CARTESIAN_POINT('Ctrl Pts',(15.1271567394664,-3.07086851128606,0.048251716799367));
#79938=CARTESIAN_POINT('Ctrl Pts',(15.0310858171913,-3.07484656022861,0.0432824746719422));
#79939=CARTESIAN_POINT('Ctrl Pts',(14.9348922574478,-3.0743093170539,0.0383132325445207));
#79940=CARTESIAN_POINT('Ctrl Pts',(14.8390315762507,-3.06928190568342,0.0333439904170962));
#79941=CARTESIAN_POINT('Ctrl Pts',(14.7431081497739,-3.0642512036381,0.028371495689299));
#79942=CARTESIAN_POINT('Ctrl Pts',(14.6475184752423,-3.05472452826285,0.023399000961501));
#79943=CARTESIAN_POINT('Ctrl Pts',(14.5527111342476,-3.04077867010638,0.0184265062337037));
#79944=CARTESIAN_POINT('Ctrl Pts',(14.4577618030923,-3.02681192564914,0.013446564347092));
#79945=CARTESIAN_POINT('Ctrl Pts',(14.3635975760094,-3.00841287909547,0.00846662246047965));
#79946=CARTESIAN_POINT('Ctrl Pts',(14.2706547108404,-2.98570891065769,0.00348668057386803));
#79947=CARTESIAN_POINT('Ctrl Pts',(14.2491023085036,-2.98044411640452,0.00233188820804814));
#79948=CARTESIAN_POINT('Ctrl Pts',(14.2276155056363,-2.97494804394752,0.00117709584222782));
#79949=CARTESIAN_POINT('Ctrl Pts',(14.2061995950377,-2.96922265367245,2.23034764079699E-5));
#79950=CARTESIAN_POINT('Origin',(15.,0.,8.20842344717745));
#79951=CARTESIAN_POINT('',(16.8723108164276,2.43738680900023,1.43740555432678));
#79952=CARTESIAN_POINT('',(16.8723108164276,2.43738680900022,1.35414036795513));
#79953=CARTESIAN_POINT('',(16.8723108164276,2.43738680900022,8.20842344717745));
#79954=CARTESIAN_POINT('',(11.9270323372931,0.000383793694356834,0.708423426365591));
#79955=CARTESIAN_POINT('Ctrl Pts',(16.8723108164276,2.43738680900022,1.35414036795513));
#79956=CARTESIAN_POINT('Ctrl Pts',(16.9488467645666,2.37859471124328,1.34915700951272));
#79957=CARTESIAN_POINT('Ctrl Pts',(17.0226289554853,2.31618034982088,1.34417365107031));
#79958=CARTESIAN_POINT('Ctrl Pts',(17.0933051804222,2.25043899531123,1.3391902926279));
#79959=CARTESIAN_POINT('Ctrl Pts',(17.163985736743,2.18469361185065,1.33420662878097));
#79960=CARTESIAN_POINT('Ctrl Pts',(17.2315596282501,2.11562112957336,1.32922296493404));
#79961=CARTESIAN_POINT('Ctrl Pts',(17.2957104120883,2.04355473472801,1.32423930108711));
#79962=CARTESIAN_POINT('Ctrl Pts',(17.3601121879841,1.97120637773592,1.31923613849101));
#79963=CARTESIAN_POINT('Ctrl Pts',(17.4210637143198,1.89584096046158,1.31423297589491));
#79964=CARTESIAN_POINT('Ctrl Pts',(17.4782856482745,1.81782906114865,1.3092298132988));
#79965=CARTESIAN_POINT('Ctrl Pts',(17.535369363359,1.74000559860883,1.30423873577976));
#79966=CARTESIAN_POINT('Ctrl Pts',(17.5887412740794,1.65954881494975,1.29924765826073));
#79967=CARTESIAN_POINT('Ctrl Pts',(17.6381683823442,1.57685441192242,1.29425658074169));
#79968=CARTESIAN_POINT('Ctrl Pts',(17.6877750100846,1.49385966245803,1.28924737560705));
#79969=CARTESIAN_POINT('Ctrl Pts',(17.7334079269677,1.40861140609851,1.28423817047242));
#79970=CARTESIAN_POINT('Ctrl Pts',(17.7748794341556,1.32153182931781,1.27922896533778));
#79971=CARTESIAN_POINT('Ctrl Pts',(17.8163509413436,1.2344522525371,1.27421976020315));
#79972=CARTESIAN_POINT('Ctrl Pts',(17.8536609240355,1.14554178452447,1.26921055506852));
#79973=CARTESIAN_POINT('Ctrl Pts',(17.8866717782577,1.05523850129278,1.26420134993389));
#79974=CARTESIAN_POINT('Ctrl Pts',(17.9196220614258,0.965100914017152,1.25920133610442));
#79975=CARTESIAN_POINT('Ctrl Pts',(17.9484040181812,0.873260955603744,1.25420132227496));
#79976=CARTESIAN_POINT('Ctrl Pts',(17.9728410642138,0.78013989573926,1.24920130844549));
#79977=CARTESIAN_POINT('Ctrl Pts',(17.9972450936874,0.687144650466591,1.2442080500664));
#79978=CARTESIAN_POINT('Ctrl Pts',(18.0173157690538,0.592872164657343,1.23921479168731));
#79979=CARTESIAN_POINT('Ctrl Pts',(18.0329252006786,0.49776196830291,1.23422153330823));
#79980=CARTESIAN_POINT('Ctrl Pts',(18.0485182458185,0.402751616826001,1.22923351675694));
#79981=CARTESIAN_POINT('Ctrl Pts',(18.0596592868045,0.306905733810672,1.22424550020565));
#79982=CARTESIAN_POINT('Ctrl Pts',(18.0662709882578,0.210676236363457,1.21925748365436));
#79983=CARTESIAN_POINT('Ctrl Pts',(18.0728779987174,0.114515013622831,1.2142730060945));
#79984=CARTESIAN_POINT('Ctrl Pts',(18.0749620280716,0.0179711540885037,
1.20928852853464));
#79985=CARTESIAN_POINT('Ctrl Pts',(18.0724974312295,-0.0784970387206864,
1.20430405097478));
#79986=CARTESIAN_POINT('Ctrl Pts',(18.0700337215717,-0.174930505744737,
1.19932136768401));
#79987=CARTESIAN_POINT('Ctrl Pts',(18.0630246502553,-0.271287921906674,
1.19433868439324));
#79988=CARTESIAN_POINT('Ctrl Pts',(18.0514966819704,-0.367110678029874,
1.18935600110248));
#79989=CARTESIAN_POINT('Ctrl Pts',(18.0399697184903,-0.462925082017096,
1.18437375211406));
#79990=CARTESIAN_POINT('Ctrl Pts',(18.0239246937907,-0.558204482949211,
1.17939150312564));
#79991=CARTESIAN_POINT('Ctrl Pts',(18.0034398632507,-0.652496159250288,
1.17440925413723));
#79992=CARTESIAN_POINT('Ctrl Pts',(17.9829512298507,-0.746805340116538,
1.16942608023046));
#79993=CARTESIAN_POINT('Ctrl Pts',(17.9580212468915,-0.840126003369507,
1.16444290632369));
#79994=CARTESIAN_POINT('Ctrl Pts',(17.9287788876878,-0.932017423138756,
1.15945973241692));
#79995=CARTESIAN_POINT('Ctrl Pts',(17.8995050420624,-1.02400778608743,1.15447119292682));
#79996=CARTESIAN_POINT('Ctrl Pts',(17.8659096838051,-1.11456541446941,1.14948265343671));
#79997=CARTESIAN_POINT('Ctrl Pts',(17.8281710387483,-1.20326673085614,1.14449411394661));
#79998=CARTESIAN_POINT('Ctrl Pts',(17.7904099793551,-1.29202073013984,1.13950261158378));
#79999=CARTESIAN_POINT('Ctrl Pts',(17.7485009237813,-1.37891582706822,1.13451110922094));
#80000=CARTESIAN_POINT('Ctrl Pts',(17.7026685033149,-1.46355225775839,1.12951960685811));
#80001=CARTESIAN_POINT('Ctrl Pts',(17.6567625502343,-1.54832447743685,1.1245200962292));
#80002=CARTESIAN_POINT('Ctrl Pts',(17.606920890662,-1.63083042003146,1.1195205856003));
#80003=CARTESIAN_POINT('Ctrl Pts',(17.5534119272192,-1.71069862335089,1.1145210749714));
#80004=CARTESIAN_POINT('Ctrl Pts',(17.5236405722932,-1.75513575080276,1.11173944371165));
#80005=CARTESIAN_POINT('Ctrl Pts',(17.4927347077816,-1.79875691118914,1.10895781245189));
#80006=CARTESIAN_POINT('Ctrl Pts',(17.4607457862635,-1.84150276279636,1.10617618119214));
#80007=CARTESIAN_POINT('Ctrl Pts',(17.4032237856212,-1.91836771437699,1.10117429342861));
#80008=CARTESIAN_POINT('Ctrl Pts',(17.3419966626954,-1.99266879379093,1.09617240566508));
#80009=CARTESIAN_POINT('Ctrl Pts',(17.2773210991351,-2.06402782477227,1.09117051790155));
#80010=CARTESIAN_POINT('Ctrl Pts',(17.2127329198155,-2.13529044136784,1.08617538827261));
#80011=CARTESIAN_POINT('Ctrl Pts',(17.1447058520614,-2.20361858776218,1.08118025864368));
#80012=CARTESIAN_POINT('Ctrl Pts',(17.0735384616154,-2.26866491536356,1.07618512901475));
#80013=CARTESIAN_POINT('Ctrl Pts',(17.0024458265917,-2.3336429172099,1.07119524635388));
#80014=CARTESIAN_POINT('Ctrl Pts',(16.9282197485466,-2.39534565917475,1.06620536369302));
#80015=CARTESIAN_POINT('Ctrl Pts',(16.8511967750666,-2.45346138139225,1.06121548103215));
#80016=CARTESIAN_POINT('Ctrl Pts',(16.7742286640186,-2.51153570855939,1.05622915259785));
#80017=CARTESIAN_POINT('Ctrl Pts',(16.6944679670887,-2.5660278319904,1.05124282416355));
#80018=CARTESIAN_POINT('Ctrl Pts',(16.6122848086959,-2.61666580702399,1.04625649572925));
#80019=CARTESIAN_POINT('Ctrl Pts',(16.5301313896643,-2.6672854578527,1.04127197168195));
#80020=CARTESIAN_POINT('Ctrl Pts',(16.4455576238991,-2.71405350170774,1.03628744763464));
#80021=CARTESIAN_POINT('Ctrl Pts',(16.3589623533002,-2.75674147723588,1.03130292358734));
#80022=CARTESIAN_POINT('Ctrl Pts',(16.2723748417191,-2.79942562788127,1.02631884615808));
#80023=CARTESIAN_POINT('Ctrl Pts',(16.1837665788222,-2.83803024338459,1.02133476872883));
#80024=CARTESIAN_POINT('Ctrl Pts',(16.0935597661888,-2.87237345896613,1.01635069129957));
#80025=CARTESIAN_POINT('Ctrl Pts',(16.0033364763351,-2.90672294769616,1.0113657034763));
#80026=CARTESIAN_POINT('Ctrl Pts',(15.9115144666329,-2.93680933462643,1.00638071565303));
#80027=CARTESIAN_POINT('Ctrl Pts',(15.8185336006982,-2.96249978810598,1.00139572782976));
#80028=CARTESIAN_POINT('Ctrl Pts',(15.7254532699317,-2.98821772354768,0.996405407393469));
#80029=CARTESIAN_POINT('Ctrl Pts',(15.6312120314289,-3.00953022070407,0.991415086957177));
#80030=CARTESIAN_POINT('Ctrl Pts',(15.5362622950073,-3.02635506855252,0.986424766520887));
#80031=CARTESIAN_POINT('Ctrl Pts',(15.4412564901616,-3.04318985158078,0.981431499268601));
#80032=CARTESIAN_POINT('Ctrl Pts',(15.345541788988,-3.05553165254109,0.976438232016316));
#80033=CARTESIAN_POINT('Ctrl Pts',(15.2495760194569,-3.06335013678033,0.97144496476403));
#80034=CARTESIAN_POINT('Ctrl Pts',(15.1534571521734,-3.07118109413753,0.966443731567249));
#80035=CARTESIAN_POINT('Ctrl Pts',(15.0570868546531,-3.07447431111347,0.961442498370468));
#80036=CARTESIAN_POINT('Ctrl Pts',(14.9609231734083,-3.07325157636395,0.956441265173687));
#80037=CARTESIAN_POINT('Ctrl Pts',(14.90778819723,-3.07257595765898,0.953677847599264));
#80038=CARTESIAN_POINT('Ctrl Pts',(14.8547162292643,-3.07052250404811,0.95091443002484));
#80039=CARTESIAN_POINT('Ctrl Pts',(14.8017835398299,-3.0671016424171,0.948151012450417));
#80040=CARTESIAN_POINT('Ctrl Pts',(14.7059710668605,-3.06090960464127,0.943149001887909));
#80041=CARTESIAN_POINT('Ctrl Pts',(14.6102826025438,-3.05021291769368,0.938146991325403));
#80042=CARTESIAN_POINT('Ctrl Pts',(14.5151751784807,-3.03502012224611,0.933144980762894));
#80043=CARTESIAN_POINT('Ctrl Pts',(14.4201959021657,-3.0198477975719,0.928149709909677));
#80044=CARTESIAN_POINT('Ctrl Pts',(14.3257965394092,-3.00019147337784,0.923154439056459));
#80045=CARTESIAN_POINT('Ctrl Pts',(14.232431163035,-2.97611161257776,0.918159168203242));
#80046=CARTESIAN_POINT('Ctrl Pts',(14.1391635207521,-2.95205695837359,0.91316912635757));
#80047=CARTESIAN_POINT('Ctrl Pts',(14.0469281354202,-2.92358808199884,0.908179084511899));
#80048=CARTESIAN_POINT('Ctrl Pts',(13.9561700024301,-2.89081669881942,0.903189042666227));
#80049=CARTESIAN_POINT('Ctrl Pts',(13.8654760443595,-2.85806848822858,0.898202529270548));
#80050=CARTESIAN_POINT('Ctrl Pts',(13.7762576732555,-2.82102396739934,0.893216015874868));
#80051=CARTESIAN_POINT('Ctrl Pts',(13.6889448638851,-2.77984472229418,0.888229502479189));
#80052=CARTESIAN_POINT('Ctrl Pts',(13.6016633716216,-2.73868024724197,0.883244777631761));
#80053=CARTESIAN_POINT('Ctrl Pts',(13.5162864791779,-2.69338418149762,0.878260052784337));
#80054=CARTESIAN_POINT('Ctrl Pts',(13.4332234124963,-2.64416591288258,0.873275327936909));
#80055=CARTESIAN_POINT('Ctrl Pts',(13.3501675300782,-2.59495190123789,0.868291034226667));
#80056=CARTESIAN_POINT('Ctrl Pts',(13.2694254525897,-2.54181658491102,0.863306740516423));
#80057=CARTESIAN_POINT('Ctrl Pts',(13.1913801241305,-2.48501436507108,0.858322446806182));
#80058=CARTESIAN_POINT('Ctrl Pts',(13.1133203034898,-2.42820159766742,0.853337227565992));
#80059=CARTESIAN_POINT('Ctrl Pts',(13.0379585808719,-2.36772083244518,0.848352008325803));
#80060=CARTESIAN_POINT('Ctrl Pts',(12.9656464668122,-2.30386804136134,0.843366789085613));
#80061=CARTESIAN_POINT('Ctrl Pts',(12.8932566914509,-2.23994667406553,0.838376215851565));
#80062=CARTESIAN_POINT('Ctrl Pts',(12.823923392296,-2.17264634182216,0.833385642617515));
#80063=CARTESIAN_POINT('Ctrl Pts',(12.7579625247845,-2.10230117008223,0.828395069383467));
#80064=CARTESIAN_POINT('Ctrl Pts',(12.6919625443282,-2.03191428562805,0.823401536879435));
#80065=CARTESIAN_POINT('Ctrl Pts',(12.6293392617936,-1.95847929996441,0.818408004375404));
#80066=CARTESIAN_POINT('Ctrl Pts',(12.5703681319383,-1.88236320504285,0.813414471871371));
#80067=CARTESIAN_POINT('Ctrl Pts',(12.5113027306581,-1.80612543070379,0.808412956691309));
#80068=CARTESIAN_POINT('Ctrl Pts',(12.4559013912022,-1.72719834772307,0.803411441511248));
#80069=CARTESIAN_POINT('Ctrl Pts',(12.4043960227106,-1.64597759495063,0.798409926331186));
#80070=CARTESIAN_POINT('Ctrl Pts',(12.3759596580807,-1.60113522202919,0.795648565457015));
#80071=CARTESIAN_POINT('Ctrl Pts',(12.3487100495383,-1.55559413528145,0.792887204582844));
#80072=CARTESIAN_POINT('Ctrl Pts',(12.3226800398894,-1.50942375799289,0.790125843708672));
#80073=CARTESIAN_POINT('Ctrl Pts',(12.2735423910071,-1.42226651838476,0.784913137954711));
#80074=CARTESIAN_POINT('Ctrl Pts',(12.2285939954989,-1.33258274597609,0.779700432200751));
#80075=CARTESIAN_POINT('Ctrl Pts',(12.188090757582,-1.24079356155826,0.77448772644679));
#80076=CARTESIAN_POINT('Ctrl Pts',(12.1476603528802,-1.14916943311491,0.76928439421797));
#80077=CARTESIAN_POINT('Ctrl Pts',(12.1116593496754,-1.0554477792978,0.76408106198915));
#80078=CARTESIAN_POINT('Ctrl Pts',(12.0802982731441,-0.960075036752079,
0.75887772976033));
#80079=CARTESIAN_POINT('Ctrl Pts',(12.0490053639031,-0.864909598998068,
0.753685707636213));
#80080=CARTESIAN_POINT('Ctrl Pts',(12.0223324057197,-0.76810058798344,0.748493685512095));
#80081=CARTESIAN_POINT('Ctrl Pts',(12.0004417921737,-0.670114026015082,
0.743301663387977));
#80082=CARTESIAN_POINT('Ctrl Pts',(11.9785799823023,-0.572256394787969,
0.73811647292779));
#80083=CARTESIAN_POINT('Ctrl Pts',(11.961488078542,-0.473224670510129,0.732931282467602));
#80084=CARTESIAN_POINT('Ctrl Pts',(11.9492787988412,-0.373500204551646,
0.727746092007415));
#80085=CARTESIAN_POINT('Ctrl Pts',(11.9370878120961,-0.273925154061226,
0.722568670429739));
#80086=CARTESIAN_POINT('Ctrl Pts',(11.9297649225634,-0.173659811268035,
0.717391248852062));
#80087=CARTESIAN_POINT('Ctrl Pts',(11.927371687701,-0.0731949756367123,
0.712213827274386));
#80088=CARTESIAN_POINT('Ctrl Pts',(11.9267876601978,-0.048678273149109,
0.710950367242076));
#80089=CARTESIAN_POINT('Ctrl Pts',(11.9264969631059,-0.0241497297134993,
0.709686907209766));
#80090=CARTESIAN_POINT('Ctrl Pts',(11.9265000239204,0.000383456645624363,
0.708423447177456));
#80091=CARTESIAN_POINT('Ctrl Pts',(11.93146095593,0.00038659779505148,0.708423253219806));
#80092=CARTESIAN_POINT('Ctrl Pts',(11.9310937115442,0.493586194944426,0.682982393802185));
#80093=CARTESIAN_POINT('Ctrl Pts',(12.275455933301,2.00734761848573,0.604866478137318));
#80094=CARTESIAN_POINT('Ctrl Pts',(14.4123128401962,3.45239818247855,0.486829844919761));
#80095=CARTESIAN_POINT('Ctrl Pts',(16.256580383956,2.90127052393581,0.394234071119828));
#80096=CARTESIAN_POINT('Ctrl Pts',(16.8725886476925,2.43775122616123,0.354313353567141));
#80097=CARTESIAN_POINT('',(11.9265000946077,0.000762596727450985,0.791576552865784));
#80098=CARTESIAN_POINT('Ctrl Pts',(11.9265000946079,0.000762597557556419,
0.791576552822547));
#80099=CARTESIAN_POINT('Ctrl Pts',(11.9265102684111,0.0417661159950146,
0.789440845722602));
#80100=CARTESIAN_POINT('Ctrl Pts',(11.9273409490568,0.0827585467976382,
0.787305138622661));
#80101=CARTESIAN_POINT('Ctrl Pts',(11.9289910136247,0.123717644668866,0.785169431522718));
#80102=CARTESIAN_POINT('Ctrl Pts',(11.9328555153485,0.219645105569208,0.780167540124415));
#80103=CARTESIAN_POINT('Ctrl Pts',(11.9412257044201,0.315558408633647,0.77516564872611));
#80104=CARTESIAN_POINT('Ctrl Pts',(11.9541042636064,0.411000502456114,0.770163757327807));
#80105=CARTESIAN_POINT('Ctrl Pts',(11.9669654222801,0.506313642307278,0.765168624098085));
#80106=CARTESIAN_POINT('Ctrl Pts',(11.9843227863911,0.601156407398729,0.760173490868364));
#80107=CARTESIAN_POINT('Ctrl Pts',(12.00612705987,0.695073426594247,0.755178357638643));
#80108=CARTESIAN_POINT('Ctrl Pts',(12.0279084296238,0.78889179312916,0.750188471415134));
#80109=CARTESIAN_POINT('Ctrl Pts',(12.0541273238847,0.881785922065945,0.745198585191627));
#80110=CARTESIAN_POINT('Ctrl Pts',(12.0846829867416,0.973308256518122,0.740208698968118));
#80111=CARTESIAN_POINT('Ctrl Pts',(12.1152168847939,1.0647653995936,0.73522236704154));
#80112=CARTESIAN_POINT('Ctrl Pts',(12.1500812718183,1.15485227599997,0.730236035114959));
#80113=CARTESIAN_POINT('Ctrl Pts',(12.1891251681878,1.24313512133021,0.725249703188382));
#80114=CARTESIAN_POINT('Ctrl Pts',(12.2281549355248,1.33138601925478,0.720265175693552));
#80115=CARTESIAN_POINT('Ctrl Pts',(12.271361029811,1.41783378265897,0.715280648198722));
#80116=CARTESIAN_POINT('Ctrl Pts',(12.3185441745335,1.50206421502933,0.710296120703892));
#80117=CARTESIAN_POINT('Ctrl Pts',(12.365723091145,1.58628709945819,0.705312039875675));
#80118=CARTESIAN_POINT('Ctrl Pts',(12.4168781351221,1.66829266547198,0.700327959047457));
#80119=CARTESIAN_POINT('Ctrl Pts',(12.471764384952,1.74769188497363,0.69534387821924));
#80120=CARTESIAN_POINT('Ctrl Pts',(12.526660659747,1.82710560673066,0.690358887049416));
#80121=CARTESIAN_POINT('Ctrl Pts',(12.5852892445217,1.90391167586761,0.685373895879593));
#80122=CARTESIAN_POINT('Ctrl Pts',(12.6473628880279,1.97775146804938,0.680388904709768));
#80123=CARTESIAN_POINT('Ctrl Pts',(12.7095029325691,2.05167024767821,0.675398581025936));
#80124=CARTESIAN_POINT('Ctrl Pts',(12.7750951102901,2.12261607957009,0.670408257342104));
#80125=CARTESIAN_POINT('Ctrl Pts',(12.8438131569517,2.19026494923906,0.665417933658272));
#80126=CARTESIAN_POINT('Ctrl Pts',(12.9125717813246,2.25795376527506,0.660424663209736));
#80127=CARTESIAN_POINT('Ctrl Pts',(12.9844596236029,2.32234145009085,0.6554313927612));
#80128=CARTESIAN_POINT('Ctrl Pts',(13.059116569471,2.38314367151833,0.650438122312663));
#80129=CARTESIAN_POINT('Ctrl Pts',(13.1338926166026,2.44404289157491,0.645436886030366));
#80130=CARTESIAN_POINT('Ctrl Pts',(13.2114462355921,2.50134496681132,0.640435649748068));
#80131=CARTESIAN_POINT('Ctrl Pts',(13.2913876071823,2.55480839616396,0.635434413465771));
#80132=CARTESIAN_POINT('Ctrl Pts',(13.3355584200923,2.5843490844019,0.632671029904176));
#80133=CARTESIAN_POINT('Ctrl Pts',(13.3804577527622,2.61271863442847,0.629907646342582));
#80134=CARTESIAN_POINT('Ctrl Pts',(13.4260168470823,2.63988243759665,0.627144262780988));
#80135=CARTESIAN_POINT('Ctrl Pts',(13.5084837698325,2.68905187985409,0.622142237562878));
#80136=CARTESIAN_POINT('Ctrl Pts',(13.5934001254049,2.73443876140458,0.617140212344768));
#80137=CARTESIAN_POINT('Ctrl Pts',(13.6803844323884,2.77579123921758,0.612138187126659));
#80138=CARTESIAN_POINT('Ctrl Pts',(13.7672515386383,2.81708799961554,0.607142901526823));
#80139=CARTESIAN_POINT('Ctrl Pts',(13.8561806658599,2.85436097341372,0.602147615926989));
#80140=CARTESIAN_POINT('Ctrl Pts',(13.9467633602653,2.88740278290375,0.597152330327153));
#80141=CARTESIAN_POINT('Ctrl Pts',(14.0372512350179,2.92041000507086,0.5921622736648));
#80142=CARTESIAN_POINT('Ctrl Pts',(14.1293888261519,2.94919471850926,0.587172217002445));
#80143=CARTESIAN_POINT('Ctrl Pts',(14.2227461292744,2.97359692467593,0.582182160340092));
#80144=CARTESIAN_POINT('Ctrl Pts',(14.3160374205969,2.99798187634294,0.57719563208539));
#80145=CARTESIAN_POINT('Ctrl Pts',(14.4105462863825,3.0179903706246,0.57220910383069));
#80146=CARTESIAN_POINT('Ctrl Pts',(14.5058268521429,3.03351201578913,0.567222575575988));
#80147=CARTESIAN_POINT('Ctrl Pts',(14.6010732434356,3.04902809377469,0.562237835849172));
#80148=CARTESIAN_POINT('Ctrl Pts',(14.6970903524384,3.0600604498773,0.557253096122355));
#80149=CARTESIAN_POINT('Ctrl Pts',(14.7934223269749,3.06654983898966,0.55226835639554));
#80150=CARTESIAN_POINT('Ctrl Pts',(14.88974596966,3.0730386668281,0.547284047803976));
#80151=CARTESIAN_POINT('Ctrl Pts',(14.9863839862799,3.07498527967503,0.542299739212411));
#80152=CARTESIAN_POINT('Ctrl Pts',(15.0828766862315,3.07238241514289,0.537315430620848));
#80153=CARTESIAN_POINT('Ctrl Pts',(15.1793873034701,3.06977906729678,0.532330196515882));
#80154=CARTESIAN_POINT('Ctrl Pts',(15.2757521121938,3.0626245761527,0.52734496241092));
#80155=CARTESIAN_POINT('Ctrl Pts',(15.3715137788867,3.05096374316335,0.522359728305954));
#80156=CARTESIAN_POINT('Ctrl Pts',(15.4673782885559,3.03929038705477,0.517369140322651));
#80157=CARTESIAN_POINT('Ctrl Pts',(15.5626379271535,3.02310108065177,0.512378552339349));
#80158=CARTESIAN_POINT('Ctrl Pts',(15.6568430504918,3.00249220765361,0.507387964356046));
#80159=CARTESIAN_POINT('Ctrl Pts',(15.7511040338299,2.98187111438971,0.502394417146811));
#80160=CARTESIAN_POINT('Ctrl Pts',(15.8443088336417,2.95682535001433,0.497400869937575));
#80161=CARTESIAN_POINT('Ctrl Pts',(15.9360225654421,2.9275013248474,0.49240732272834));
#80162=CARTESIAN_POINT('Ctrl Pts',(16.0278829067494,2.89813042359346,0.487405793055847));
#80163=CARTESIAN_POINT('Ctrl Pts',(16.1182470102679,2.86446775891739,0.482404263383352));
#80164=CARTESIAN_POINT('Ctrl Pts',(16.2066996507123,2.82670801516018,0.477402733710859));
#80165=CARTESIAN_POINT('Ctrl Pts',(16.2555320312988,2.80586185196218,0.474641520486987));
#80166=CARTESIAN_POINT('Ctrl Pts',(16.3037822453033,2.78376778355852,0.471880307263116));
#80167=CARTESIAN_POINT('Ctrl Pts',(16.3513839134321,2.76046441174612,0.469119094039244));
#80168=CARTESIAN_POINT('Ctrl Pts',(16.4374993846867,2.71830662769506,0.464123824180957));
#80169=CARTESIAN_POINT('Ctrl Pts',(16.5217927731749,2.67204060736011,0.459128554322671));
#80170=CARTESIAN_POINT('Ctrl Pts',(16.6038453090492,2.62184714936641,0.454133284464384));
#80171=CARTESIAN_POINT('Ctrl Pts',(16.6857774726772,2.57172732589509,0.449145342738585));
#80172=CARTESIAN_POINT('Ctrl Pts',(16.7654749475324,2.51769174789098,0.444157401012784));
#80173=CARTESIAN_POINT('Ctrl Pts',(16.842541521382,2.4599680875945,0.439169459286985));
#80174=CARTESIAN_POINT('Ctrl Pts',(16.8525088698863,2.45250244055218,0.438524347521702));
#80175=CARTESIAN_POINT('Ctrl Pts',(16.8624322437064,2.44497516489369,0.43787923575642));
#80176=CARTESIAN_POINT('Ctrl Pts',(16.8723108164276,2.43738680900022,0.437234123991137));
#80177=CARTESIAN_POINT('Ctrl Pts',(16.8723108164276,2.43738680900023,1.43740555432678));
#80178=CARTESIAN_POINT('Ctrl Pts',(16.9487418871335,2.37867527422642,1.43240470324732));
#80179=CARTESIAN_POINT('Ctrl Pts',(17.0223095105188,2.31644150982458,1.42740385216786));
#80180=CARTESIAN_POINT('Ctrl Pts',(17.0926908320212,2.251010291308,1.4224030010884));
#80181=CARTESIAN_POINT('Ctrl Pts',(17.1167707269066,2.22862399860322,1.42069203622215));
#80182=CARTESIAN_POINT('Ctrl Pts',(17.1404779828383,2.20586372150002,1.41898107135591));
#80183=CARTESIAN_POINT('Ctrl Pts',(17.163800751531,2.1827433558882,1.41727010648966));
#80184=CARTESIAN_POINT('Ctrl Pts',(17.2319678784332,2.11516780697037,1.41226934690146));
#80185=CARTESIAN_POINT('Ctrl Pts',(17.2970853426487,2.04427799071225,1.40726858731326));
#80186=CARTESIAN_POINT('Ctrl Pts',(17.3588141257413,1.97038020955432,1.40226782772507));
#80187=CARTESIAN_POINT('Ctrl Pts',(17.4204595366264,1.89658223631145,1.39727382226914));
#80188=CARTESIAN_POINT('Ctrl Pts',(17.4787250838348,1.81978470635024,1.39227981681321));
#80189=CARTESIAN_POINT('Ctrl Pts',(17.533308060935,1.74033115193675,1.38728581135728));
#80190=CARTESIAN_POINT('Ctrl Pts',(17.5878337497707,1.66096098902162,1.38229704742391));
#80191=CARTESIAN_POINT('Ctrl Pts',(17.6386843051097,1.57894070316164,1.37730828349053));
#80192=CARTESIAN_POINT('Ctrl Pts',(17.6855975113525,1.49464653246751,1.37231951955716));
#80193=CARTESIAN_POINT('Ctrl Pts',(17.7324774131216,1.41041220362208,1.36733429723116));
#80194=CARTESIAN_POINT('Ctrl Pts',(17.7754253098421,1.32390758132023,1.36234907490517));
#80195=CARTESIAN_POINT('Ctrl Pts',(17.814223055485,1.23553666233609,1.35736385257917));
#80196=CARTESIAN_POINT('Ctrl Pts',(17.853006822366,1.14719758324431,1.35238042642033));
#80197=CARTESIAN_POINT('Ctrl Pts',(17.8876432330553,1.05699394482163,1.34739700026148));
#80198=CARTESIAN_POINT('Ctrl Pts',(17.917961175185,0.965352179317362,1.34241357410264));
#80199=CARTESIAN_POINT('Ctrl Pts',(17.9482764581108,0.873718451764499,1.33743058504294));
#80200=CARTESIAN_POINT('Ctrl Pts',(17.9742738879916,0.780647264485796,1.33244759598325));
#80201=CARTESIAN_POINT('Ctrl Pts',(17.9958317302719,0.686581745967842,1.32746460692355));
#80202=CARTESIAN_POINT('Ctrl Pts',(18.0173935580156,0.592498837272972,1.32248069664359));
#80203=CARTESIAN_POINT('Ctrl Pts',(18.0345140701432,0.497421659861666,1.31749678636364));
#80204=CARTESIAN_POINT('Ctrl Pts',(18.0471225362022,0.401804055938678,1.31251287608368));
#80205=CARTESIAN_POINT('Ctrl Pts',(18.059744550821,0.306083705114281,1.30752361029054));
#80206=CARTESIAN_POINT('Ctrl Pts',(18.0678447826611,0.209822204081699,1.3025343444974));
#80207=CARTESIAN_POINT('Ctrl Pts',(18.0714043704515,0.113478822566934,1.29754507870427));
#80208=CARTESIAN_POINT('Ctrl Pts',(18.0749660687942,0.0170783170949871,
1.29255285467361));
#80209=CARTESIAN_POINT('Ctrl Pts',(18.0739817668327,-0.0794037270874671,
1.28756063064296));
#80210=CARTESIAN_POINT('Ctrl Pts',(18.0684847305754,-0.175509852218593,
1.28256840661231));
#80211=CARTESIAN_POINT('Ctrl Pts',(18.0629788920172,-0.271769870280725,
1.27756818862719));
#80212=CARTESIAN_POINT('Ctrl Pts',(18.052945936315,-0.367652331417721,1.27256797064207));
#80213=CARTESIAN_POINT('Ctrl Pts',(18.0384707819403,-0.462706772476012,
1.26756775265695));
#80214=CARTESIAN_POINT('Ctrl Pts',(18.0304395300363,-0.515445841156773,
1.26479348102061));
#80215=CARTESIAN_POINT('Ctrl Pts',(18.0210417158762,-0.567930216229394,
1.26201920938427));
#80216=CARTESIAN_POINT('Ctrl Pts',(18.0102984817983,-0.620084913929582,
1.25924493774793));
#80217=CARTESIAN_POINT('Ctrl Pts',(17.99093241947,-0.714100470050287,1.25424395601049));
#80218=CARTESIAN_POINT('Ctrl Pts',(17.9671240151282,-0.807371905796901,
1.24924297427306));
#80219=CARTESIAN_POINT('Ctrl Pts',(17.9389446606578,-0.899447903767208,
1.24424199253562));
#80220=CARTESIAN_POINT('Ctrl Pts',(17.9108033673361,-0.991399536991763,
1.23924776549904));
#80221=CARTESIAN_POINT('Ctrl Pts',(17.8783029846973,-1.08215852561021,1.23425353846245));
#80222=CARTESIAN_POINT('Ctrl Pts',(17.8415659243467,-1.17128363242723,1.22925931142587));
#80223=CARTESIAN_POINT('Ctrl Pts',(17.8048674264319,-1.26031518572674,1.22427032676737));
#80224=CARTESIAN_POINT('Ctrl Pts',(17.7639412580249,-1.34771586332309,1.21928134210886));
#80225=CARTESIAN_POINT('Ctrl Pts',(17.7189593437629,-1.43306047917184,1.21429235745036));
#80226=CARTESIAN_POINT('Ctrl Pts',(17.6740093810356,-1.51834447306863,1.20930691656536));
#80227=CARTESIAN_POINT('Ctrl Pts',(17.6250096035478,-1.60157492164121,1.20432147568036));
#80228=CARTESIAN_POINT('Ctrl Pts',(17.5721792599945,-1.68234838973802,1.19933603479537));
#80229=CARTESIAN_POINT('Ctrl Pts',(17.5193679653499,-1.76309273354149,1.19435239149869));
#80230=CARTESIAN_POINT('Ctrl Pts',(17.462729088836,-1.8413814903884,1.18936874820201));
#80231=CARTESIAN_POINT('Ctrl Pts',(17.4025263638967,-1.91683836584653,1.18438510490533));
#80232=CARTESIAN_POINT('Ctrl Pts',(17.3423289394216,-1.9922885978103,1.17940190038651));
#80233=CARTESIAN_POINT('Ctrl Pts',(17.2785685641232,-2.06490710135893,1.17441869586768));
#80234=CARTESIAN_POINT('Ctrl Pts',(17.2115499297707,-2.13434982093642,1.16943549134886));
#80235=CARTESIAN_POINT('Ctrl Pts',(17.1445189320766,-2.20380535104145,1.16445136754751));
#80236=CARTESIAN_POINT('Ctrl Pts',(17.0742287862168,-2.27008361804563,1.15946724374617));
#80237=CARTESIAN_POINT('Ctrl Pts',(17.0010210200543,-2.33287743512191,1.15448311994482));
#80238=CARTESIAN_POINT('Ctrl Pts',(16.9277346531377,-2.39573867184,1.14949364485481));
#80239=CARTESIAN_POINT('Ctrl Pts',(16.8515247457088,-2.45510770393165,1.14450416976479));
#80240=CARTESIAN_POINT('Ctrl Pts',(16.7727657065589,-2.51071782557272,1.13951469467478));
#80241=CARTESIAN_POINT('Ctrl Pts',(16.6939600044306,-2.56636089497363,1.13452226343179));
#80242=CARTESIAN_POINT('Ctrl Pts',(16.6126025329471,-2.61824038368877,1.12952983218879));
#80243=CARTESIAN_POINT('Ctrl Pts',(16.5290946600094,-2.66613423719263,1.1245374009458));
#80244=CARTESIAN_POINT('Ctrl Pts',(16.4454531613369,-2.71410472839716,1.11953698102737));
#80245=CARTESIAN_POINT('Ctrl Pts',(16.3596547806514,-2.75807665023309,1.11453656110893));
#80246=CARTESIAN_POINT('Ctrl Pts',(16.2721232444532,-2.79787503311384,1.1095361411905));
#80247=CARTESIAN_POINT('Ctrl Pts',(16.2235976642845,-2.81993839110969,1.10676401712906));
#80248=CARTESIAN_POINT('Ctrl Pts',(16.1745397518106,-2.84071994360021,1.10399189306762));
#80249=CARTESIAN_POINT('Ctrl Pts',(16.1250236863888,-2.86019648889098,1.10121976900619));
#80250=CARTESIAN_POINT('Ctrl Pts',(16.0356933907305,-2.89533347997462,1.09621867168757));
#80251=CARTESIAN_POINT('Ctrl Pts',(15.9445596851152,-2.9263427387285,1.09121757436896));
#80252=CARTESIAN_POINT('Ctrl Pts',(15.8520396290823,-2.95303754132475,1.08621647705035));
#80253=CARTESIAN_POINT('Ctrl Pts',(15.7596444867547,-2.97969630258196,1.08122213184176));
#80254=CARTESIAN_POINT('Ctrl Pts',(15.6658671319447,-3.0020520642932,1.07622778663316));
#80255=CARTESIAN_POINT('Ctrl Pts',(15.5711440478102,-3.01996634528449,1.07123344142456));
#80256=CARTESIAN_POINT('Ctrl Pts',(15.476520345553,-3.03786183091146,1.06624433619952));
#80257=CARTESIAN_POINT('Ctrl Pts',(15.3809533152628,-3.05132501860483,1.06125523097447));
#80258=CARTESIAN_POINT('Ctrl Pts',(15.2848930395133,-3.060267669018,1.05626612574943));
#80259=CARTESIAN_POINT('Ctrl Pts',(15.1889009372904,-3.06920397287417,1.05128056126893));
#80260=CARTESIAN_POINT('Ctrl Pts',(15.092416721016,-3.07362607677781,1.04629499678843));
#80261=CARTESIAN_POINT('Ctrl Pts',(14.9958981032323,-3.07349726280062,1.04130943230793));
#80262=CARTESIAN_POINT('Ctrl Pts',(14.8994142507982,-3.07336849522135,1.03632566359385));
#80263=CARTESIAN_POINT('Ctrl Pts',(14.8028964596618,-3.06869206737867,1.03134189487976));
#80264=CARTESIAN_POINT('Ctrl Pts',(14.7068040067704,-3.05948334846818,1.02635812616567));
#80265=CARTESIAN_POINT('Ctrl Pts',(14.610719982083,-3.0502754372482,1.02137479457457));
#80266=CARTESIAN_POINT('Ctrl Pts',(14.515061658071,-3.03653606739773,1.01639146298346));
#80267=CARTESIAN_POINT('Ctrl Pts',(14.4202836798045,-3.01833252609764,1.01140813139236));
#80268=CARTESIAN_POINT('Ctrl Pts',(14.3254881893817,-3.00012562132361,1.00642387902954));
#80269=CARTESIAN_POINT('Ctrl Pts',(14.2315737984917,-2.97745298969018,1.00143962666673));
#80270=CARTESIAN_POINT('Ctrl Pts',(14.138984390863,-2.95043291244225,0.996455374303908));
#80271=CARTESIAN_POINT('Ctrl Pts',(14.0462955485446,-2.92338381747979,0.991465769195024));
#80272=CARTESIAN_POINT('Ctrl Pts',(13.9549349519283,-2.89197807926445,0.98647616408614));
#80273=CARTESIAN_POINT('Ctrl Pts',(13.8653305375861,-2.85638363338424,0.981486558977256));
#80274=CARTESIAN_POINT('Ctrl Pts',(13.7756730178246,-2.82076809191418,0.976493996702998));
#80275=CARTESIAN_POINT('Ctrl Pts',(13.6877741521712,-2.78095908051636,0.971501434428742));
#80276=CARTESIAN_POINT('Ctrl Pts',(13.6020392023819,-2.73717150692516,0.966508872154485));
#80277=CARTESIAN_POINT('Ctrl Pts',(13.5161670619236,-2.69331386568329,0.961508320921701));
#80278=CARTESIAN_POINT('Ctrl Pts',(13.4324661316727,-2.64546516798433,0.956507769688916));
#80279=CARTESIAN_POINT('Ctrl Pts',(13.3513144472805,-2.59388476965609,0.951507218456132));
#80280=CARTESIAN_POINT('Ctrl Pts',(13.3063472068996,-2.56530337682445,0.948736345725575));
#80281=CARTESIAN_POINT('Ctrl Pts',(13.2621621416622,-2.53557694537095,0.945965472995017));
#80282=CARTESIAN_POINT('Ctrl Pts',(13.2188191240773,-2.50475486569991,0.94319460026446));
#80283=CARTESIAN_POINT('Ctrl Pts',(13.1411026375429,-2.44948913033611,0.938226268448822));
#80284=CARTESIAN_POINT('Ctrl Pts',(13.0658163178445,-2.39050011911477,0.933257936633185));
#80285=CARTESIAN_POINT('Ctrl Pts',(12.993341590778,-2.32803012839154,0.928289604817548));
#80286=CARTESIAN_POINT('Ctrl Pts',(12.9209650615504,-2.2656447798371,0.923328004720215));
#80287=CARTESIAN_POINT('Ctrl Pts',(12.851392890196,-2.19978811067773,0.918366404622881));
#80288=CARTESIAN_POINT('Ctrl Pts',(12.7849769697351,-2.13074522770695,0.913404804525548));
#80289=CARTESIAN_POINT('Ctrl Pts',(12.7170273221634,-2.06010795380276,0.908328627373058));
#80290=CARTESIAN_POINT('Ctrl Pts',(12.6523818995062,-1.98613574498245,0.903252450220569));
#80291=CARTESIAN_POINT('Ctrl Pts',(12.591381212228,-1.90917725347645,0.898176273068079));
#80292=CARTESIAN_POINT('Ctrl Pts',(12.5318614696195,-1.83408712235883,0.893223332846699));
#80293=CARTESIAN_POINT('Ctrl Pts',(12.4758117997149,-1.75615442742861,0.888270392625318));
#80294=CARTESIAN_POINT('Ctrl Pts',(12.423509743578,-1.67573870533634,0.883317452403938));
#80295=CARTESIAN_POINT('Ctrl Pts',(12.371224912302,-1.59534946689947,0.87836614335565));
#80296=CARTESIAN_POINT('Ctrl Pts',(12.3226854854737,-1.51247919856714,0.873414834307364));
#80297=CARTESIAN_POINT('Ctrl Pts',(12.2781261773748,-1.42751712553921,0.868463525259076));
#80298=CARTESIAN_POINT('Ctrl Pts',(12.233568985247,-1.34255908707331,0.863512451331738));
#80299=CARTESIAN_POINT('Ctrl Pts',(12.1929917421335,-1.25550983595175,0.858561377404399));
#80300=CARTESIAN_POINT('Ctrl Pts',(12.1565830637728,-1.16678291758856,0.853610303477062));
#80301=CARTESIAN_POINT('Ctrl Pts',(12.118568299928,-1.07414201437193,0.848440824259455));
#80302=CARTESIAN_POINT('Ctrl Pts',(12.0850985616984,-0.979672504177722,
0.843271345041847));
#80303=CARTESIAN_POINT('Ctrl Pts',(12.056331770515,-0.883866282149559,0.838101865824241));
#80304=CARTESIAN_POINT('Ctrl Pts',(12.0287437004715,-0.791985726300763,
0.833144206353827));
#80305=CARTESIAN_POINT('Ctrl Pts',(12.0054807933222,-0.698876309440068,
0.828186546883415));
#80306=CARTESIAN_POINT('Ctrl Pts',(11.9866303353989,-0.604983896035051,
0.823228887413001));
#80307=CARTESIAN_POINT('Ctrl Pts',(11.9677673215222,-0.511028942570008,
0.818267925734138));
#80308=CARTESIAN_POINT('Ctrl Pts',(11.9533226715503,-0.416290393835121,
0.813306964055275));
#80309=CARTESIAN_POINT('Ctrl Pts',(11.9433318910098,-0.321220051494601,
0.808346002376412));
#80310=CARTESIAN_POINT('Ctrl Pts',(11.9333265779387,-0.226011420394089,
0.803377824511912));
#80311=CARTESIAN_POINT('Ctrl Pts',(11.9277880803185,-0.130470475492244,
0.798409646647412));
#80312=CARTESIAN_POINT('Ctrl Pts',(11.92669985314,-0.035049355345871,0.793441468782912));
#80313=CARTESIAN_POINT('Ctrl Pts',(11.9265636897254,-0.023109876349453,
0.792819830143869));
#80314=CARTESIAN_POINT('Ctrl Pts',(11.9264971333298,-0.0111722661562855,
0.792198191504826));
#80315=CARTESIAN_POINT('Ctrl Pts',(11.9265000946077,0.00076259672746494,
0.791576552865783));
#80316=CARTESIAN_POINT('Origin',(15.,0.,8.20842344717745));
#80317=CARTESIAN_POINT('',(16.8723108164276,2.43738680900022,2.43734748439975));
#80318=CARTESIAN_POINT('',(16.8745674052796,2.44028174751842,2.35408151804441));
#80319=CARTESIAN_POINT('',(16.8723108164276,2.43738680900022,8.20842344717745));
#80320=CARTESIAN_POINT('',(11.9265010952115,-0.0025946606954943,1.70842344717746));
#80321=CARTESIAN_POINT('Ctrl Pts',(16.8745674052796,2.44028174751842,2.35408151804441));
#80322=CARTESIAN_POINT('Ctrl Pts',(17.5915515786301,1.8810510050653,2.30683846615771));
#80323=CARTESIAN_POINT('Ctrl Pts',(18.57195445782,-0.0162668050744201,2.20692035802376));
#80324=CARTESIAN_POINT('Ctrl Pts',(17.0556965627559,-2.98822639630323,2.05432719364256));
#80325=CARTESIAN_POINT('Ctrl Pts',(13.6199702038025,-3.35423301941131,1.89630202490083));
#80326=CARTESIAN_POINT('Ctrl Pts',(12.0268863100021,-1.40035468792022,1.78100077607913));
#80327=CARTESIAN_POINT('Ctrl Pts',(11.9234216648843,-0.194497604817307,
1.71837458350467));
#80328=CARTESIAN_POINT('Ctrl Pts',(11.9251450970424,-0.0025958054348495,
1.70842344717746));
#80329=CARTESIAN_POINT('Ctrl Pts',(11.9265010952115,-0.0025946606954943,
1.70842344717746));
#80330=CARTESIAN_POINT('Ctrl Pts',(11.9264210367132,0.0922384354117233,
1.70350363271174));
#80331=CARTESIAN_POINT('Ctrl Pts',(11.9307343098358,0.187216848308208,1.69858381824602));
#80332=CARTESIAN_POINT('Ctrl Pts',(11.9394546047295,0.281893833718155,1.69366400378031));
#80333=CARTESIAN_POINT('Ctrl Pts',(11.948166308935,0.376477549295093,1.6887490360075));
#80334=CARTESIAN_POINT('Ctrl Pts',(11.9612763661112,0.4707599788253,1.68383406823469));
#80335=CARTESIAN_POINT('Ctrl Pts',(11.9787464135551,0.564295150071033,1.67891910046188));
#80336=CARTESIAN_POINT('Ctrl Pts',(11.9962072615455,0.65778106716012,1.67400672083414));
#80337=CARTESIAN_POINT('Ctrl Pts',(12.0180234592683,0.750520063001247,1.6690943412064));
#80338=CARTESIAN_POINT('Ctrl Pts',(12.0441050153961,0.842073090647898,1.66418196157866));
#80339=CARTESIAN_POINT('Ctrl Pts',(12.0701804419867,0.933604602029459,1.65927073643008));
#80340=CARTESIAN_POINT('Ctrl Pts',(12.1005191119511,1.0239502635342,1.65435951128151));
#80341=CARTESIAN_POINT('Ctrl Pts',(12.1349806190297,1.11268423043766,1.64944828613293));
#80342=CARTESIAN_POINT('Ctrl Pts',(12.1694440749485,1.20142321535485,1.64453678324859));
#80343=CARTESIAN_POINT('Ctrl Pts',(12.2080306654003,1.28854990321406,1.63962528036426));
#80344=CARTESIAN_POINT('Ctrl Pts',(12.250551564298,1.37365772644274,1.63471377747993));
#80345=CARTESIAN_POINT('Ctrl Pts',(12.293113726129,1.4588481396102,1.62979750839777));
#80346=CARTESIAN_POINT('Ctrl Pts',(12.3396176159273,1.54201537104518,1.6248812393156));
#80347=CARTESIAN_POINT('Ctrl Pts',(12.3898282804378,1.62277720109616,1.61996497023344));
#80348=CARTESIAN_POINT('Ctrl Pts',(12.4400646730544,1.70358041376894,1.61504618203917));
#80349=CARTESIAN_POINT('Ctrl Pts',(12.4940113630609,1.78197539972019,1.61012739384489));
#80350=CARTESIAN_POINT('Ctrl Pts',(12.5513911754764,1.8576105820288,1.60520860565062));
#80351=CARTESIAN_POINT('Ctrl Pts',(12.6088638310716,1.93336814554642,1.60028185863047));
#80352=CARTESIAN_POINT('Ctrl Pts',(12.6697804092842,2.0063566429471,1.59535511161032));
#80353=CARTESIAN_POINT('Ctrl Pts',(12.7338248711224,2.07625926494174,1.59042836459017));
#80354=CARTESIAN_POINT('Ctrl Pts',(12.7779215682039,2.12438949601602,1.5870361388659));
#80355=CARTESIAN_POINT('Ctrl Pts',(12.8235003370015,2.17105754874544,1.58364391314163));
#80356=CARTESIAN_POINT('Ctrl Pts',(12.870448969525,2.21617117087174,1.58025168741736));
#80357=CARTESIAN_POINT('Ctrl Pts',(12.939662886243,2.28267982760693,1.57525070621411));
#80358=CARTESIAN_POINT('Ctrl Pts',(13.0121162445308,2.34605892694005,1.57024972501086));
#80359=CARTESIAN_POINT('Ctrl Pts',(13.0874945653347,2.40597697669279,1.56524874380762));
#80360=CARTESIAN_POINT('Ctrl Pts',(13.1627710746291,2.46581409671629,1.56025451729776));
#80361=CARTESIAN_POINT('Ctrl Pts',(13.2409643540982,2.52219918746141,1.55526029078791));
#80362=CARTESIAN_POINT('Ctrl Pts',(13.3217235890849,2.57483796355539,1.55026606427806));
#80363=CARTESIAN_POINT('Ctrl Pts',(13.4023980522268,2.62742148545873,1.54527708013826));
#80364=CARTESIAN_POINT('Ctrl Pts',(13.4856327508062,2.67626627209292,1.54028809599846));
#80365=CARTESIAN_POINT('Ctrl Pts',(13.5710451584194,2.72111931210729,1.53529911185867));
#80366=CARTESIAN_POINT('Ctrl Pts',(13.6563968961586,2.76594049225077,1.53031367147846));
#80367=CARTESIAN_POINT('Ctrl Pts',(13.7439228805237,2.80677535915943,1.52532823109825));
#80368=CARTESIAN_POINT('Ctrl Pts',(13.8332139058721,2.84341563274694,1.52034279071804));
#80369=CARTESIAN_POINT('Ctrl Pts',(13.922472735926,2.88004269510308,1.51535914791738));
#80370=CARTESIAN_POINT('Ctrl Pts',(14.0134949370345,2.91247800289763,1.51037550511672));
#80371=CARTESIAN_POINT('Ctrl Pts',(14.1058500172198,2.9405608407741,1.50539186231606));
#80372=CARTESIAN_POINT('Ctrl Pts',(14.1981969663038,2.96864120618887,1.50040865828394));
#80373=CARTESIAN_POINT('Ctrl Pts',(14.2918761414045,2.9923697361742,1.49542545425183));
#80374=CARTESIAN_POINT('Ctrl Pts',(14.386441558151,3.01163548399135,1.49044225021972));
#80375=CARTESIAN_POINT('Ctrl Pts',(14.4810244201531,3.03090478591852,1.48545812689521));
#80376=CARTESIAN_POINT('Ctrl Pts',(14.5764934186825,3.04570958307655,1.4804740035707));
#80377=CARTESIAN_POINT('Ctrl Pts',(14.6723930966562,3.05599017781168,1.4754898802462));
#80378=CARTESIAN_POINT('Ctrl Pts',(14.7683957392884,3.06628181051847,1.47050040561533));
#80379=CARTESIAN_POINT('Ctrl Pts',(14.864829547641,3.07203949665644,1.46551093098446));
#80380=CARTESIAN_POINT('Ctrl Pts',(14.9612348975193,3.07325552416809,1.46052145635359));
#80381=CARTESIAN_POINT('Ctrl Pts',(15.0576973656084,3.07447227215133,1.4555290255604));
#80382=CARTESIAN_POINT('Ctrl Pts',(15.1541309034876,3.07114201867648,1.4505365947672));
#80383=CARTESIAN_POINT('Ctrl Pts',(15.2500789622654,3.06330911966655,1.44554416397401));
#80384=CARTESIAN_POINT('Ctrl Pts',(15.3461805534101,3.05546368675505,1.44054374448645));
#80385=CARTESIAN_POINT('Ctrl Pts',(15.4417946796475,3.04310127835409,1.4355433249989));
#80386=CARTESIAN_POINT('Ctrl Pts',(15.5364730371926,3.02631771801399,1.43054290551135));
#80387=CARTESIAN_POINT('Ctrl Pts',(15.5889607566914,3.01701325995024,1.4277707765661));
#80388=CARTESIAN_POINT('Ctrl Pts',(15.6411611034272,3.00635092360513,1.42499864762086));
#80389=CARTESIAN_POINT('Ctrl Pts',(15.6929998032508,2.99435360682307,1.42222651867561));
#80390=CARTESIAN_POINT('Ctrl Pts',(15.7865289946372,2.97270762917992,1.41722494688563));
#80391=CARTESIAN_POINT('Ctrl Pts',(15.8792061005138,2.94663761271737,1.41222337509564));
#80392=CARTESIAN_POINT('Ctrl Pts',(15.9705815251702,2.91622594340671,1.40722180330566));
#80393=CARTESIAN_POINT('Ctrl Pts',(16.0618102063975,2.88586311340545,1.40222826373875));
#80394=CARTESIAN_POINT('Ctrl Pts',(16.1517409521813,2.85117263825007,1.39723472417185));
#80395=CARTESIAN_POINT('Ctrl Pts',(16.23993582613,2.81228757368079,1.39224118460495));
#80396=CARTESIAN_POINT('Ctrl Pts',(16.3280487064443,2.77343866005341,1.38725228746723));
#80397=CARTESIAN_POINT('Ctrl Pts',(16.4144285216831,2.73040307941623,1.38226339032952));
#80398=CARTESIAN_POINT('Ctrl Pts',(16.4986544260729,2.68336303194557,1.3772744931918));
#80399=CARTESIAN_POINT('Ctrl Pts',(16.5828202222499,2.63635655482602,1.37228915640399));
#80400=CARTESIAN_POINT('Ctrl Pts',(16.6648347817327,2.5853515055851,1.36730381961618));
#80401=CARTESIAN_POINT('Ctrl Pts',(16.7443001550306,2.53057685501947,1.36231848282837));
#80402=CARTESIAN_POINT('Ctrl Pts',(16.7877527159398,2.50062545932088,1.35959244453729));
#80403=CARTESIAN_POINT('Ctrl Pts',(16.8304434838481,2.46954775257882,1.35686640624621));
#80404=CARTESIAN_POINT('Ctrl Pts',(16.8723108164276,2.43738680900022,1.35414036795513));
#80405=CARTESIAN_POINT('',(11.9265006184838,0.00194982547800578,1.79157655278712));
#80406=CARTESIAN_POINT('Ctrl Pts',(11.9265006184838,0.00194982547801677,
1.79157655278712));
#80407=CARTESIAN_POINT('Ctrl Pts',(11.9265698355604,0.111056329985969,1.78594824763792));
#80408=CARTESIAN_POINT('Ctrl Pts',(11.9324528884889,0.219943981301199,1.78031994248873));
#80409=CARTESIAN_POINT('Ctrl Pts',(11.944055790133,0.328035419093971,1.77469163733954));
#80410=CARTESIAN_POINT('Ctrl Pts',(11.9557100333901,0.436605150071001,1.76903842753511));
#80411=CARTESIAN_POINT('Ctrl Pts',(11.9731347345555,0.544371404507665,1.76338521773069));
#80412=CARTESIAN_POINT('Ctrl Pts',(11.996184973256,0.650766882306438,1.75773200792626));
#80413=CARTESIAN_POINT('Ctrl Pts',(12.0193615261158,0.757745402020997,1.75204781881385));
#80414=CARTESIAN_POINT('Ctrl Pts',(12.0482253298664,0.863337884085554,1.74636362970144));
#80415=CARTESIAN_POINT('Ctrl Pts',(12.0825807013878,0.966988565643491,1.74067944058904));
#80416=CARTESIAN_POINT('Ctrl Pts',(12.0974066837613,1.01171878131936,1.73822644171707));
#80417=CARTESIAN_POINT('Ctrl Pts',(12.113254780959,1.05608764941845,1.7357734428451));
#80418=CARTESIAN_POINT('Ctrl Pts',(12.1301065854665,1.1000518347865,1.73332044397313));
#80419=CARTESIAN_POINT('Ctrl Pts',(12.164462065989,1.18968085424443,1.72831955787038));
#80420=CARTESIAN_POINT('Ctrl Pts',(12.2030802784572,1.2778552664331,1.72331867176762));
#80421=CARTESIAN_POINT('Ctrl Pts',(12.2458175953055,1.36414131660581,1.71831778566487));
#80422=CARTESIAN_POINT('Ctrl Pts',(12.2884971917689,1.4503108301219,1.71332365368454));
#80423=CARTESIAN_POINT('Ctrl Pts',(12.3352846428408,1.53459666069137,1.70832952170421));
#80424=CARTESIAN_POINT('Ctrl Pts',(12.3859876110696,1.61658327361088,1.70333538972388));
#80425=CARTESIAN_POINT('Ctrl Pts',(12.4366373630816,1.69848383599879,1.69834649942505));
#80426=CARTESIAN_POINT('Ctrl Pts',(12.491194232924,1.77808960697265,1.69335760912621));
#80427=CARTESIAN_POINT('Ctrl Pts',(12.5494196283456,1.85500891967181,1.68836871882738));
#80428=CARTESIAN_POINT('Ctrl Pts',(12.6076036808387,1.93187361583092,1.68338337088894));
#80429=CARTESIAN_POINT('Ctrl Pts',(12.6694508165293,2.00605529705837,1.6783980229505));
#80430=CARTESIAN_POINT('Ctrl Pts',(12.7346792726769,2.07719143372977,1.67341267501206));
#80431=CARTESIAN_POINT('Ctrl Pts',(12.7998842210012,2.14830193349622,1.66842912375387));
#80432=CARTESIAN_POINT('Ctrl Pts',(12.8684677723131,2.21636874656426,1.66344557249567));
#80433=CARTESIAN_POINT('Ctrl Pts',(12.9401086694023,2.28106333891201,1.65846202123747));
#80434=CARTESIAN_POINT('Ctrl Pts',(13.011743273447,2.34575224838913,1.65347890774194));
#80435=CARTESIAN_POINT('Ctrl Pts',(13.0864343635891,2.40706923226672,1.64849579424641));
#80436=CARTESIAN_POINT('Ctrl Pts',(13.1638254948465,2.46472421106789,1.64351268075087));
#80437=CARTESIAN_POINT('Ctrl Pts',(13.2412309206289,2.52238983902899,1.63852864684961));
#80438=CARTESIAN_POINT('Ctrl Pts',(13.3213370261886,2.57639185654604,1.63354461294836));
#80439=CARTESIAN_POINT('Ctrl Pts',(13.4037569974814,2.62648253885505,1.6285605790471));
#80440=CARTESIAN_POINT('Ctrl Pts',(13.4862654990349,2.67662702537064,1.62357119161545));
#80441=CARTESIAN_POINT('Ctrl Pts',(13.5710924526084,2.72285156117808,1.61858180418381));
#80442=CARTESIAN_POINT('Ctrl Pts',(13.6578251637094,2.76495369921961,1.61359241675217));
#80443=CARTESIAN_POINT('Ctrl Pts',(13.744609282735,2.80708079190066,1.60860007202737));
#80444=CARTESIAN_POINT('Ctrl Pts',(13.8333010054676,2.84508044886725,1.60360772730257));
#80445=CARTESIAN_POINT('Ctrl Pts',(13.9234682772436,2.87879865567203,1.59861538257777));
#80446=CARTESIAN_POINT('Ctrl Pts',(14.0137798807211,2.91257083556553,1.59361504655419));
#80447=CARTESIAN_POINT('Ctrl Pts',(14.1055713319809,2.94204774716723,1.58861471053061));
#80448=CARTESIAN_POINT('Ctrl Pts',(14.1983961503845,2.96712546385918,1.58361437450704));
#80449=CARTESIAN_POINT('Ctrl Pts',(14.2498739494698,2.98103279687194,1.58084134141516));
#80450=CARTESIAN_POINT('Ctrl Pts',(14.3016693755805,2.99358808204046,1.57806830832328));
#80451=CARTESIAN_POINT('Ctrl Pts',(14.3537053912393,3.00478044600382,1.5752952752314));
#80452=CARTESIAN_POINT('Ctrl Pts',(14.4475558636107,3.02496663112224,1.57029392256673));
#80453=CARTESIAN_POINT('Ctrl Pts',(14.5425166949139,3.04078686829603,1.56529256990206));
#80454=CARTESIAN_POINT('Ctrl Pts',(14.6381459848649,3.05212449315729,1.56029121723738));
#80455=CARTESIAN_POINT('Ctrl Pts',(14.7360484047801,3.06373161593919,1.55517098128278));
#80456=CARTESIAN_POINT('Ctrl Pts',(14.834651037717,3.07064013422976,1.55005074532817));
#80457=CARTESIAN_POINT('Ctrl Pts',(14.9334654360006,3.07277975159194,1.54493050937356));
#80458=CARTESIAN_POINT('Ctrl Pts',(15.0297349728532,3.07486426534779,1.53994213973828));
#80459=CARTESIAN_POINT('Ctrl Pts',(15.1262050293233,3.07242250789681,1.534953770103));
#80460=CARTESIAN_POINT('Ctrl Pts',(15.2224172674361,3.06544169886597,1.52996540046772));
#80461=CARTESIAN_POINT('Ctrl Pts',(15.3185662289433,3.0584654809548,1.52498031156994));
#80462=CARTESIAN_POINT('Ctrl Pts',(15.4144572728825,3.04695617520024,1.51999522267215));
#80463=CARTESIAN_POINT('Ctrl Pts',(15.5096329791833,3.03095306405902,1.51501013377437));
#80464=CARTESIAN_POINT('Ctrl Pts',(15.6047720307396,3.01495611614971,1.51002696476946));
#80465=CARTESIAN_POINT('Ctrl Pts',(15.6991958603445,2.99446887633508,1.50504379576455));
#80466=CARTESIAN_POINT('Ctrl Pts',(15.7924541456017,2.96958223949409,1.50006062675964));
#80467=CARTESIAN_POINT('Ctrl Pts',(15.8901681473408,2.94350656301284,1.49483937072356));
#80468=CARTESIAN_POINT('Ctrl Pts',(15.9866019507966,2.91260073338112,1.48961811468749));
#80469=CARTESIAN_POINT('Ctrl Pts',(16.0812530067942,2.87702870776404,1.48439685865142));
#80470=CARTESIAN_POINT('Ctrl Pts',(16.1716282965709,2.84306361261318,1.47941146760338));
#80471=CARTESIAN_POINT('Ctrl Pts',(16.2603779902462,2.80484495110589,1.47442607655533));
#80472=CARTESIAN_POINT('Ctrl Pts',(16.3470845853442,2.76256499831732,1.46944068550729));
#80473=CARTESIAN_POINT('Ctrl Pts',(16.4338218336145,2.7202700983996,1.46445353198604));
#80474=CARTESIAN_POINT('Ctrl Pts',(16.5185141581414,2.67391125463293,1.45946637846479));
#80475=CARTESIAN_POINT('Ctrl Pts',(16.60076913139,2.62372644114989,1.45447922494355));
#80476=CARTESIAN_POINT('Ctrl Pts',(16.6831075506654,2.57349071617627,1.4494870120547));
#80477=CARTESIAN_POINT('Ctrl Pts',(16.7630033204026,2.51942151976691,1.44449479916585));
#80478=CARTESIAN_POINT('Ctrl Pts',(16.8400938804713,2.46179949651716,1.439502586277));
#80479=CARTESIAN_POINT('Ctrl Pts',(16.8508881161555,2.45373124926347,1.43880357562692));
#80480=CARTESIAN_POINT('Ctrl Pts',(16.8616274084294,2.44559340972417,1.43810456497685));
#80481=CARTESIAN_POINT('Ctrl Pts',(16.8723108164276,2.43738680900023,1.43740555432678));
#80482=CARTESIAN_POINT('Ctrl Pts',(16.8723108164276,2.43738680900022,2.43734748439974));
#80483=CARTESIAN_POINT('Ctrl Pts',(16.9488595251288,2.37858490904914,2.43236381332471));
#80484=CARTESIAN_POINT('Ctrl Pts',(17.0226234707783,2.31618266128806,2.42738014224968));
#80485=CARTESIAN_POINT('Ctrl Pts',(17.0932575334937,2.25048331441755,2.42239647117465));
#80486=CARTESIAN_POINT('Ctrl Pts',(17.1639647946043,2.18471588301997,2.41740763549899));
#80487=CARTESIAN_POINT('Ctrl Pts',(17.2315353734165,2.11564482830248,2.41241879982333));
#80488=CARTESIAN_POINT('Ctrl Pts',(17.2956604304822,2.04361088221767,2.40742996414767));
#80489=CARTESIAN_POINT('Ctrl Pts',(17.359819608922,1.97153860638563,2.40243847387899));
#80490=CARTESIAN_POINT('Ctrl Pts',(17.4205293379208,1.89650064017566,2.39744698361031));
#80491=CARTESIAN_POINT('Ctrl Pts',(17.4775219314432,1.81886979446515,2.39245549334163));
#80492=CARTESIAN_POINT('Ctrl Pts',(17.534609958825,1.7411089562284,2.38745564484339));
#80493=CARTESIAN_POINT('Ctrl Pts',(17.5879681735439,1.66074693078762,2.38245579634514));
#80494=CARTESIAN_POINT('Ctrl Pts',(17.6373729259274,1.57818449478665,2.3774559478469));
#80495=CARTESIAN_POINT('Ctrl Pts',(17.6770126431661,1.51194083482035,2.37344433821129));
#80496=CARTESIAN_POINT('Ctrl Pts',(17.7141081258761,1.4442812245987,2.36943272857568));
#80497=CARTESIAN_POINT('Ctrl Pts',(17.748566182052,1.37542218714116,2.36542111894007));
#80498=CARTESIAN_POINT('Ctrl Pts',(17.7915216125909,1.28958247565582,2.36042024430652));
#80499=CARTESIAN_POINT('Ctrl Pts',(17.8305268726252,1.20157879439895,2.35541936967296));
#80500=CARTESIAN_POINT('Ctrl Pts',(17.8653588069058,1.11180985680425,2.35041849503941));
#80501=CARTESIAN_POINT('Ctrl Pts',(17.9001436983387,1.02216215814038,2.34542437442022));
#80502=CARTESIAN_POINT('Ctrl Pts',(17.9307663087813,0.930754346975528,2.34043025380103));
#80503=CARTESIAN_POINT('Ctrl Pts',(17.9570498009236,0.838008785668726,2.33543613318183));
#80504=CARTESIAN_POINT('Ctrl Pts',(17.9833057073287,0.745360565105695,2.33044725412255));
#80505=CARTESIAN_POINT('Ctrl Pts',(18.005231429926,0.651377805421232,2.32545837506326));
#80506=CARTESIAN_POINT('Ctrl Pts',(18.0226989602409,0.556500894661161,2.32046949600397));
#80507=CARTESIAN_POINT('Ctrl Pts',(18.0401540885004,0.461691347098805,2.31548415907989));
#80508=CARTESIAN_POINT('Ctrl Pts',(18.0531572379258,0.365989340739401,2.31049882215582));
#80509=CARTESIAN_POINT('Ctrl Pts',(18.0616310358816,0.269847457142608,2.30551348523175));
#80510=CARTESIAN_POINT('Ctrl Pts',(18.070101780184,0.173740219640054,2.30052994484469));
#80511=CARTESIAN_POINT('Ctrl Pts',(18.0740463776682,0.0771938564023398,
2.29554640445763));
#80512=CARTESIAN_POINT('Ctrl Pts',(18.0734391959091,-0.0193328489793903,
2.29056286407058));
#80513=CARTESIAN_POINT('Ctrl Pts',(18.0728320674669,-0.11585107830551,2.28557976129056));
#80514=CARTESIAN_POINT('Ctrl Pts',(18.0676739574472,-0.212349214546744,
2.28059665851053));
#80515=CARTESIAN_POINT('Ctrl Pts',(18.0579913576166,-0.308368459383391,
2.27561355573051));
#80516=CARTESIAN_POINT('Ctrl Pts',(18.0483069690312,-0.404405442728394,
2.2706295323766));
#80517=CARTESIAN_POINT('Ctrl Pts',(18.0340964746571,-0.499962922521446,
2.26564550902268));
#80518=CARTESIAN_POINT('Ctrl Pts',(18.0154381165457,-0.594588273751947,
2.26066148566876));
#80519=CARTESIAN_POINT('Ctrl Pts',(17.9967597155873,-0.689315271731034,
2.25567210846662));
#80520=CARTESIAN_POINT('Ctrl Pts',(17.9736239974891,-0.783107711128687,
2.25068273126448));
#80521=CARTESIAN_POINT('Ctrl Pts',(17.9461600823604,-0.875524425191021,
2.24569335406234));
#80522=CARTESIAN_POINT('Ctrl Pts',(17.9186798879704,-0.967995919346955,
2.2407010194022));
#80523=CARTESIAN_POINT('Ctrl Pts',(17.8868665326475,-1.05908965050869,2.23570868474206));
#80524=CARTESIAN_POINT('Ctrl Pts',(17.8508979423385,-1.14838285095618,2.23071635008192));
#80525=CARTESIAN_POINT('Ctrl Pts',(17.8148717740528,-1.23781899061168,2.22571602376778));
#80526=CARTESIAN_POINT('Ctrl Pts',(17.774677272193,-1.32544844613389,2.22071569745364));
#80527=CARTESIAN_POINT('Ctrl Pts',(17.7305390600662,-1.41087160700504,2.2157153711395));
#80528=CARTESIAN_POINT('Ctrl Pts',(17.7060603665301,-1.45824659740661,2.21294223082578));
#80529=CARTESIAN_POINT('Ctrl Pts',(17.6803694935711,-1.50494347420096,2.21016909051206));
#80530=CARTESIAN_POINT('Ctrl Pts',(17.653510412745,-1.55089804289437,2.20739595019834));
#80531=CARTESIAN_POINT('Ctrl Pts',(17.6050747227622,-1.63376913058891,2.2023950730133));
#80532=CARTESIAN_POINT('Ctrl Pts',(17.5526686296632,-1.71451359020438,2.19739419582825));
#80533=CARTESIAN_POINT('Ctrl Pts',(17.4965042006414,-1.79272670147452,2.19239331864321));
#80534=CARTESIAN_POINT('Ctrl Pts',(17.4404156255765,-1.87083418051327,2.18739919548965));
#80535=CARTESIAN_POINT('Ctrl Pts',(17.3805790565024,-1.94641675259952,2.18240507233609));
#80536=CARTESIAN_POINT('Ctrl Pts',(17.3172516710118,-2.01909557554691,2.17741094918253));
#80537=CARTESIAN_POINT('Ctrl Pts',(17.2539907507559,-2.09169811846171,2.17242206760914));
#80538=CARTESIAN_POINT('Ctrl Pts',(17.1872465842831,-2.16140264186641,2.16743318603574));
#80539=CARTESIAN_POINT('Ctrl Pts',(17.1173181210884,-2.22786135657286,2.16244430446235));
#80540=CARTESIAN_POINT('Ctrl Pts',(17.0474393080759,-2.29427288466681,2.15745896506431));
#80541=CARTESIAN_POINT('Ctrl Pts',(16.9743810100404,-2.35744288416394,2.15247362566628));
#80542=CARTESIAN_POINT('Ctrl Pts',(16.8984800503645,-2.41705931833873,2.14748828626824));
#80543=CARTESIAN_POINT('Ctrl Pts',(16.8226064430564,-2.47665426858703,2.14250474343296));
#80544=CARTESIAN_POINT('Ctrl Pts',(16.7438925541852,-2.53269792729628,2.13752120059768));
#80545=CARTESIAN_POINT('Ctrl Pts',(16.6627086657526,-2.58491820815115,2.1325376577624));
#80546=CARTESIAN_POINT('Ctrl Pts',(16.5815319065773,-2.63713390322139,2.12755455256272));
#80547=CARTESIAN_POINT('Ctrl Pts',(16.497885948157,-2.68552665086909,2.12257144736304));
#80548=CARTESIAN_POINT('Ctrl Pts',(16.4121695582981,-2.72986801670265,2.11758834216336));
#80549=CARTESIAN_POINT('Ctrl Pts',(16.3264373338193,-2.77421757383632,2.11260431642122));
#80550=CARTESIAN_POINT('Ctrl Pts',(16.2386343079239,-2.81451406124734,2.10762029067908));
#80551=CARTESIAN_POINT('Ctrl Pts',(16.1491823467888,-2.85057576356584,2.10263626493694));
#80552=CARTESIAN_POINT('Ctrl Pts',(16.0596342973297,-2.88667620297287,2.09764688540854));
#80553=CARTESIAN_POINT('Ctrl Pts',(15.9684341840563,-2.9185326116556,2.09265750588014));
#80554=CARTESIAN_POINT('Ctrl Pts',(15.8760220683032,-2.94601214964327,2.08766812635174));
#80555=CARTESIAN_POINT('Ctrl Pts',(15.7835551757941,-2.9735079759708,2.08267578939699));
#80556=CARTESIAN_POINT('Ctrl Pts',(15.6898752760018,-2.99662166072452,2.07768345244225));
#80557=CARTESIAN_POINT('Ctrl Pts',(15.5954336797639,-3.01527129509151,2.07269111548751));
#80558=CARTESIAN_POINT('Ctrl Pts',(15.500840904271,-3.03395078322995,2.06769078695054));
#80559=CARTESIAN_POINT('Ctrl Pts',(15.4054844312867,-3.04815188815817,2.06269045841358));
#80560=CARTESIAN_POINT('Ctrl Pts',(15.3098216838575,-3.0578444653402,2.05769012987661));
#80561=CARTESIAN_POINT('Ctrl Pts',(15.2567683880726,-3.06321984058265,2.05491701373661));
#80562=CARTESIAN_POINT('Ctrl Pts',(15.2036209243158,-3.0672094732637,2.0521438975966));
#80563=CARTESIAN_POINT('Ctrl Pts',(15.1504570807384,-3.06981512747196,2.0493707814566));
#80564=CARTESIAN_POINT('Ctrl Pts',(15.0545843771295,-3.07451401861313,2.04436989882898));
#80565=CARTESIAN_POINT('Ctrl Pts',(14.9583240901873,-3.07472553622669,2.03936901620135));
#80566=CARTESIAN_POINT('Ctrl Pts',(14.8621310646495,-3.07040622828077,2.03436813357373));
#80567=CARTESIAN_POINT('Ctrl Pts',(14.7660679534245,-3.0660927538131,2.02937400493088));
#80568=CARTESIAN_POINT('Ctrl Pts',(14.6700723575853,-3.05726063493976,2.02437987628803));
#80569=CARTESIAN_POINT('Ctrl Pts',(14.5746020880084,-3.04391834096665,2.01938574764518));
#80570=CARTESIAN_POINT('Ctrl Pts',(14.4792320183685,-3.03059005027459,2.01439686054379));
#80571=CARTESIAN_POINT('Ctrl Pts',(14.3843866110825,-3.01276105520946,2.0094079734424));
#80572=CARTESIAN_POINT('Ctrl Pts',(14.2905204849002,-2.99049177689118,2.00441908634101));
#80573=CARTESIAN_POINT('Ctrl Pts',(14.1967210042557,-2.96823830990006,1.99943374138073));
#80574=CARTESIAN_POINT('Ctrl Pts',(14.1038998480948,-2.94155092800557,1.99444839642044));
#80575=CARTESIAN_POINT('Ctrl Pts',(14.0125023773816,-2.91054130623893,1.98946305146016));
#80576=CARTESIAN_POINT('Ctrl Pts',(13.9211378431163,-2.87954285925408,1.98447950304362));
#80577=CARTESIAN_POINT('Ctrl Pts',(13.8311963898972,-2.84422540803508,1.97949595462709));
#80578=CARTESIAN_POINT('Ctrl Pts',(13.7431081927623,-2.80475047640585,1.97451240621055));
#80579=CARTESIAN_POINT('Ctrl Pts',(13.6550277309741,-2.7652790112147,1.96952929541762));
#80580=CARTESIAN_POINT('Ctrl Pts',(13.5688006019236,-2.72165097107885,1.96454618462469));
#80581=CARTESIAN_POINT('Ctrl Pts',(13.4848359778387,-2.67407558530942,1.95956307383176));
#80582=CARTESIAN_POINT('Ctrl Pts',(13.4008558426759,-2.62649141077304,1.9545790424914));
#80583=CARTESIAN_POINT('Ctrl Pts',(13.3191394241955,-2.57495865865483,1.94959501115103));
#80584=CARTESIAN_POINT('Ctrl Pts',(13.2400693798354,-2.51973142660226,1.94461097981066));
#80585=CARTESIAN_POINT('Ctrl Pts',(13.1609143998115,-2.4644448704194,1.93962159471068));
#80586=CARTESIAN_POINT('Ctrl Pts',(13.0844118291418,-2.4054561632609,1.9346322096107));
#80587=CARTESIAN_POINT('Ctrl Pts',(13.0109133258318,-2.34306134205798,1.92964282451072));
#80588=CARTESIAN_POINT('Ctrl Pts',(12.9373712568537,-2.28062953680839,1.92465048199139));
#80589=CARTESIAN_POINT('Ctrl Pts',(12.8668371213099,-2.21478789660277,1.91965813947206));
#80590=CARTESIAN_POINT('Ctrl Pts',(12.7996260617113,-2.14586970287109,1.91466579695273));
#80591=CARTESIAN_POINT('Ctrl Pts',(12.7323074136824,-2.07684118800574,1.90966546291685));
#80592=CARTESIAN_POINT('Ctrl Pts',(12.6683227538112,-2.00472661410948,1.90466512888096));
#80593=CARTESIAN_POINT('Ctrl Pts',(12.6079472049745,-1.92989265914212,1.89966479484507));
#80594=CARTESIAN_POINT('Ctrl Pts',(12.5744644293987,-1.88839161165023,1.89689173413501));
#80595=CARTESIAN_POINT('Ctrl Pts',(12.5420908874423,-1.84605474329759,1.89411867342494));
#80596=CARTESIAN_POINT('Ctrl Pts',(12.5108675917382,-1.80294817012053,1.89134561271488));
#80597=CARTESIAN_POINT('Ctrl Pts',(12.4541870026739,-1.72469550956294,1.88631159208979));
#80598=CARTESIAN_POINT('Ctrl Pts',(12.4011017867308,-1.64363183337957,1.8812775714647));
#80599=CARTESIAN_POINT('Ctrl Pts',(12.3519001953372,-1.56011848093183,1.87624355083961));
#80600=CARTESIAN_POINT('Ctrl Pts',(12.3027665260435,-1.47672041748381,1.87121647960866));
#80601=CARTESIAN_POINT('Ctrl Pts',(12.2575060428062,-1.39087976641773,1.86618940837772));
#80602=CARTESIAN_POINT('Ctrl Pts',(12.2163652628411,-1.30298883344488,1.86116233714677));
#80603=CARTESIAN_POINT('Ctrl Pts',(12.1752705752684,-1.21519636976166,1.85614089803414));
#80604=CARTESIAN_POINT('Ctrl Pts',(12.1382865969624,-1.12535857852669,1.8511194589215));
#80605=CARTESIAN_POINT('Ctrl Pts',(12.1056147224448,-1.03389366719782,1.84609801980887));
#80606=CARTESIAN_POINT('Ctrl Pts',(12.0729730496365,-0.942513305552657,
1.84108122248818));
#80607=CARTESIAN_POINT('Ctrl Pts',(12.0446356948167,-0.849509220498868,
1.83606442516749));
#80608=CARTESIAN_POINT('Ctrl Pts',(12.0207561451115,-0.755320000469499,
1.8310476278468));
#80609=CARTESIAN_POINT('Ctrl Pts',(11.9968896807392,-0.661182393528222,
1.82603357959232));
#80610=CARTESIAN_POINT('Ctrl Pts',(11.9774762692274,-0.565861359986251,
1.82101953133784));
#80611=CARTESIAN_POINT('Ctrl Pts',(11.96261946134,-0.469810295086867,1.81600548308336));
#80612=CARTESIAN_POINT('Ctrl Pts',(11.9477647807859,-0.373772983654849,
1.81099215278603));
#80613=CARTESIAN_POINT('Ctrl Pts',(11.9374654783482,-0.277006273422207,
1.80597882248871));
#80614=CARTESIAN_POINT('Ctrl Pts',(11.9317737860968,-0.179972637690354,
1.80096549219138));
#80615=CARTESIAN_POINT('Ctrl Pts',(11.9282206620398,-0.11939793859866,1.7978358457351));
#80616=CARTESIAN_POINT('Ctrl Pts',(11.9264621300047,-0.0587193777735862,
1.79470619927883));
#80617=CARTESIAN_POINT('Ctrl Pts',(11.9265006184833,0.00194982479121544,
1.79157655282255));
#80618=CARTESIAN_POINT('Origin',(15.,0.,8.20842344717745));
#80619=CARTESIAN_POINT('',(16.8723108164276,2.43738680900022,3.43723392788203));
#80620=CARTESIAN_POINT('',(16.8723108164276,2.43738680900022,3.35426497682436));
#80621=CARTESIAN_POINT('',(16.8723108164276,2.43738680900022,8.20842344717745));
#80622=CARTESIAN_POINT('',(11.9265007775872,0.00218628177021425,2.70842344717746));
#80623=CARTESIAN_POINT('Ctrl Pts',(16.8723108164276,2.43738680900022,3.35426497682436));
#80624=CARTESIAN_POINT('Ctrl Pts',(16.9487990501378,2.37863136371089,3.34927201212424));
#80625=CARTESIAN_POINT('Ctrl Pts',(17.0224461613876,2.31632796124631,3.34427904742411));
#80626=CARTESIAN_POINT('Ctrl Pts',(17.0929223199439,2.25079506234593,3.33928608272398));
#80627=CARTESIAN_POINT('Ctrl Pts',(17.1635078534999,2.1851604601043,3.3342853692259));
#80628=CARTESIAN_POINT('Ctrl Pts',(17.2309123057041,2.11628667045165,3.32928465572782));
#80629=CARTESIAN_POINT('Ctrl Pts',(17.2948444052853,2.04452718385714,3.32428394222975));
#80630=CARTESIAN_POINT('Ctrl Pts',(17.3193712199737,2.01699748216784,3.32236547601198));
#80631=CARTESIAN_POINT('Ctrl Pts',(17.3433874196244,1.98904339107765,3.32044700979421));
#80632=CARTESIAN_POINT('Ctrl Pts',(17.3668782451022,1.96068600822823,3.31852854357645));
#80633=CARTESIAN_POINT('Ctrl Pts',(17.428111909547,1.88676666181879,3.31352766709645));
#80634=CARTESIAN_POINT('Ctrl Pts',(17.4859862459092,1.80984705629152,3.30852679061646));
#80635=CARTESIAN_POINT('Ctrl Pts',(17.540193809841,1.73026519887715,3.30352591413646));
#80636=CARTESIAN_POINT('Ctrl Pts',(17.5943281628246,1.65079082209502,3.29853179167533));
#80637=CARTESIAN_POINT('Ctrl Pts',(17.6448053409217,1.56866169897679,3.29353766921419));
#80638=CARTESIAN_POINT('Ctrl Pts',(17.6913576793253,1.48424933617532,3.28854354675306));
#80639=CARTESIAN_POINT('Ctrl Pts',(17.7378611588566,1.39992556812542,3.28355466585873));
#80640=CARTESIAN_POINT('Ctrl Pts',(17.7804477770603,1.31332370643703,3.2785657849644));
#80641=CARTESIAN_POINT('Ctrl Pts',(17.8188933647738,1.22484384638785,3.27357690407007));
#80642=CARTESIAN_POINT('Ctrl Pts',(17.8573116557536,1.13642680788265,3.26859156532873));
#80643=CARTESIAN_POINT('Ctrl Pts',(17.8915945869304,1.04613482298226,3.26360622658738));
#80644=CARTESIAN_POINT('Ctrl Pts',(17.9215645623794,0.954391302270142,3.25862088784604));
#80645=CARTESIAN_POINT('Ctrl Pts',(17.9515237376556,0.862680842842486,3.25363734565339));
#80646=CARTESIAN_POINT('Ctrl Pts',(17.977172909325,0.769520303512664,3.24865380346074));
#80647=CARTESIAN_POINT('Ctrl Pts',(17.9983834837999,0.675350822962396,3.24367026126809));
#80648=CARTESIAN_POINT('Ctrl Pts',(18.0195921957061,0.581189611737178,3.23868715669631));
#80649=CARTESIAN_POINT('Ctrl Pts',(18.0363629891924,0.486020063444048,3.23370405212454));
#80650=CARTESIAN_POINT('Ctrl Pts',(18.0486180445656,0.39029510418242,3.22872094755276));
#80651=CARTESIAN_POINT('Ctrl Pts',(18.0608753638864,0.294552461092729,3.22373692242312));
#80652=CARTESIAN_POINT('Ctrl Pts',(18.0686152326411,0.198254638372426,3.21875289729347));
#80653=CARTESIAN_POINT('Ctrl Pts',(18.0718116384515,0.101860236961538,3.21376887216383));
#80654=CARTESIAN_POINT('Ctrl Pts',(18.0750114778239,0.00536228919936145,
3.208779493221));
#80655=CARTESIAN_POINT('Ctrl Pts',(18.073658096343,-0.0912320052277161,
3.20379011427817));
#80656=CARTESIAN_POINT('Ctrl Pts',(18.0677776329475,-0.187463715921185,
3.19880073533534));
#80657=CARTESIAN_POINT('Ctrl Pts',(18.0618936839234,-0.283752467697744,
3.19380839895181));
#80658=CARTESIAN_POINT('Ctrl Pts',(18.0514773571495,-0.379677771915711,
3.18881606256827));
#80659=CARTESIAN_POINT('Ctrl Pts',(18.0366064918961,-0.474787598168444,
3.18382372618473));
#80660=CARTESIAN_POINT('Ctrl Pts',(18.0217118217248,-0.570049673907353,
3.17882339819108));
#80661=CARTESIAN_POINT('Ctrl Pts',(18.0023484632009,-0.664493235810517,
3.17382307019743));
#80662=CARTESIAN_POINT('Ctrl Pts',(17.978644976644,-0.757678264907645,3.16882274220378));
#80663=CARTESIAN_POINT('Ctrl Pts',(17.9654993048104,-0.809357574167647,
3.16604961974743));
#80664=CARTESIAN_POINT('Ctrl Pts',(17.9510196326832,-0.860650087983236,
3.16327649729108));
#80665=CARTESIAN_POINT('Ctrl Pts',(17.9352342955905,-0.911483340489089,
3.16050337483472));
#80666=CARTESIAN_POINT('Ctrl Pts',(17.9067680010694,-1.00315286447835,3.1555024983807));
#80667=CARTESIAN_POINT('Ctrl Pts',(17.8739535732588,-1.09364749386917,3.15050162192668));
#80668=CARTESIAN_POINT('Ctrl Pts',(17.8369061867942,-1.18252506837228,3.14550074547265));
#80669=CARTESIAN_POINT('Ctrl Pts',(17.7999088352689,-1.27128260784792,3.14050662303218));
#80670=CARTESIAN_POINT('Ctrl Pts',(17.7586900546112,-1.35842703147765,3.13551250059171));
#80671=CARTESIAN_POINT('Ctrl Pts',(17.7134148091021,-1.44353119943615,3.13051837815124));
#80672=CARTESIAN_POINT('Ctrl Pts',(17.6681870820484,-1.52854604665064,3.12552949727229));
#80673=CARTESIAN_POINT('Ctrl Pts',(17.6189115588135,-1.61152450989622,3.12054061639334));
#80674=CARTESIAN_POINT('Ctrl Pts',(17.5658009099349,-1.69206026505481,3.11555173551439));
#80675=CARTESIAN_POINT('Ctrl Pts',(17.512727970039,-1.77253883918726,3.1105663967805));
#80676=CARTESIAN_POINT('Ctrl Pts',(17.4558255585379,-1.85057778790208,3.10558105804662));
#80677=CARTESIAN_POINT('Ctrl Pts',(17.3953513163893,-1.92579706123772,3.10059571931274));
#80678=CARTESIAN_POINT('Ctrl Pts',(17.3348988670677,-2.00098922814678,3.09561217712265));
#80679=CARTESIAN_POINT('Ctrl Pts',(17.2708774192136,-2.07336339710243,3.09062863493255));
#80680=CARTESIAN_POINT('Ctrl Pts',(17.2035862312026,-2.142570879027,3.08564509274246));
#80681=CARTESIAN_POINT('Ctrl Pts',(17.1363009521811,-2.21177228368797,3.08066198816834));
#80682=CARTESIAN_POINT('Ctrl Pts',(17.0657468098319,-2.27780723983766,3.07567888359422));
#80683=CARTESIAN_POINT('Ctrl Pts',(16.9922606716825,-2.34036314833129,3.0706957790201));
#80684=CARTESIAN_POINT('Ctrl Pts',(16.9187609579395,-2.40293061320298,3.06571175388321));
#80685=CARTESIAN_POINT('Ctrl Pts',(16.8423285067147,-2.46201746966545,3.06072772874632));
#80686=CARTESIAN_POINT('Ctrl Pts',(16.7633332392227,-2.51735141318259,3.05574370360943));
#80687=CARTESIAN_POINT('Ctrl Pts',(16.6842531153189,-2.57274479620856,3.05075432465195));
#80688=CARTESIAN_POINT('Ctrl Pts',(16.6026050391149,-2.62437696616575,3.04576494569447));
#80689=CARTESIAN_POINT('Ctrl Pts',(16.5187876960584,-2.67201912124551,3.04077556673699));
#80690=CARTESIAN_POINT('Ctrl Pts',(16.4349206704307,-2.71968951612242,3.03578323033459));
#80691=CARTESIAN_POINT('Ctrl Pts',(16.3488822085863,-2.76336498837243,3.03079089393219));
#80692=CARTESIAN_POINT('Ctrl Pts',(16.2610934583573,-2.8028638103355,3.02579855752978));
#80693=CARTESIAN_POINT('Ctrl Pts',(16.1731641779293,-2.84242586109833,3.02079822951084));
#80694=CARTESIAN_POINT('Ctrl Pts',(16.0834794224651,-2.87779775104511,3.01579790149191));
#80695=CARTESIAN_POINT('Ctrl Pts',(15.9924779858168,-2.9088467985903,3.01079757347297));
#80696=CARTESIAN_POINT('Ctrl Pts',(15.9420096711571,-2.92606623115213,3.00802445101297));
#80697=CARTESIAN_POINT('Ctrl Pts',(15.891136628461,-2.94195699421057,3.00525132855297));
#80698=CARTESIAN_POINT('Ctrl Pts',(15.8399350346931,-2.95650323651018,3.00247820609297));
#80699=CARTESIAN_POINT('Ctrl Pts',(15.7476012654901,-2.98273502502342,2.99747732955086));
#80700=CARTESIAN_POINT('Ctrl Pts',(15.6538763853701,-3.00468295413782,2.99247645300875));
#80701=CARTESIAN_POINT('Ctrl Pts',(15.5591936696892,-3.02220196045525,2.98747557646664));
#80702=CARTESIAN_POINT('Ctrl Pts',(15.4646388293375,-3.03969730618494,2.98248145394219));
#80703=CARTESIAN_POINT('Ctrl Pts',(15.3691291521665,-3.05277553816698,2.97748733141774));
#80704=CARTESIAN_POINT('Ctrl Pts',(15.2731125303631,-3.06134150263551,2.9724932088933));
#80705=CARTESIAN_POINT('Ctrl Pts',(15.177196682505,-3.06989847672282,2.96750432793453));
#80706=CARTESIAN_POINT('Ctrl Pts',(15.080775382386,-3.07395255927076,2.96251544697577));
#80707=CARTESIAN_POINT('Ctrl Pts',(14.9843051467686,-3.07345992678968,2.95752656601701));
#80708=CARTESIAN_POINT('Ctrl Pts',(14.8879034059093,-3.07296764408222,2.95254122720979));
#80709=CARTESIAN_POINT('Ctrl Pts',(14.7914532360493,-3.06793506620663,2.94755588840257));
#80710=CARTESIAN_POINT('Ctrl Pts',(14.6954137119675,-3.0583703901167,2.94257054959536));
#80711=CARTESIAN_POINT('Ctrl Pts',(14.5994087972882,-3.04880916081317,2.93758700733596));
#80712=CARTESIAN_POINT('Ctrl Pts',(14.5038146704269,-3.03471912183679,2.93260346507656));
#80713=CARTESIAN_POINT('Ctrl Pts',(14.409086871846,-3.01616046074728,2.92761992281716));
#80714=CARTESIAN_POINT('Ctrl Pts',(14.3143673916023,-2.99760342935046,2.92263681817782));
#80715=CARTESIAN_POINT('Ctrl Pts',(14.2205145188283,-2.97457864058691,2.91765371353848));
#80716=CARTESIAN_POINT('Ctrl Pts',(14.1279741089871,-2.94719749854046,2.91267060889915));
#80717=CARTESIAN_POINT('Ctrl Pts',(14.0354166036046,-2.9198112982125,2.9076865837012));
#80718=CARTESIAN_POINT('Ctrl Pts',(13.9441724633098,-2.88806727078575,2.90270255850325));
#80719=CARTESIAN_POINT('Ctrl Pts',(13.8546718481927,-2.8521265179998,2.8977185333053));
#80720=CARTESIAN_POINT('Ctrl Pts',(13.7650750919802,-2.81614715784409,2.8927291542934));
#80721=CARTESIAN_POINT('Ctrl Pts',(13.6772260076248,-2.77596223628351,2.8877397752815));
#80722=CARTESIAN_POINT('Ctrl Pts',(13.591534029511,-2.73178071227809,2.8827503962696));
#80723=CARTESIAN_POINT('Ctrl Pts',(13.5057912577034,-2.68757299979087,2.87775805981645));
#80724=CARTESIAN_POINT('Ctrl Pts',(13.422208517895,-2.63936418685725,2.8727657233633));
#80725=CARTESIAN_POINT('Ctrl Pts',(13.3411680848319,-2.58740776206991,2.86777338691015));
#80726=CARTESIAN_POINT('Ctrl Pts',(13.259997924222,-2.53536816670624,2.86277305884669));
#80727=CARTESIAN_POINT('Ctrl Pts',(13.1813785536951,-2.47956923479637,2.85777273078323));
#80728=CARTESIAN_POINT('Ctrl Pts',(13.1056608056481,-2.42030602749783,2.85277240271977));
#80729=CARTESIAN_POINT('Ctrl Pts',(13.063668653474,-2.38743936567286,2.84999928093026));
#80730=CARTESIAN_POINT('Ctrl Pts',(13.022568326117,-2.35350789677246,2.84722615914075));
#80731=CARTESIAN_POINT('Ctrl Pts',(12.9824147133544,-2.31856676874125,2.84445303735124));
#80732=CARTESIAN_POINT('Ctrl Pts',(12.9110410684898,-2.2564583931385,2.83952377205846));
#80733=CARTESIAN_POINT('Ctrl Pts',(12.8423960887178,-2.19092748208239,2.83459450676568));
#80734=CARTESIAN_POINT('Ctrl Pts',(12.7768328506208,-2.12224646917393,2.82966524147289));
#80735=CARTESIAN_POINT('Ctrl Pts',(12.7096405802844,-2.05185895750933,2.82461350004392));
#80736=CARTESIAN_POINT('Ctrl Pts',(12.6456856417414,-1.97816296524106,2.81956175861494));
#80737=CARTESIAN_POINT('Ctrl Pts',(12.5853131208015,-1.90149665406668,2.81451001718596));
#80738=CARTESIAN_POINT('Ctrl Pts',(12.5265519994705,-1.82687663915281,2.80959311150735));
#80739=CARTESIAN_POINT('Ctrl Pts',(12.4711847807881,-1.74944324348275,2.80467620582875));
#80740=CARTESIAN_POINT('Ctrl Pts',(12.4194921084729,-1.66954522902682,2.79975930015014));
#80741=CARTESIAN_POINT('Ctrl Pts',(12.3678305275951,-1.58969527059142,2.79484535182813));
#80742=CARTESIAN_POINT('Ctrl Pts',(12.3198393500791,-1.5073840154634,2.78993140350612));
#80743=CARTESIAN_POINT('Ctrl Pts',(12.2757571653357,-1.4229909443774,2.78501745518411));
#80744=CARTESIAN_POINT('Ctrl Pts',(12.2316886534711,-1.33862404931331,2.78010503101115));
#80745=CARTESIAN_POINT('Ctrl Pts',(12.1915269348586,-1.25217702194179,2.77519260683818));
#80746=CARTESIAN_POINT('Ctrl Pts',(12.1554650790604,-1.16405469525924,2.77028018266522));
#80747=CARTESIAN_POINT('Ctrl Pts',(12.1176244835151,-1.07158576240239,2.76512545470791));
#80748=CARTESIAN_POINT('Ctrl Pts',(12.084298822646,-0.977272503217062,2.75997072675059));
#80749=CARTESIAN_POINT('Ctrl Pts',(12.0556539747487,-0.881605769937465,
2.75481599879328));
#80750=CARTESIAN_POINT('Ctrl Pts',(12.0283356592049,-0.790369327832824,
2.74989998438869));
#80751=CARTESIAN_POINT('Ctrl Pts',(12.0052743578697,-0.697902448005611,
2.7449839699841));
#80752=CARTESIAN_POINT('Ctrl Pts',(11.9865621544327,-0.604644193640178,
2.74006795557951));
#80753=CARTESIAN_POINT('Ctrl Pts',(11.9678412361408,-0.511342506006135,
2.73514965163416));
#80754=CARTESIAN_POINT('Ctrl Pts',(11.9534735149745,-0.417249157219473,
2.73023134768882));
#80755=CARTESIAN_POINT('Ctrl Pts',(11.9434993964955,-0.322810022732573,
2.72531304374347));
#80756=CARTESIAN_POINT('Ctrl Pts',(11.9335132389539,-0.228256897355436,
2.72038880325658));
#80757=CARTESIAN_POINT('Ctrl Pts',(11.9279312866406,-0.133357604235048,
2.71546456276969));
#80758=CARTESIAN_POINT('Ctrl Pts',(11.9267418836813,-0.038559051874358,
2.71054032228281));
#80759=CARTESIAN_POINT('Ctrl Pts',(11.9265714467364,-0.0249747779103842,
2.70983469724769));
#80760=CARTESIAN_POINT('Ctrl Pts',(11.926491118504,-0.0113925648463264,
2.70912907221258));
#80761=CARTESIAN_POINT('Ctrl Pts',(11.9265007775872,0.00218628177021425,
2.70842344717746));
#80762=CARTESIAN_POINT('Ctrl Pts',(11.9237226922662,0.00218825791429551,
2.70842344717746));
#80763=CARTESIAN_POINT('Ctrl Pts',(11.9225818664433,0.14340888213774,2.70109158765481));
#80764=CARTESIAN_POINT('Ctrl Pts',(11.9953557666493,1.29803405602119,2.64108467188491));
#80765=CARTESIAN_POINT('Ctrl Pts',(13.4561116265877,3.28204067332613,2.52840269986777));
#80766=CARTESIAN_POINT('Ctrl Pts',(15.8744262025005,3.14463381132417,2.41762058301274));
#80767=CARTESIAN_POINT('Ctrl Pts',(16.7921285915167,2.50458207762493,2.35951352240495));
#80768=CARTESIAN_POINT('Ctrl Pts',(16.8745674052796,2.44028174751842,2.35408151804441));
#80769=CARTESIAN_POINT('',(11.9265010538313,-0.00254517192390105,2.79157655284934));
#80770=CARTESIAN_POINT('Ctrl Pts',(11.9265010538309,-0.00254517140556233,
2.79157655282255));
#80771=CARTESIAN_POINT('Ctrl Pts',(11.9264216029999,0.0933980899065408,
2.7866185005732));
#80772=CARTESIAN_POINT('Ctrl Pts',(11.9308389262345,0.18941702310935,2.78166044832386));
#80773=CARTESIAN_POINT('Ctrl Pts',(11.9397475440067,0.285056407727899,2.77670239607451));
#80774=CARTESIAN_POINT('Ctrl Pts',(11.9486532096028,0.380664098956192,2.77174598684583));
#80775=CARTESIAN_POINT('Ctrl Pts',(11.9620471721085,0.475892049971424,2.76678957761714));
#80776=CARTESIAN_POINT('Ctrl Pts',(11.9798719422631,0.570288317319068,2.76183316838845));
#80777=CARTESIAN_POINT('Ctrl Pts',(11.9976957965019,0.664679734166605,2.75687701384212));
#80778=CARTESIAN_POINT('Ctrl Pts',(12.019949922976,0.758239116294989,2.75192085929579));
#80779=CARTESIAN_POINT('Ctrl Pts',(12.0465255813558,0.850524019892715,2.74696470474945));
#80780=CARTESIAN_POINT('Ctrl Pts',(12.0731073154434,0.942830021598326,2.74200741713065));
#80781=CARTESIAN_POINT('Ctrl Pts',(12.1040124203163,1.03386053986693,2.73705012951185));
#80782=CARTESIAN_POINT('Ctrl Pts',(12.1390824255821,1.12318871183192,2.73209284189306));
#80783=CARTESIAN_POINT('Ctrl Pts',(12.1741916518084,1.21261678502838,2.72713001023225));
#80784=CARTESIAN_POINT('Ctrl Pts',(12.2134749116354,1.30033829888587,2.72216717857144));
#80785=CARTESIAN_POINT('Ctrl Pts',(12.256725873535,1.38594708306904,2.71720434691064));
#80786=CARTESIAN_POINT('Ctrl Pts',(12.3000047118528,1.47161104443597,2.71223831657019));
#80787=CARTESIAN_POINT('Ctrl Pts',(12.347256123295,1.55515918055392,2.70727228622975));
#80788=CARTESIAN_POINT('Ctrl Pts',(12.3982292736095,1.6362124975985,2.70230625588931));
#80789=CARTESIAN_POINT('Ctrl Pts',(12.4492835184772,1.71739476454095,2.69733232495789));
#80790=CARTESIAN_POINT('Ctrl Pts',(12.5040710654416,1.79607392841595,2.69235839402647));
#80791=CARTESIAN_POINT('Ctrl Pts',(12.5622996527535,1.87190257947215,2.68738446309506));
#80792=CARTESIAN_POINT('Ctrl Pts',(12.5853736915098,1.90195093396744,2.68541346087122));
#80793=CARTESIAN_POINT('Ctrl Pts',(12.6089876478043,1.93155207612388,2.68344245864738));
#80794=CARTESIAN_POINT('Ctrl Pts',(12.6331217549488,1.96068600828974,2.68147145642354));
#80795=CARTESIAN_POINT('Ctrl Pts',(12.6943554201245,2.03460535557759,2.67647057988345));
#80796=CARTESIAN_POINT('Ctrl Pts',(12.759162058285,2.10578234896022,2.67146970334336));
#80797=CARTESIAN_POINT('Ctrl Pts',(12.8272667762959,2.17385201626343,2.66646882680326));
#80798=CARTESIAN_POINT('Ctrl Pts',(12.8952795143374,2.2418297509354,2.66147470428089));
#80799=CARTESIAN_POINT('Ctrl Pts',(12.9665811718247,2.30670819277677,2.65648058175851));
#80800=CARTESIAN_POINT('Ctrl Pts',(13.0408565389775,2.36815522065864,2.65148645923613));
#80801=CARTESIAN_POINT('Ctrl Pts',(13.1150539506503,2.42953775700402,2.64649757827947));
#80802=CARTESIAN_POINT('Ctrl Pts',(13.1922185311815,2.4874957608074,2.64150869732281));
#80803=CARTESIAN_POINT('Ctrl Pts',(13.2719988876619,2.5417345270028,2.63651981636615));
#80804=CARTESIAN_POINT('Ctrl Pts',(13.3517225993516,2.59593478317276,2.63153447756109));
#80805=CARTESIAN_POINT('Ctrl Pts',(13.4340580331092,2.64642080545337,2.62654913875604));
#80806=CARTESIAN_POINT('Ctrl Pts',(13.5186222214209,2.69293930996079,2.62156379995098));
#80807=CARTESIAN_POINT('Ctrl Pts',(13.6031559356531,2.7394410507691,2.61658025769378));
#80808=CARTESIAN_POINT('Ctrl Pts',(13.6899164246177,2.78197790344047,2.61159671543658));
#80809=CARTESIAN_POINT('Ctrl Pts',(13.7784941838012,2.8203414316342,2.60661317317938));
#80810=CARTESIAN_POINT('Ctrl Pts',(13.8670641647007,2.85870159100919,2.60163006854227));
#80811=CARTESIAN_POINT('Ctrl Pts',(13.9574506959103,2.89288898040133,2.59664696390515));
#80812=CARTESIAN_POINT('Ctrl Pts',(14.0492232431778,2.92274285709274,2.59166385926804));
#80813=CARTESIAN_POINT('Ctrl Pts',(14.1410127441345,2.95260224886859,2.58667983407233));
#80814=CARTESIAN_POINT('Ctrl Pts',(14.2341883525122,2.97812640235122,2.58169580887662));
#80815=CARTESIAN_POINT('Ctrl Pts',(14.3283043178312,2.99920442126837,2.57671178368091));
#80816=CARTESIAN_POINT('Ctrl Pts',(14.42252138203,3.0203050820837,2.57172240467128));
#80817=CARTESIAN_POINT('Ctrl Pts',(14.5176803909867,3.03694997767989,2.56673302566166));
#80818=CARTESIAN_POINT('Ctrl Pts',(14.6133255659997,3.04907939091302,2.56174364665203));
#80819=CARTESIAN_POINT('Ctrl Pts',(14.7090274344377,3.06121599382383,2.55675131020117));
#80820=CARTESIAN_POINT('Ctrl Pts',(14.8052156056642,3.06883175028921,2.5517589737503));
#80821=CARTESIAN_POINT('Ctrl Pts',(14.9014314598568,3.07191902446891,2.54676663729944));
#80822=CARTESIAN_POINT('Ctrl Pts',(14.9978013340396,3.07501124068175,2.54176630923828));
#80823=CARTESIAN_POINT('Ctrl Pts',(15.0941985414059,3.07356050695242,2.53676598117711));
#80824=CARTESIAN_POINT('Ctrl Pts',(15.1901668254077,3.06761125772389,2.53176565311594));
#80825=CARTESIAN_POINT('Ctrl Pts',(15.2433896816504,3.06431187564433,2.52899253130457));
#80826=CARTESIAN_POINT('Ctrl Pts',(15.2964807342468,3.05962981736536,2.52621940949319));
#80827=CARTESIAN_POINT('Ctrl Pts',(15.3493635103379,3.05357943856786,2.52344628768182));
#80828=CARTESIAN_POINT('Ctrl Pts',(15.4447236617431,3.0426691747573,2.5184456932474));
#80829=CARTESIAN_POINT('Ctrl Pts',(15.5397385953953,3.02726860088142,2.51344509881299));
#80830=CARTESIAN_POINT('Ctrl Pts',(15.6339525189152,3.00740859441499,2.50844450437857));
#80831=CARTESIAN_POINT('Ctrl Pts',(15.7280447702709,2.98757423606801,2.50345036794022));
#80832=CARTESIAN_POINT('Ctrl Pts',(15.8213376413766,2.96329197781237,2.49845623150185));
#80833=CARTESIAN_POINT('Ctrl Pts',(15.9133807516656,2.93464441670313,2.4934620950635));
#80834=CARTESIAN_POINT('Ctrl Pts',(16.0053187419076,2.90602957322977,2.48847366229872));
#80835=CARTESIAN_POINT('Ctrl Pts',(16.0960093935895,2.8730594723877,2.48348522953395));
#80836=CARTESIAN_POINT('Ctrl Pts',(16.1850140219671,2.83586741892873,2.47849679676917));
#80837=CARTESIAN_POINT('Ctrl Pts',(16.2739586339688,2.79870044430329,2.47351172773571));
#80838=CARTESIAN_POINT('Ctrl Pts',(16.3612190785803,2.75731734333633,2.46852665870225));
#80839=CARTESIAN_POINT('Ctrl Pts',(16.4463740661562,2.71190049794435,2.46354158966879));
#80840=CARTESIAN_POINT('Ctrl Pts',(16.5315057777478,2.6664960666435,2.45855788323771));
#80841=CARTESIAN_POINT('Ctrl Pts',(16.6145327864978,2.61706028285798,2.45357417680662));
#80842=CARTESIAN_POINT('Ctrl Pts',(16.6950567625211,2.56382230699233,2.44859047037553));
#80843=CARTESIAN_POINT('Ctrl Pts',(16.7556094151612,2.52378825975504,2.4448428083836));
#80844=CARTESIAN_POINT('Ctrl Pts',(16.8147470884424,2.48160514568058,2.44109514639167));
#80845=CARTESIAN_POINT('Ctrl Pts',(16.8723108164276,2.43738680900022,2.43734748439974));
#80846=CARTESIAN_POINT('Ctrl Pts',(16.8723108164276,2.43738680900022,3.43723392788203));
#80847=CARTESIAN_POINT('Ctrl Pts',(16.9512302592254,2.37676379839261,3.43208135302821));
#80848=CARTESIAN_POINT('Ctrl Pts',(17.0272819369425,2.31224276762403,3.4269287781744));
#80849=CARTESIAN_POINT('Ctrl Pts',(17.1000649707149,2.24413220839957,3.42177620332058));
#80850=CARTESIAN_POINT('Ctrl Pts',(17.1704753050321,2.17824202772195,3.41679160046401));
#80851=CARTESIAN_POINT('Ctrl Pts',(17.2378264618397,2.10899305298184,3.41180699760745));
#80852=CARTESIAN_POINT('Ctrl Pts',(17.301789126522,2.03670544434512,3.40682239475088));
#80853=CARTESIAN_POINT('Ctrl Pts',(17.3657344160622,1.96443747228039,3.40183914593706));
#80854=CARTESIAN_POINT('Ctrl Pts',(17.4262927521021,1.88913283495649,3.39685589712325));
#80855=CARTESIAN_POINT('Ctrl Pts',(17.4831730360029,1.81114712910573,3.39187264830943));
#80856=CARTESIAN_POINT('Ctrl Pts',(17.5400533715129,1.73316135249643,3.38688939497419));
#80857=CARTESIAN_POINT('Ctrl Pts',(17.5932553903981,1.65249485746842,3.38190614163894));
#80858=CARTESIAN_POINT('Ctrl Pts',(17.6425301527128,1.56953389323185,3.37692288830369));
#80859=CARTESIAN_POINT('Ctrl Pts',(17.6918183894875,1.4865502428547,3.37193827226989));
#80860=CARTESIAN_POINT('Ctrl Pts',(17.7371770124854,1.40127125400007,3.36695365623609));
#80861=CARTESIAN_POINT('Ctrl Pts',(17.7784025697423,1.31410859918402,3.36196904020229));
#80862=CARTESIAN_POINT('Ctrl Pts',(17.8196743521061,1.22684821123074,3.35697883505278));
#80863=CARTESIAN_POINT('Ctrl Pts',(17.8568036333464,1.13770033958764,3.35198862990328));
#80864=CARTESIAN_POINT('Ctrl Pts',(17.889634861312,1.04709723440101,3.34699842475377));
#80865=CARTESIAN_POINT('Ctrl Pts',(17.9224881621865,0.956433215437768,3.34200486461725));
#80866=CARTESIAN_POINT('Ctrl Pts',(17.9510375280809,0.864312433644861,3.33701130448073));
#80867=CARTESIAN_POINT('Ctrl Pts',(17.975177680863,0.771180923840089,3.33201774434421));
#80868=CARTESIAN_POINT('Ctrl Pts',(17.9993542688009,0.677908849014769,3.32701664733982));
#80869=CARTESIAN_POINT('Ctrl Pts',(18.0191082754717,0.583623430262389,3.32201555033544));
#80870=CARTESIAN_POINT('Ctrl Pts',(18.0343857991061,0.488779165046244,3.31701445333105));
#80871=CARTESIAN_POINT('Ctrl Pts',(18.0378910403734,0.467018306391696,3.3158670126842));
#80872=CARTESIAN_POINT('Ctrl Pts',(18.0411608484674,0.445228040187508,3.31471957203734));
#80873=CARTESIAN_POINT('Ctrl Pts',(18.0441949589413,0.423413866041879,3.31357213139049));
#80874=CARTESIAN_POINT('Ctrl Pts',(18.0574184878613,0.32834140076324,3.30857125396422));
#80875=CARTESIAN_POINT('Ctrl Pts',(18.0662070432973,0.232483017404805,3.30357037653796));
#80876=CARTESIAN_POINT('Ctrl Pts',(18.0704768138282,0.136287878197188,3.2985694991117));
#80877=CARTESIAN_POINT('Ctrl Pts',(18.0747408177609,0.0402226566778314,
3.29357537569027));
#80878=CARTESIAN_POINT('Ctrl Pts',(18.0744981468719,-0.0561779822314671,
3.28858125226883));
#80879=CARTESIAN_POINT('Ctrl Pts',(18.0697164401893,-0.152457295107154,
3.2835871288474));
#80880=CARTESIAN_POINT('Ctrl Pts',(18.0649397521201,-0.248635558570522,
3.27859824698016));
#80881=CARTESIAN_POINT('Ctrl Pts',(18.0556335204819,-0.344692313312812,
3.27360936511292));
#80882=CARTESIAN_POINT('Ctrl Pts',(18.0418174138874,-0.440169365779964,
3.26862048324569));
#80883=CARTESIAN_POINT('Ctrl Pts',(18.0280111168177,-0.535578628924582,
3.26363514351673));
#80884=CARTESIAN_POINT('Ctrl Pts',(18.0097013730412,-0.630408575110616,
3.25864980378777));
#80885=CARTESIAN_POINT('Ctrl Pts',(17.9869597261553,-0.724205664384442,
3.25366446405881));
#80886=CARTESIAN_POINT('Ctrl Pts',(17.9642262745538,-0.817968952507546,
3.24868092086982));
#80887=CARTESIAN_POINT('Ctrl Pts',(17.9370641964582,-0.910699697378456,
3.24369737768082));
#80888=CARTESIAN_POINT('Ctrl Pts',(17.9055960391893,-1.00195504242819,3.23871383449183));
#80889=CARTESIAN_POINT('Ctrl Pts',(17.8741306451927,-1.09320237419135,3.23373072891621));
#80890=CARTESIAN_POINT('Ctrl Pts',(17.8383600670373,-1.1829741490899,3.2287476233406));
#80891=CARTESIAN_POINT('Ctrl Pts',(17.7984562393385,-1.27084417868895,3.22376451776498));
#80892=CARTESIAN_POINT('Ctrl Pts',(17.7585450399249,-1.35873044113655,3.21878049162523));
#80893=CARTESIAN_POINT('Ctrl Pts',(17.714499255917,-1.44471386115675,3.21379646548547));
#80894=CARTESIAN_POINT('Ctrl Pts',(17.6665378745369,-1.52839066133637,3.20881243934572));
#80895=CARTESIAN_POINT('Ctrl Pts',(17.6185249732746,-1.61215734672715,3.20382305938936));
#80896=CARTESIAN_POINT('Ctrl Pts',(17.5665882962256,-1.69361208458467,3.19883367943301));
#80897=CARTESIAN_POINT('Ctrl Pts',(17.5109913654501,-1.77237823633529,3.19384429947665));
#80898=CARTESIAN_POINT('Ctrl Pts',(17.4553614797148,-1.85119107655109,3.18885196207617));
#80899=CARTESIAN_POINT('Ctrl Pts',(17.3960672896008,-1.92731181151864,3.1838596246757));
#80900=CARTESIAN_POINT('Ctrl Pts',(17.3334126674274,-2.00039685399905,3.17886728727522));
#80901=CARTESIAN_POINT('Ctrl Pts',(17.2706577493435,-2.07359888913899,3.17386695826921));
#80902=CARTESIAN_POINT('Ctrl Pts',(17.2045319589979,-2.14375520994463,3.16886662926321));
#80903=CARTESIAN_POINT('Ctrl Pts',(17.1353759985662,-2.21055911360623,3.1638663002572));
#80904=CARTESIAN_POINT('Ctrl Pts',(17.0970230700705,-2.2476076243112,3.16109318772105));
#80905=CARTESIAN_POINT('Ctrl Pts',(17.0577387654674,-2.28362575726213,3.15832007518491));
#80906=CARTESIAN_POINT('Ctrl Pts',(17.01758528669,-2.31856676870264,3.15554696264876));
#80907=CARTESIAN_POINT('Ctrl Pts',(16.9451747419857,-2.38157744045409,3.15054608612742));
#80908=CARTESIAN_POINT('Ctrl Pts',(16.8696832447064,-2.44130263317381,3.14554520960607));
#80909=CARTESIAN_POINT('Ctrl Pts',(16.7914412364284,-2.49742678499768,3.14054433308473));
#80910=CARTESIAN_POINT('Ctrl Pts',(16.7133048991478,-2.55347513744941,3.13555021057726));
#80911=CARTESIAN_POINT('Ctrl Pts',(16.6324257872682,-2.60593186144669,3.1305560880698));
#80912=CARTESIAN_POINT('Ctrl Pts',(16.5491687979154,-2.65452034943514,3.12556196556233));
#80913=CARTESIAN_POINT('Ctrl Pts',(16.4659991906131,-2.70305784156442,3.12057308461678));
#80914=CARTESIAN_POINT('Ctrl Pts',(16.3804570441074,-2.74773494872369,3.11558420367123));
#80915=CARTESIAN_POINT('Ctrl Pts',(16.2929368919671,-2.78831785192979,3.11059532272568));
#80916=CARTESIAN_POINT('Ctrl Pts',(16.2054788798438,-2.82887194094588,3.10560998392601));
#80917=CARTESIAN_POINT('Ctrl Pts',(16.1160460508533,-2.86533742089797,3.10062464512633));
#80918=CARTESIAN_POINT('Ctrl Pts',(16.0250573779798,-2.89752646611713,3.09563930632666));
#80919=CARTESIAN_POINT('Ctrl Pts',(15.9341014942885,-2.92970391151363,3.0906557640713));
#80920=CARTESIAN_POINT('Ctrl Pts',(15.8415912938814,-2.9576078380647,3.08567222181594));
#80921=CARTESIAN_POINT('Ctrl Pts',(15.7479646625862,-2.98109897747832,3.08068867956058));
#80922=CARTESIAN_POINT('Ctrl Pts',(15.6543462528656,-3.00458805407979,3.07570557492177));
#80923=CARTESIAN_POINT('Ctrl Pts',(15.5596120327128,-3.02366500743946,3.07072247028296));
#80924=CARTESIAN_POINT('Ctrl Pts',(15.4642129048914,-3.03824104194059,3.06573936564415));
#80925=CARTESIAN_POINT('Ctrl Pts',(15.3687961533535,-3.0528197691697,3.06075534044322));
#80926=CARTESIAN_POINT('Ctrl Pts',(15.2727146838301,-3.0628958599669,3.05577131524229));
#80927=CARTESIAN_POINT('Ctrl Pts',(15.1764263303416,-3.06843217294471,3.05078729004136));
#80928=CARTESIAN_POINT('Ctrl Pts',(15.0800345443018,-3.07397443300704,3.04579791102115));
#80929=CARTESIAN_POINT('Ctrl Pts',(14.9834358692918,-3.074967154573,3.04080853200095));
#80930=CARTESIAN_POINT('Ctrl Pts',(14.8870897351376,-3.07142532419212,3.03581915298074));
#80931=CARTESIAN_POINT('Ctrl Pts',(14.7906864920082,-3.06788139439849,3.03082681651627));
#80932=CARTESIAN_POINT('Ctrl Pts',(14.6945365247006,-3.05979759740087,3.02583448005179));
#80933=CARTESIAN_POINT('Ctrl Pts',(14.5990936205754,-3.04724077239339,3.02084214358732));
#80934=CARTESIAN_POINT('Ctrl Pts',(14.5034979336912,-3.03466384671539,3.0158418155079));
#80935=CARTESIAN_POINT('Ctrl Pts',(14.4086120013494,-3.0175996735953,3.01084148742848));
#80936=CARTESIAN_POINT('Ctrl Pts',(14.3148788347279,-2.99616609000505,3.00584115934905));
#80937=CARTESIAN_POINT('Ctrl Pts',(14.2628955478462,-2.98427928232712,3.00306803753504));
#80938=CARTESIAN_POINT('Ctrl Pts',(14.2112665472188,-2.97104947544008,3.00029491572103));
#80939=CARTESIAN_POINT('Ctrl Pts',(14.1600649653834,-2.95650323653191,2.99752179390702));
#80940=CARTESIAN_POINT('Ctrl Pts',(14.0677311973554,-2.93027144835505,2.99252091742801));
#80941=CARTESIAN_POINT('Ctrl Pts',(13.976466386845,-2.8996642779387,2.98752004094901));
#80942=CARTESIAN_POINT('Ctrl Pts',(13.886715360663,-2.86478612845989,2.98251916447001));
#80943=CARTESIAN_POINT('Ctrl Pts',(13.7970855492583,-2.82995508426004,2.97752504200993));
#80944=CARTESIAN_POINT('Ctrl Pts',(13.7089658642828,-2.7908646827843,2.97253091954985));
#80945=CARTESIAN_POINT('Ctrl Pts',(13.6227873256133,-2.7476694669317,2.96753679708977));
#80946=CARTESIAN_POINT('Ctrl Pts',(13.5366992353812,-2.70451958649365,2.96254791619655));
#80947=CARTESIAN_POINT('Ctrl Pts',(13.4525486314016,-2.65727365182197,2.95755903530334));
#80948=CARTESIAN_POINT('Ctrl Pts',(13.3707468824896,-2.60613440349547,2.95257015441012));
#80949=CARTESIAN_POINT('Ctrl Pts',(13.2890032136005,-2.5550314645236,2.94758481566998));
#80950=CARTESIAN_POINT('Ctrl Pts',(13.2096054553147,-2.50004093914038,2.94259947692984));
#80951=CARTESIAN_POINT('Ctrl Pts',(13.1329398021085,-2.44141116312865,2.9376141381897));
#80952=CARTESIAN_POINT('Ctrl Pts',(13.0563017766302,-2.38280251532021,2.9326305959983));
#80953=CARTESIAN_POINT('Ctrl Pts',(12.9823942480704,-2.32055748890506,2.92764705380689));
#80954=CARTESIAN_POINT('Ctrl Pts',(12.9115730699147,-2.25496678638391,2.92266351161549));
#80955=CARTESIAN_POINT('Ctrl Pts',(12.8407581107952,-2.189381843594,2.91768040704502));
#80956=CARTESIAN_POINT('Ctrl Pts',(12.7730292849172,-2.12045210706759,2.91269730247454));
#80957=CARTESIAN_POINT('Ctrl Pts',(12.7087072797838,-2.04850675378045,2.90771419790406));
#80958=CARTESIAN_POINT('Ctrl Pts',(12.6443733920732,-1.97654810961079,2.90273017277576));
#80959=CARTESIAN_POINT('Ctrl Pts',(12.5834478673824,-1.90157306932208,2.89774614764746));
#80960=CARTESIAN_POINT('Ctrl Pts',(12.5262119131704,-1.82394483235097,2.89276212251917));
#80961=CARTESIAN_POINT('Ctrl Pts',(12.4689144764028,-1.74623320754331,2.88777274357776));
#80962=CARTESIAN_POINT('Ctrl Pts',(12.4153147830547,-1.66586304998148,2.88278336463635));
#80963=CARTESIAN_POINT('Ctrl Pts',(12.3656512492023,-1.58322737128015,2.87779398569494));
#80964=CARTESIAN_POINT('Ctrl Pts',(12.3159582774265,-1.50054271050704,2.87280164931286));
#80965=CARTESIAN_POINT('Ctrl Pts',(12.2702063187608,-1.41559024069342,2.86780931293078));
#80966=CARTESIAN_POINT('Ctrl Pts',(12.2285872744958,-1.3287865723709,2.86281697654869));
#80967=CARTESIAN_POINT('Ctrl Pts',(12.1869016074819,-1.24184395085775,2.85781664855655));
#80968=CARTESIAN_POINT('Ctrl Pts',(12.1493622354496,-1.15304461762709,2.85281632056441));
#80969=CARTESIAN_POINT('Ctrl Pts',(12.1161124565978,-1.06282401507016,2.84781599257226));
#80970=CARTESIAN_POINT('Ctrl Pts',(12.0976725244638,-1.01278874128219,2.84504287010327));
#80971=CARTESIAN_POINT('Ctrl Pts',(12.080551041576,-0.962316593232633,2.84226974763428));
#80972=CARTESIAN_POINT('Ctrl Pts',(12.0647657044095,-0.911483340489195,
2.83949662516529));
#80973=CARTESIAN_POINT('Ctrl Pts',(12.0303090566219,-0.800523183781246,
2.83344338074116));
#80974=CARTESIAN_POINT('Ctrl Pts',(12.0021241467251,-0.687529803949023,
2.82739013631703));
#80975=CARTESIAN_POINT('Ctrl Pts',(11.9804132908884,-0.573147761189416,
2.8213368918929));
#80976=CARTESIAN_POINT('Ctrl Pts',(11.9589656931388,-0.460152674246049,
2.81535704694966));
#80977=CARTESIAN_POINT('Ctrl Pts',(11.9438361316593,-0.345802413645502,
2.80937720200641));
#80978=CARTESIAN_POINT('Ctrl Pts',(11.9351734469449,-0.230738921052811,
2.80339735706317));
#80979=CARTESIAN_POINT('Ctrl Pts',(11.9294653892418,-0.15492073340149,2.79945708899189));
#80980=CARTESIAN_POINT('Ctrl Pts',(11.9265641950853,-0.0787932931996348,
2.79551682092061));
#80981=CARTESIAN_POINT('Ctrl Pts',(11.9265010538313,-0.00254517192389286,
2.79157655284934));
#80982=CARTESIAN_POINT('Origin',(15.,0.,8.20842344717745));
#80983=CARTESIAN_POINT('',(16.8744034286678,2.4401532777456,4.43742370379915));
#80984=CARTESIAN_POINT('',(16.8723108164276,2.43738680900022,4.35414769597494));
#80985=CARTESIAN_POINT('',(16.8723108164276,2.43738680900022,8.20842344717745));
#80986=CARTESIAN_POINT('',(11.926500046528,0.00053479698373032,3.70842344715139));
#80987=CARTESIAN_POINT('Ctrl Pts',(16.8723108164276,2.43738680900022,4.35414769597494));
#80988=CARTESIAN_POINT('Ctrl Pts',(16.9488483750057,2.37859347416326,4.34916459568889));
#80989=CARTESIAN_POINT('Ctrl Pts',(17.022627942246,2.31618088767149,4.34418149540283));
#80990=CARTESIAN_POINT('Ctrl Pts',(17.0932982724848,2.25044542089165,4.33919839511677));
#80991=CARTESIAN_POINT('Ctrl Pts',(17.1639761185111,2.18470296314693,4.33421476487815));
#80992=CARTESIAN_POINT('Ctrl Pts',(17.231543749874,2.11563722236728,4.32923113463953));
#80993=CARTESIAN_POINT('Ctrl Pts',(17.295685840847,2.04358233749817,4.32424750440091));
#80994=CARTESIAN_POINT('Ctrl Pts',(17.3598940064996,1.97145322674465,4.31925874037626));
#80995=CARTESIAN_POINT('Ctrl Pts',(17.420669291915,1.89632915049203,4.3142699763516));
#80996=CARTESIAN_POINT('Ctrl Pts',(17.4777359811466,1.81857819676022,4.30928121232694));
#80997=CARTESIAN_POINT('Ctrl Pts',(17.5348324844232,1.74078662265126,4.30428984196157));
#80998=CARTESIAN_POINT('Ctrl Pts',(17.5882162894751,1.66036580309245,4.2992984715962));
#80999=CARTESIAN_POINT('Ctrl Pts',(17.6376556431944,1.57771193756179,4.29430710123082));
#81000=CARTESIAN_POINT('Ctrl Pts',(17.687178382336,1.4949186663356,4.28930731231838));
#81001=CARTESIAN_POINT('Ctrl Pts',(17.7327431714415,1.40988521179885,4.28430752340594));
#81002=CARTESIAN_POINT('Ctrl Pts',(17.7741646975999,1.32303154935572,4.2793077344935));
#81003=CARTESIAN_POINT('Ctrl Pts',(17.809038064846,1.24990822561668,4.27509834167129));
#81004=CARTESIAN_POINT('Ctrl Pts',(17.8409753984857,1.17549521079981,4.27088894884907));
#81005=CARTESIAN_POINT('Ctrl Pts',(17.8698934162568,1.1000518302907,4.26667955602686));
#81006=CARTESIAN_POINT('Ctrl Pts',(17.9042487347892,1.01042323302418,4.26167869350647));
#81007=CARTESIAN_POINT('Ctrl Pts',(17.9344612304041,0.919027319678192,4.25667783098609));
#81008=CARTESIAN_POINT('Ctrl Pts',(17.9603478056003,0.826282711835128,4.25167696846571));
#81009=CARTESIAN_POINT('Ctrl Pts',(17.9861994180126,0.733663366204382,4.24668286018277));
#81010=CARTESIAN_POINT('Ctrl Pts',(18.007736605184,0.639699365344247,4.24168875189983));
#81011=CARTESIAN_POINT('Ctrl Pts',(18.0248246780298,0.544828337352284,4.23669464361689));
#81012=CARTESIAN_POINT('Ctrl Pts',(18.0418948154112,0.450056885008856,4.23170577709828));
#81013=CARTESIAN_POINT('Ctrl Pts',(18.054525044472,0.35438072756338,4.22671691057968));
#81014=CARTESIAN_POINT('Ctrl Pts',(18.0626310335647,0.258250657784551,4.22172804406108));
#81015=CARTESIAN_POINT('Ctrl Pts',(18.0707312669298,0.162188845993797,4.21674271993032));
#81016=CARTESIAN_POINT('Ctrl Pts',(18.0743136099195,0.065674198492784,4.21175739579957));
#81017=CARTESIAN_POINT('Ctrl Pts',(18.0733453163882,-0.0308353082480665,
4.20677207166882));
#81018=CARTESIAN_POINT('Ctrl Pts',(18.0723773718256,-0.12731003339422,4.20178854422659));
#81019=CARTESIAN_POINT('Ctrl Pts',(18.0668620537893,-0.223779183249446,
4.19680501678437));
#81020=CARTESIAN_POINT('Ctrl Pts',(18.0568187148435,-0.319783668411212,
4.19182148934214));
#81021=CARTESIAN_POINT('Ctrl Pts',(18.0467762580836,-0.415779720739623,
4.18683839964255));
#81022=CARTESIAN_POINT('Ctrl Pts',(18.0322066170607,-0.511310753255124,
4.18185530994296));
#81023=CARTESIAN_POINT('Ctrl Pts',(18.013181020168,-0.605922758855491,4.17687222024337));
#81024=CARTESIAN_POINT('Ctrl Pts',(17.9941519089521,-0.700552240763099,
4.17188821008969));
#81025=CARTESIAN_POINT('Ctrl Pts',(17.9706652937107,-0.794261928563089,
4.16690419993602));
#81026=CARTESIAN_POINT('Ctrl Pts',(17.9428433014491,-0.88660901930666,4.16192018978235));
#81027=CARTESIAN_POINT('Ctrl Pts',(17.9149914232404,-0.97905530784485,4.15693082588325));
#81028=CARTESIAN_POINT('Ctrl Pts',(17.8827949977367,-1.07013565659585,4.15194146198414));
#81029=CARTESIAN_POINT('Ctrl Pts',(17.8464256657073,-1.15942364112636,4.14695209808503));
#81030=CARTESIAN_POINT('Ctrl Pts',(17.8100347762303,-1.24876454994617,4.14195977680549));
#81031=CARTESIAN_POINT('Ctrl Pts',(17.7694662395117,-1.33631058130578,4.13696745552595));
#81032=CARTESIAN_POINT('Ctrl Pts',(17.7249384690705,-1.42165839419308,4.13197513424641));
#81033=CARTESIAN_POINT('Ctrl Pts',(17.6803394189777,-1.50714283108624,4.12697482130418));
#81034=CARTESIAN_POINT('Ctrl Pts',(17.6317687010872,-1.59042164471374,4.12197450836195));
#81035=CARTESIAN_POINT('Ctrl Pts',(17.579488938003,-1.67111910668276,4.11697419541973));
#81036=CARTESIAN_POINT('Ctrl Pts',(17.5504935795652,-1.71587546548723,4.11420092604153));
#81037=CARTESIAN_POINT('Ctrl Pts',(17.5203580550293,-1.75983835100493,4.11142765666333));
#81038=CARTESIAN_POINT('Ctrl Pts',(17.4891324099213,-1.80294816782937,4.10865438728513));
#81039=CARTESIAN_POINT('Ctrl Pts',(17.4328249414843,-1.88068570189063,4.10365350491937));
#81040=CARTESIAN_POINT('Ctrl Pts',(17.3727740527321,-1.95591853085914,4.0986526225536));
#81041=CARTESIAN_POINT('Ctrl Pts',(17.3092303728174,-2.02826461174513,4.09365174018784));
#81042=CARTESIAN_POINT('Ctrl Pts',(17.2457725119616,-2.10051298546995,4.08865761177492));
#81043=CARTESIAN_POINT('Ctrl Pts',(17.1788315222906,-2.16988203288277,4.08366348336201));
#81044=CARTESIAN_POINT('Ctrl Pts',(17.1087003964975,-2.23601987643477,4.0786693549491));
#81045=CARTESIAN_POINT('Ctrl Pts',(17.0386428757322,-2.30208830604593,4.07368046804567));
#81046=CARTESIAN_POINT('Ctrl Pts',(16.9654021923812,-2.36493197416687,4.06869158114224));
#81047=CARTESIAN_POINT('Ctrl Pts',(16.8893098741311,-2.42423399231814,4.06370269423881));
#81048=CARTESIAN_POINT('Ctrl Pts',(16.8132715811698,-2.48349390623696,4.05871734942822));
#81049=CARTESIAN_POINT('Ctrl Pts',(16.7343860233073,-2.53921690019619,4.05373200461763));
#81050=CARTESIAN_POINT('Ctrl Pts',(16.6530189243427,-2.59112537052238,4.04874665980704));
#81051=CARTESIAN_POINT('Ctrl Pts',(16.5716811467436,-2.64301513516479,4.04376311151025));
#81052=CARTESIAN_POINT('Ctrl Pts',(16.487863974313,-2.69109287173475,4.03877956321347));
#81053=CARTESIAN_POINT('Ctrl Pts',(16.4019625223432,-2.73512400741631,4.03379601491669));
#81054=CARTESIAN_POINT('Ctrl Pts',(16.3160686131762,-2.77915127682831,4.02881290421346));
#81055=CARTESIAN_POINT('Ctrl Pts',(16.2280911788234,-2.81913245191646,4.02382979351022));
#81056=CARTESIAN_POINT('Ctrl Pts',(16.1384494151317,-2.85487918819455,4.01884668280699));
#81057=CARTESIAN_POINT('Ctrl Pts',(16.048791091061,-2.89063252830858,4.01386265152614));
#81058=CARTESIAN_POINT('Ctrl Pts',(15.957468234481,-2.92214971355348,4.00887862024528));
#81059=CARTESIAN_POINT('Ctrl Pts',(15.8649184602626,-2.9492911533277,4.00389458896443));
#81060=CARTESIAN_POINT('Ctrl Pts',(15.7722692698296,-2.97646174821571,3.99890520387772));
#81061=CARTESIAN_POINT('Ctrl Pts',(15.6783909522895,-2.99924709033049,3.99391581879102));
#81062=CARTESIAN_POINT('Ctrl Pts',(15.5837344509653,-3.01755800950972,3.98892643370431));
#81063=CARTESIAN_POINT('Ctrl Pts',(15.4890218422372,-3.03587978244039,3.9839340911721));
#81064=CARTESIAN_POINT('Ctrl Pts',(15.3935305651652,-3.04972178852117,3.97894174863989));
#81065=CARTESIAN_POINT('Ctrl Pts',(15.2977177781436,-3.05904664472074,3.97394940610768));
#81066=CARTESIAN_POINT('Ctrl Pts',(15.2017516175532,-3.06838642780554,3.96894907201803));
#81067=CARTESIAN_POINT('Ctrl Pts',(15.1054633571565,-3.0731946012312,3.96394873792838));
#81068=CARTESIAN_POINT('Ctrl Pts',(15.0093111762828,-3.0734858958512,3.95894840383872));
#81069=CARTESIAN_POINT('Ctrl Pts',(14.9559875519744,-3.07364744065173,3.95617534207361));
#81070=CARTESIAN_POINT('Ctrl Pts',(14.90270572017,-3.07242073058102,3.9534022803085));
#81071=CARTESIAN_POINT('Ctrl Pts',(14.8495429190397,-3.06981512746108,3.95062921854339));
#81072=CARTESIAN_POINT('Ctrl Pts',(14.7536703234448,-3.06511624160693,3.94562834154831));
#81073=CARTESIAN_POINT('Ctrl Pts',(14.6578508137849,-3.05591359805995,3.94062746455323));
#81074=CARTESIAN_POINT('Ctrl Pts',(14.5625413030582,-3.04220843113518,3.93562658755814));
#81075=CARTESIAN_POINT('Ctrl Pts',(14.4673605136946,-3.02852177388226,3.93063246455538));
#81076=CARTESIAN_POINT('Ctrl Pts',(14.3726887848571,-3.01034474086119,3.92563834155262));
#81077=CARTESIAN_POINT('Ctrl Pts',(14.2789809042196,-2.98773052893329,3.92064421854986));
#81078=CARTESIAN_POINT('Ctrl Pts',(14.1853713739254,-2.96514005156742,3.91565533708824));
#81079=CARTESIAN_POINT('Ctrl Pts',(14.0927241049829,-2.9381217556984,3.91066645562662));
#81080=CARTESIAN_POINT('Ctrl Pts',(14.0014856279963,-2.90678022886182,3.90567757416501));
#81081=CARTESIAN_POINT('Ctrl Pts',(13.9103119305315,-2.87546095457913,3.90069223482034));
#81082=CARTESIAN_POINT('Ctrl Pts',(13.8205454502547,-2.8398246935631,3.89570689547568));
#81083=CARTESIAN_POINT('Ctrl Pts',(13.7326184923474,-2.80002613631733,3.89072155613101));
#81084=CARTESIAN_POINT('Ctrl Pts',(13.6447232199693,-2.76024192095689,3.88573801331291));
#81085=CARTESIAN_POINT('Ctrl Pts',(13.5586665520638,-2.71629857036273,3.88075447049481));
#81086=CARTESIAN_POINT('Ctrl Pts',(13.4748608060477,-2.66839889991558,3.8757709276767));
#81087=CARTESIAN_POINT('Ctrl Pts',(13.3910624189226,-2.62050343548613,3.87078782245805));
#81088=CARTESIAN_POINT('Ctrl Pts',(13.3095149414523,-2.56865255978706,3.8658047172394));
#81089=CARTESIAN_POINT('Ctrl Pts',(13.2306051238602,-2.51309451121327,3.86082161202074));
#81090=CARTESIAN_POINT('Ctrl Pts',(13.1516807284728,-2.45752619884866,3.8558375862235));
#81091=CARTESIAN_POINT('Ctrl Pts',(13.0753953193757,-2.39824960601306,3.85085356042627));
#81092=CARTESIAN_POINT('Ctrl Pts',(13.0021048714653,-2.33555503154548,3.84586953462903));
#81093=CARTESIAN_POINT('Ctrl Pts',(12.9287356949499,-2.27279311056099,3.84088015499089));
#81094=CARTESIAN_POINT('Ctrl Pts',(12.8583682361594,-2.20660616374052,3.83589077535274));
#81095=CARTESIAN_POINT('Ctrl Pts',(12.7913235179395,-2.1373231968032,3.83090139571459));
#81096=CARTESIAN_POINT('Ctrl Pts',(12.7242390589276,-2.06799916235066,3.82590905861903));
#81097=CARTESIAN_POINT('Ctrl Pts',(12.6604815519403,-1.99557578271777,3.82091672152347));
#81098=CARTESIAN_POINT('Ctrl Pts',(12.6003320372269,-1.9204155587894,3.81592438442791));
#81099=CARTESIAN_POINT('Ctrl Pts',(12.5400862364191,-1.845135019935,3.81092405570278));
#81100=CARTESIAN_POINT('Ctrl Pts',(12.4834602174762,-1.76710924381181,3.80592372697764));
#81101=CARTESIAN_POINT('Ctrl Pts',(12.4306919269981,-1.68673005427879,3.80092339825251));
#81102=CARTESIAN_POINT('Ctrl Pts',(12.4014273312902,-1.64215281928218,3.79815028210222));
#81103=CARTESIAN_POINT('Ctrl Pts',(12.3733484337038,-1.59685221060393,3.79537716595194));
#81104=CARTESIAN_POINT('Ctrl Pts',(12.3464895869019,-1.55089804229029,3.79260404980166));
#81105=CARTESIAN_POINT('Ctrl Pts',(12.2962687235998,-1.46497261064162,3.78741885744656));
#81106=CARTESIAN_POINT('Ctrl Pts',(12.2501518247339,-1.37648008503504,3.78223366509146));
#81107=CARTESIAN_POINT('Ctrl Pts',(12.2083991234112,-1.28583311352156,3.77704847273635));
#81108=CARTESIAN_POINT('Ctrl Pts',(12.1667175851587,-1.19534064019856,3.77187211799406));
#81109=CARTESIAN_POINT('Ctrl Pts',(12.1293856045808,-1.10270138378311,3.76669576325176));
#81110=CARTESIAN_POINT('Ctrl Pts',(12.0966184712053,-1.00835407881036,3.76151940850946));
#81111=CARTESIAN_POINT('Ctrl Pts',(12.063916973894,-0.914195761555924,3.75635342255801));
#81112=CARTESIAN_POINT('Ctrl Pts',(12.0357622347784,-0.818336582006121,
3.75118743660656));
#81113=CARTESIAN_POINT('Ctrl Pts',(12.0123217486003,-0.721235686938343,
3.7460214506551));
#81114=CARTESIAN_POINT('Ctrl Pts',(11.9889093155104,-0.624251000209755,
3.74086164724859));
#81115=CARTESIAN_POINT('Ctrl Pts',(11.970200001538,-0.526027935410458,3.73570184384208));
#81116=CARTESIAN_POINT('Ctrl Pts',(11.9563118270862,-0.427041632706651,
3.73054204043557));
#81117=CARTESIAN_POINT('Ctrl Pts',(11.9424418566281,-0.328185076790691,
3.725389000267));
#81118=CARTESIAN_POINT('Ctrl Pts',(11.9333804921489,-0.228567664282163,
3.72023596009843));
#81119=CARTESIAN_POINT('Ctrl Pts',(11.9291947176724,-0.128674659621159,
3.71508291992986));
#81120=CARTESIAN_POINT('Ctrl Pts',(11.9273915716872,-0.0856427974625278,
3.71286309567906));
#81121=CARTESIAN_POINT('Ctrl Pts',(11.926492547944,-0.0425599106124228,
3.71064327142826));
#81122=CARTESIAN_POINT('Ctrl Pts',(11.9265000465279,0.000534796477657107,
3.70842344717746));
#81123=CARTESIAN_POINT('Ctrl Pts',(11.926500046528,0.000534796983736532,
3.70842344715139));
#81124=CARTESIAN_POINT('Ctrl Pts',(11.9265179259855,0.103288763884867,3.70313055243193));
#81125=CARTESIAN_POINT('Ctrl Pts',(11.9316930045359,0.205917075552153,3.69783765771246));
#81126=CARTESIAN_POINT('Ctrl Pts',(11.9419621490322,0.307907050987914,3.69254476299299));
#81127=CARTESIAN_POINT('Ctrl Pts',(11.9522653070746,0.410234838471516,3.68723433710346));
#81128=CARTESIAN_POINT('Ctrl Pts',(11.9676962419627,0.511919711507636,3.68192391121393));
#81129=CARTESIAN_POINT('Ctrl Pts',(11.9881402471583,0.612456593737547,3.6766134853244));
#81130=CARTESIAN_POINT('Ctrl Pts',(12.0086191925345,0.713165300264503,3.67129398355968));
#81131=CARTESIAN_POINT('Ctrl Pts',(12.034128220555,0.812721762062335,3.66597448179496));
#81132=CARTESIAN_POINT('Ctrl Pts',(12.0645027368102,0.910636078686353,3.66065498003023));
#81133=CARTESIAN_POINT('Ctrl Pts',(12.0949645851663,1.0088319162704,3.65532018375807));
#81134=CARTESIAN_POINT('Ctrl Pts',(12.1303197790766,1.1053758367413,3.64998538748591));
#81135=CARTESIAN_POINT('Ctrl Pts',(12.1703549949709,1.19979639752506,3.64465059121375));
#81136=CARTESIAN_POINT('Ctrl Pts',(12.1955495272369,1.25921613117943,3.64129335449581));
#81137=CARTESIAN_POINT('Ctrl Pts',(12.2225965524397,1.31779542095264,3.63793611777786));
#81138=CARTESIAN_POINT('Ctrl Pts',(12.2514338177412,1.3754221867278,3.63457888105992));
#81139=CARTESIAN_POINT('Ctrl Pts',(12.2943892720977,1.46126194584123,3.62957800365029));
#81140=CARTESIAN_POINT('Ctrl Pts',(12.3414447733354,1.54523722853729,3.62457712624066));
#81141=CARTESIAN_POINT('Ctrl Pts',(12.3924149664827,1.62693040508086,3.61957624883103));
#81142=CARTESIAN_POINT('Ctrl Pts',(12.4433163211217,1.70851324976051,3.61458212542644));
#81143=CARTESIAN_POINT('Ctrl Pts',(12.4981216295677,1.78781974491484,3.60958800202185));
#81144=CARTESIAN_POINT('Ctrl Pts',(12.5565988421315,1.86445515680238,3.60459387861725));
#81145=CARTESIAN_POINT('Ctrl Pts',(12.6150146802628,1.94101013642041,3.59960499676705));
#81146=CARTESIAN_POINT('Ctrl Pts',(12.677094496469,2.01489925900873,3.59461611491685));
#81147=CARTESIAN_POINT('Ctrl Pts',(12.7425625419643,2.08575606748667,3.58962723306665));
#81148=CARTESIAN_POINT('Ctrl Pts',(12.8079841047226,2.15656256717085,3.58464189335493));
#81149=CARTESIAN_POINT('Ctrl Pts',(12.8767888174963,2.22434071151225,3.57965655364321));
#81150=CARTESIAN_POINT('Ctrl Pts',(12.948660817216,2.2887572626155,3.57467121393149));
#81151=CARTESIAN_POINT('Ctrl Pts',(13.0205069168094,2.35315060027235,3.56968767075985));
#81152=CARTESIAN_POINT('Ctrl Pts',(13.0954177807538,2.41418445918998,3.56470412758821));
#81153=CARTESIAN_POINT('Ctrl Pts',(13.1730415652243,2.47156329629689,3.55972058441658));
#81154=CARTESIAN_POINT('Ctrl Pts',(13.2506585334171,2.52893709486964,3.55473747885842));
#81155=CARTESIAN_POINT('Ctrl Pts',(13.3309875955968,2.58265624918541,3.54975437330026));
#81156=CARTESIAN_POINT('Ctrl Pts',(13.4136456492958,2.63246692742794,3.54477126774211));
#81157=CARTESIAN_POINT('Ctrl Pts',(13.4963189729971,2.68228680754659,3.53978724161989));
#81158=CARTESIAN_POINT('Ctrl Pts',(13.5813217669772,2.72819655121854,3.53480321549767));
#81159=CARTESIAN_POINT('Ctrl Pts',(13.668244847156,2.76998744814366,3.52981918937546));
#81160=CARTESIAN_POINT('Ctrl Pts',(13.7552612996843,2.81182323664675,3.52482980943666));
#81161=CARTESIAN_POINT('Ctrl Pts',(13.8442017604325,2.84953115524765,3.51984042949785));
#81162=CARTESIAN_POINT('Ctrl Pts',(13.9346357166394,2.88295008519736,3.51485104955905));
#81163=CARTESIAN_POINT('Ctrl Pts',(14.0251232773767,2.916388824145,3.50985871217615));
#81164=CARTESIAN_POINT('Ctrl Pts',(14.1171056783353,2.94553337985266,3.50486637479326));
#81165=CARTESIAN_POINT('Ctrl Pts',(14.2101378756744,2.97027272730231,3.49987403741037));
#81166=CARTESIAN_POINT('Ctrl Pts',(14.3033189965691,2.99505167686489,3.49487370842182));
#81167=CARTESIAN_POINT('Ctrl Pts',(14.3975528408454,3.01541124538148,3.48987337943328));
#81168=CARTESIAN_POINT('Ctrl Pts',(14.4923849059777,3.03129166632324,3.48487305044474));
#81169=CARTESIAN_POINT('Ctrl Pts',(14.5449774465139,3.04009872626596,3.48209993773589));
#81170=CARTESIAN_POINT('Ctrl Pts',(14.5977538872124,3.04752907963788,3.47932682502704));
#81171=CARTESIAN_POINT('Ctrl Pts',(14.6506364897203,3.05357943857451,3.47655371231819));
#81172=CARTESIAN_POINT('Ctrl Pts',(14.7478038738911,3.06469646994753,3.47145834833928));
#81173=CARTESIAN_POINT('Ctrl Pts',(14.8456751428802,3.07119073221958,3.46636298436037));
#81174=CARTESIAN_POINT('Ctrl Pts',(14.9437730708905,3.07298564631254,3.46126762038146));
#81175=CARTESIAN_POINT('Ctrl Pts',(15.0399040776467,3.07474457132041,3.45627442145242));
#81176=CARTESIAN_POINT('Ctrl Pts',(15.1362522756829,3.07199079458058,3.45128122252339));
#81177=CARTESIAN_POINT('Ctrl Pts',(15.232360432918,3.06470404431066,3.44628802359435));
#81178=CARTESIAN_POINT('Ctrl Pts',(15.3283766492337,3.05742426483843,3.44129960135975));
#81179=CARTESIAN_POINT('Ctrl Pts',(15.4241528461465,3.04562016087953,3.43631117912515));
#81180=CARTESIAN_POINT('Ctrl Pts',(15.5192316013898,3.02932348786295,3.43132275689055));
#81181=CARTESIAN_POINT('Ctrl Pts',(15.6142453186025,3.01303796248409,3.42633774695513));
#81182=CARTESIAN_POINT('Ctrl Pts',(15.7085621113835,2.99226605011536,3.4213527370197));
#81183=CARTESIAN_POINT('Ctrl Pts',(15.8017305545386,2.96709123013083,3.41636772708428));
#81184=CARTESIAN_POINT('Ctrl Pts',(15.8984541423936,2.94095578308408,3.41119249789595));
#81185=CARTESIAN_POINT('Ctrl Pts',(15.9939394997286,2.91007475332913,3.40601726870763));
#81186=CARTESIAN_POINT('Ctrl Pts',(16.0876947952964,2.87459949945817,3.4008420395193));
#81187=CARTESIAN_POINT('Ctrl Pts',(16.1779764290032,2.84043861439844,3.39585855412683));
#81188=CARTESIAN_POINT('Ctrl Pts',(16.2666535061744,2.80201811261858,3.39087506873436));
#81189=CARTESIAN_POINT('Ctrl Pts',(16.3533052419485,2.75952299720708,3.38589158334189));
#81190=CARTESIAN_POINT('Ctrl Pts',(16.4399652523917,2.71702382379239,3.38090762205943));
#81191=CARTESIAN_POINT('Ctrl Pts',(16.5245991469185,2.67044946398176,3.37592366077698));
#81192=CARTESIAN_POINT('Ctrl Pts',(16.606810133319,2.62003119169666,3.37093969949453));
#81193=CARTESIAN_POINT('Ctrl Pts',(16.6890743805132,2.56958025568474,3.36595250932813));
#81194=CARTESIAN_POINT('Ctrl Pts',(16.768912220232,2.51528067766863,3.36096531916174));
#81195=CARTESIAN_POINT('Ctrl Pts',(16.8459558454969,2.45740702092184,3.35597812899535));
#81196=CARTESIAN_POINT('Ctrl Pts',(16.8547776101565,2.45078028473102,3.35540707827169));
#81197=CARTESIAN_POINT('Ctrl Pts',(16.8635627751665,2.44410673224555,3.35483602754802));
#81198=CARTESIAN_POINT('Ctrl Pts',(16.8723108164276,2.43738680900022,3.35426497682436));
#81199=CARTESIAN_POINT('',(11.9260286661608,0.000457056471357439,3.79157660457388));
#81200=CARTESIAN_POINT('Ctrl Pts',(11.9265000341218,0.000457981234923757,
3.79157655282255));
#81201=CARTESIAN_POINT('Ctrl Pts',(11.9265037802304,0.0255980166936363,
3.79026691442027));
#81202=CARTESIAN_POINT('Ctrl Pts',(11.9268159741402,0.0507354235207862,
3.78895727601798));
#81203=CARTESIAN_POINT('Ctrl Pts',(11.9274364573799,0.0758651867586845,
3.7876476376157));
#81204=CARTESIAN_POINT('Ctrl Pts',(11.9298057860042,0.171823729304893,3.7826467551499));
#81205=CARTESIAN_POINT('Ctrl Pts',(11.936678843721,0.267838568083366,3.7776458726841));
#81206=CARTESIAN_POINT('Ctrl Pts',(11.9480654915482,0.363452893950377,3.77264499021831));
#81207=CARTESIAN_POINT('Ctrl Pts',(11.9594367611156,0.458938087700323,3.76765086170423));
#81208=CARTESIAN_POINT('Ctrl Pts',(11.9753094540373,0.554023411679852,3.76265673319015));
#81209=CARTESIAN_POINT('Ctrl Pts',(11.995641432497,0.648252919678345,3.75766260467606));
#81210=CARTESIAN_POINT('Ctrl Pts',(12.0159520718507,0.742383530588454,3.7526737176705));
#81211=CARTESIAN_POINT('Ctrl Pts',(12.040712600613,0.835659684587091,3.74768483066494));
#81212=CARTESIAN_POINT('Ctrl Pts',(12.0698293049436,0.927632442205818,3.74269594365938));
#81213=CARTESIAN_POINT('Ctrl Pts',(12.0989253365193,1.01953989949872,3.73771059874558));
#81214=CARTESIAN_POINT('Ctrl Pts',(12.1323712630674,1.11014538307368,3.73272525383178));
#81215=CARTESIAN_POINT('Ctrl Pts',(12.1700229371203,1.19901295805135,3.72773990891797));
#81216=CARTESIAN_POINT('Ctrl Pts',(12.207661043059,1.28784850881123,3.72275636051737));
#81217=CARTESIAN_POINT('Ctrl Pts',(12.2495017141688,1.37494699183315,3.71777281211677));
#81218=CARTESIAN_POINT('Ctrl Pts',(12.2953522069319,1.45989128549082,3.71278926371617));
#81219=CARTESIAN_POINT('Ctrl Pts',(12.3411986736766,1.54482812039991,3.70780615290864));
#81220=CARTESIAN_POINT('Ctrl Pts',(12.3910540534722,1.62761075610814,3.70282304210111));
#81221=CARTESIAN_POINT('Ctrl Pts',(12.4446795723252,1.70784652762125,3.69783993129358));
#81222=CARTESIAN_POINT('Ctrl Pts',(12.4983149979361,1.78809712186014,3.69285589990806));
#81223=CARTESIAN_POINT('Ctrl Pts',(12.5557217020849,1.86579955277997,3.68787186852255));
#81224=CARTESIAN_POINT('Ctrl Pts',(12.6166181154014,1.94059090025874,3.68288783713703));
#81225=CARTESIAN_POINT('Ctrl Pts',(12.677579943147,2.01546258799133,3.67789845194576));
#81226=CARTESIAN_POINT('Ctrl Pts',(12.7420386862182,2.08741660883097,3.67290906675449));
#81227=CARTESIAN_POINT('Ctrl Pts',(12.8096732310118,2.15612404444959,3.66791968156322));
#81228=CARTESIAN_POINT('Ctrl Pts',(12.8773478660129,2.22487220622907,3.66292733892634));
#81229=CARTESIAN_POINT('Ctrl Pts',(12.9482017290782,2.2903696533319,3.65793499628946));
#81230=CARTESIAN_POINT('Ctrl Pts',(13.0218792503718,2.35232662483132,3.65294265365258));
#81231=CARTESIAN_POINT('Ctrl Pts',(13.0956747119036,2.4143827747484,3.64794231945912));
#81232=CARTESIAN_POINT('Ctrl Pts',(13.1723025083832,2.47288686685116,3.64294198526566));
#81233=CARTESIAN_POINT('Ctrl Pts',(13.251376709153,2.52759150906694,3.6379416510722));
#81234=CARTESIAN_POINT('Ctrl Pts',(13.2952292903294,2.55792934037148,3.63516859033945));
#81235=CARTESIAN_POINT('Ctrl Pts',(13.3398337948282,2.58709943598804,3.63239552960671));
#81236=CARTESIAN_POINT('Ctrl Pts',(13.3851212676778,2.61506576014706,3.62962246887396));
#81237=CARTESIAN_POINT('Ctrl Pts',(13.4667917043678,2.66549961664126,3.6246215918817));
#81238=CARTESIAN_POINT('Ctrl Pts',(13.5509695081239,2.71219184757326,3.61962071488944));
#81239=CARTESIAN_POINT('Ctrl Pts',(13.6372774368868,2.75488465565842,3.61461983789718));
#81240=CARTESIAN_POINT('Ctrl Pts',(13.7234688014811,2.79751980447922,3.60962571489701));
#81241=CARTESIAN_POINT('Ctrl Pts',(13.8117841835152,2.83616607287433,3.60463159189685));
#81242=CARTESIAN_POINT('Ctrl Pts',(13.901818658671,2.87060968986674,3.59963746889669));
#81243=CARTESIAN_POINT('Ctrl Pts',(13.9917586388803,2.90501715684283,3.59464858743745));
#81244=CARTESIAN_POINT('Ctrl Pts',(14.0834137178149,2.93523058519941,3.58965970597821));
#81245=CARTESIAN_POINT('Ctrl Pts',(14.1763566660133,2.96108323226133,3.58467082451897));
#81246=CARTESIAN_POINT('Ctrl Pts',(14.2692336245182,2.98691752388817,3.57968548517631));
#81247=CARTESIAN_POINT('Ctrl Pts',(14.3633962130629,3.0083970721192,3.57470014583365));
#81248=CARTESIAN_POINT('Ctrl Pts',(14.4584005449834,3.02540448210247,3.56971480649099));
#81249=CARTESIAN_POINT('Ctrl Pts',(14.5533706409624,3.04240576326319,3.56473126367468));
#81250=CARTESIAN_POINT('Ctrl Pts',(14.6491814462386,3.05493803109365,3.55974772085837));
#81251=CARTESIAN_POINT('Ctrl Pts',(14.7453782861762,3.06293487244659,3.55476417804206));
#81252=CARTESIAN_POINT('Ctrl Pts',(14.8415666791784,3.07093101160597,3.54978107282498));
#81253=CARTESIAN_POINT('Ctrl Pts',(14.9381406022654,3.07439247998299,3.54479796760791));
#81254=CARTESIAN_POINT('Ctrl Pts',(15.0346407212946,3.07330477994425,3.53981486239083));
#81255=CARTESIAN_POINT('Ctrl Pts',(15.131158667755,3.07221687896382,3.53483083659494));
#81256=CARTESIAN_POINT('Ctrl Pts',(15.2276023444474,3.06657814546016,3.52984681079905));
#81257=CARTESIAN_POINT('Ctrl Pts',(15.3235139544554,3.05642617631648,3.52486278500316));
#81258=CARTESIAN_POINT('Ctrl Pts',(15.4195285927294,3.04626330192602,3.519873405366));
#81259=CARTESIAN_POINT('Ctrl Pts',(15.515009586372,3.03157755956898,3.51488402572885));
#81260=CARTESIAN_POINT('Ctrl Pts',(15.6095060173364,3.01245824283602,3.50989464609169));
#81261=CARTESIAN_POINT('Ctrl Pts',(15.7040584611141,2.99332759311717,3.50490230899691));
#81262=CARTESIAN_POINT('Ctrl Pts',(15.797624755,2.96975824328842,3.49990997190213));
#81263=CARTESIAN_POINT('Ctrl Pts',(15.8897679576311,2.94188973817392,3.49491763480736));
#81264=CARTESIAN_POINT('Ctrl Pts',(15.9820586611939,2.9139766217332,3.48991730608268));
#81265=CARTESIAN_POINT('Ctrl Pts',(16.0729213118051,2.88175075522685,3.484916977358));
#81266=CARTESIAN_POINT('Ctrl Pts',(16.1619378719125,2.84540025863065,3.47991664863333));
#81267=CARTESIAN_POINT('Ctrl Pts',(16.211305278649,2.82524075405788,3.47714353246629));
#81268=CARTESIAN_POINT('Ctrl Pts',(16.2601052981254,2.80381348718193,3.47437041629926));
#81269=CARTESIAN_POINT('Ctrl Pts',(16.3082700746706,2.78115653312097,3.47159730013223));
#81270=CARTESIAN_POINT('Ctrl Pts',(16.3951353878213,2.74029465124967,3.46659597714205));
#81271=CARTESIAN_POINT('Ctrl Pts',(16.4802360276853,2.69528791493697,3.46159465415187));
#81272=CARTESIAN_POINT('Ctrl Pts',(16.5631498740513,2.64631153140617,3.45659333116168));
#81273=CARTESIAN_POINT('Ctrl Pts',(16.6459414432796,2.5974073757632,3.45159938386913));
#81274=CARTESIAN_POINT('Ctrl Pts',(16.7265522571003,2.54454543504667,3.44660543657658));
#81275=CARTESIAN_POINT('Ctrl Pts',(16.8045821065948,2.48794808437751,3.44161148928402));
#81276=CARTESIAN_POINT('Ctrl Pts',(16.8273817369834,2.47141084017433,3.44015230215002));
#81277=CARTESIAN_POINT('Ctrl Pts',(16.8499611681798,2.45455498600154,3.43869311501603));
#81278=CARTESIAN_POINT('Ctrl Pts',(16.8723108164276,2.43738680900022,3.43723392788203));
#81279=CARTESIAN_POINT('Ctrl Pts',(16.8744034286678,2.4401532777456,4.43742370379915));
#81280=CARTESIAN_POINT('Ctrl Pts',(16.9648833459027,2.37176298119687,4.43153190672698));
#81281=CARTESIAN_POINT('Ctrl Pts',(17.8240291038397,1.64081102949522,4.37296505340756));
#81282=CARTESIAN_POINT('Ctrl Pts',(18.5634164219284,-0.676361122770444,
4.2617231438409));
#81283=CARTESIAN_POINT('Ctrl Pts',(16.3800292810756,-3.35423176516155,4.10369797509917));
#81284=CARTESIAN_POINT('Ctrl Pts',(12.9727817450913,-2.99125903268367,3.94698262306987));
#81285=CARTESIAN_POINT('Ctrl Pts',(11.923704677711,-0.987130664284586,3.84294232728783));
#81286=CARTESIAN_POINT('Ctrl Pts',(11.9216277130479,0.000448422365026861,
3.79157708775303));
#81287=CARTESIAN_POINT('Origin',(15.,0.,8.20842344717745));
#81288=CARTESIAN_POINT('',(16.8723108164276,2.43738680900022,5.43736140735745));
#81289=CARTESIAN_POINT('',(16.8743174193178,2.43995797974749,5.35407234097178));
#81290=CARTESIAN_POINT('',(16.8723108164276,2.43738680900022,8.20842344717745));
#81291=CARTESIAN_POINT('',(11.9269509903871,-0.00352382680246899,5.79157674146509));
#81292=CARTESIAN_POINT('Ctrl Pts',(11.9265020164746,-0.00352069106647204,
5.79157655282255));
#81293=CARTESIAN_POINT('Ctrl Pts',(11.9263925964237,0.0920009834060071,
5.78664484566267));
#81294=CARTESIAN_POINT('Ctrl Pts',(11.9307405367531,0.18759836643084,5.78171313850279));
#81295=CARTESIAN_POINT('Ctrl Pts',(11.9395400315067,0.282819785817695,5.77678143134291));
#81296=CARTESIAN_POINT('Ctrl Pts',(11.948336955793,0.378013389568948,5.77185116481026));
#81297=CARTESIAN_POINT('Ctrl Pts',(11.9615828108053,0.472830801643596,5.76692089827761));
#81298=CARTESIAN_POINT('Ctrl Pts',(11.9792197838843,0.566823725618401,5.76199063174496));
#81299=CARTESIAN_POINT('Ctrl Pts',(11.996856650819,0.660816083917506,5.75706039488403));
#81300=CARTESIAN_POINT('Ctrl Pts',(12.0188844997887,0.753983523412695,5.7521301580231));
#81301=CARTESIAN_POINT('Ctrl Pts',(12.0451942965562,0.845887406748669,5.74719992116217));
#81302=CARTESIAN_POINT('Ctrl Pts',(12.0715114625849,0.937817031967794,5.74226830336306));
#81303=CARTESIAN_POINT('Ctrl Pts',(12.1021128339379,1.02848196754582,5.73733668556395));
#81304=CARTESIAN_POINT('Ctrl Pts',(12.1368397174184,1.11745937118419,5.73240506776485));
#81305=CARTESIAN_POINT('Ctrl Pts',(12.1716074489345,1.2065414358741,5.72746764907379));
#81306=CARTESIAN_POINT('Ctrl Pts',(12.2105102107563,1.29393159048697,5.72253023038273));
#81307=CARTESIAN_POINT('Ctrl Pts',(12.2533415748387,1.37922795269323,5.71759281169167));
#81308=CARTESIAN_POINT('Ctrl Pts',(12.296202926742,1.46458403403517,5.7126519361313));
#81309=CARTESIAN_POINT('Ctrl Pts',(12.3429981327611,1.54784301736527,5.70771106057094));
#81310=CARTESIAN_POINT('Ctrl Pts',(12.3934764629018,1.62863049847199,5.70277018501057));
#81311=CARTESIAN_POINT('Ctrl Pts',(12.444035586198,1.70954728408431,5.69782140132554));
#81312=CARTESIAN_POINT('Ctrl Pts',(12.4982893379946,1.78798431024768,5.69287261764051));
#81313=CARTESIAN_POINT('Ctrl Pts',(12.5559458884148,1.86359913866777,5.68792383395549));
#81314=CARTESIAN_POINT('Ctrl Pts',(12.5713797829185,1.88384022621544,5.6865991101425));
#81315=CARTESIAN_POINT('Ctrl Pts',(12.5870573023478,1.90387928819221,5.68527438632951));
#81316=CARTESIAN_POINT('Ctrl Pts',(12.6029724092414,1.92371021184119,5.68394966251652));
#81317=CARTESIAN_POINT('Ctrl Pts',(12.6631243299309,1.99866215244131,5.67894280442458));
#81318=CARTESIAN_POINT('Ctrl Pts',(12.7268987108395,2.07091920946328,5.67393594633263));
#81319=CARTESIAN_POINT('Ctrl Pts',(12.7940253727926,2.14011172468098,5.66892908824069));
#81320=CARTESIAN_POINT('Ctrl Pts',(12.8610613977209,2.20921081347866,5.6639289906029));
#81321=CARTESIAN_POINT('Ctrl Pts',(12.9314404049951,2.27525327353562,5.65892889296511));
#81322=CARTESIAN_POINT('Ctrl Pts',(13.0048514334962,2.33790171897317,5.65392879532732));
#81323=CARTESIAN_POINT('Ctrl Pts',(13.0781852825972,2.40048430006402,5.64893395445467));
#81324=CARTESIAN_POINT('Ctrl Pts',(13.154544484504,2.45967967806806,5.64393911358203));
#81325=CARTESIAN_POINT('Ctrl Pts',(13.2335813528962,2.51518735150369,5.63894427270938));
#81326=CARTESIAN_POINT('Ctrl Pts',(13.3125613934417,2.57065511468449,5.6339530231487));
#81327=CARTESIAN_POINT('Ctrl Pts',(13.3942149157232,2.62244019424737,5.62896177358803));
#81328=CARTESIAN_POINT('Ctrl Pts',(13.478162050998,2.67028303873904,5.62397052402735));
#81329=CARTESIAN_POINT('Ctrl Pts',(13.5620784131935,2.71810834514986,5.61898110414339));
#81330=CARTESIAN_POINT('Ctrl Pts',(13.6482863379862,2.76199407175551,5.61399168425942));
#81331=CARTESIAN_POINT('Ctrl Pts',(13.7363787410871,2.80172510500643,5.60900226437546));
#81332=CARTESIAN_POINT('Ctrl Pts',(13.8244626942452,2.84145232720278,5.60401332308341));
#81333=CARTESIAN_POINT('Ctrl Pts',(13.9144303674491,2.87702546882009,5.59902438179136));
#81334=CARTESIAN_POINT('Ctrl Pts',(14.0058529089589,2.90827677695479,5.59403544049932));
#81335=CARTESIAN_POINT('Ctrl Pts',(14.0972914245552,2.939533545571,5.58904562749906));
#81336=CARTESIAN_POINT('Ctrl Pts',(14.1901848993957,2.96646683949829,5.58405581449881));
#81337=CARTESIAN_POINT('Ctrl Pts',(14.2840884776609,2.98895850459355,5.57906600149856));
#81338=CARTESIAN_POINT('Ctrl Pts',(14.3780907208969,3.01147380179655,5.57407094567623));
#81339=CARTESIAN_POINT('Ctrl Pts',(14.4731047602957,3.02953805120322,5.56907588985389));
#81340=CARTESIAN_POINT('Ctrl Pts',(14.5686748998234,3.04308411121967,5.56408083403156));
#81341=CARTESIAN_POINT('Ctrl Pts',(14.6643005749494,3.05663804282186,5.55908287559325));
#81342=CARTESIAN_POINT('Ctrl Pts',(14.7604825583859,3.0656685156294,5.55408491715495));
#81343=CARTESIAN_POINT('Ctrl Pts',(14.8567614522654,3.07016041412218,5.54908695871664));
#81344=CARTESIAN_POINT('Ctrl Pts',(14.9531915603744,3.07465936752536,5.54408115055755));
#81345=CARTESIAN_POINT('Ctrl Pts',(15.0497184457063,3.0746055134796,5.53907534239846));
#81346=CARTESIAN_POINT('Ctrl Pts',(15.1458842162635,3.07003583781121,5.53406953423937));
#81347=CARTESIAN_POINT('Ctrl Pts',(15.1980419010702,3.06755737066225,5.53135452075118));
#81348=CARTESIAN_POINT('Ctrl Pts',(15.2500934603555,3.06375139340765,5.52863950726299));
#81349=CARTESIAN_POINT('Ctrl Pts',(15.3019669800779,3.05863011705284,5.5259244937748));
#81350=CARTESIAN_POINT('Ctrl Pts',(15.3976641489927,3.04918229760645,5.52091578980068));
#81351=CARTESIAN_POINT('Ctrl Pts',(15.4930781290478,3.03522313013419,5.51590708582656));
#81352=CARTESIAN_POINT('Ctrl Pts',(15.5877513814294,3.01677817607258,5.51089838185243));
#81353=CARTESIAN_POINT('Ctrl Pts',(15.6823057632538,2.9983563812657,5.50589596674468));
#81354=CARTESIAN_POINT('Ctrl Pts',(15.7761208401512,2.97546007480159,5.50089355163692));
#81355=CARTESIAN_POINT('Ctrl Pts',(15.8687439006586,2.94816659723776,5.49589113652917));
#81356=CARTESIAN_POINT('Ctrl Pts',(15.9612665265484,2.92090271500329,5.49089414572553));
#81357=CARTESIAN_POINT('Ctrl Pts',(16.0525992897885,2.88925126764076,5.48589715492189));
#81358=CARTESIAN_POINT('Ctrl Pts',(16.1423005464758,2.8533404478823,5.48090016411825));
#81359=CARTESIAN_POINT('Ctrl Pts',(16.2319435201223,2.81745296103853,5.47590642008984));
#81360=CARTESIAN_POINT('Ctrl Pts',(16.3199566896999,2.77731176433479,5.47091267606143));
#81361=CARTESIAN_POINT('Ctrl Pts',(16.4059152154471,2.73309433737192,5.46591893203303));
#81362=CARTESIAN_POINT('Ctrl Pts',(16.4918570019696,2.68888552113658,5.46092616046666));
#81363=CARTESIAN_POINT('Ctrl Pts',(16.5757445472854,2.64060224345441,5.45593338890029));
#81364=CARTESIAN_POINT('Ctrl Pts',(16.6571753181588,2.58846908710251,5.45094061733392));
#81365=CARTESIAN_POINT('Ctrl Pts',(16.7309997475721,2.54120562048028,5.44641421400843));
#81366=CARTESIAN_POINT('Ctrl Pts',(16.8028050080403,2.49077861220831,5.44188781068294));
#81367=CARTESIAN_POINT('Ctrl Pts',(16.8723108164276,2.43738680900022,5.43736140735745));
#81368=CARTESIAN_POINT('',(14.2062007174671,-2.96922295374569,6.));
#81369=CARTESIAN_POINT('Ctrl Pts',(14.2062007174671,-2.96922295374569,6.));
#81370=CARTESIAN_POINT('Ctrl Pts',(13.2234854900245,-2.70650147589439,5.94732494375275));
#81371=CARTESIAN_POINT('Ctrl Pts',(12.123801666398,-1.66916420549225,5.87785090488653));
#81372=CARTESIAN_POINT('Ctrl Pts',(11.9273055846846,-0.328588204067301,
5.80837686602031));
#81373=CARTESIAN_POINT('Ctrl Pts',(11.9296688268652,-0.00354280879104964,
5.79157788340132));
#81374=CARTESIAN_POINT('',(15.7942157255603,-2.96911158956221,5.99999996441182));
#81375=CARTESIAN_POINT('Origin',(15.,0.,6.));
#81376=CARTESIAN_POINT('',(11.9263421499922,0.00192556373082606,5.70842344717746));
#81377=CARTESIAN_POINT('Ctrl Pts',(15.7942157255603,-2.96911158956221,5.99999996441182));
#81378=CARTESIAN_POINT('Ctrl Pts',(15.7018690189097,-2.9938136610113,5.9950202108322));
#81379=CARTESIAN_POINT('Ctrl Pts',(15.6082018290729,-3.01424790828694,5.99004045725257));
#81380=CARTESIAN_POINT('Ctrl Pts',(15.513646119697,-3.03027555079075,5.98506070367295));
#81381=CARTESIAN_POINT('Ctrl Pts',(15.4192176285349,-3.04628162920221,5.9800876500098));
#81382=CARTESIAN_POINT('Ctrl Pts',(15.3239034261041,-3.05789281051075,5.97511459634665));
#81383=CARTESIAN_POINT('Ctrl Pts',(15.2281494838423,-3.06502040173022,5.9701415426835));
#81384=CARTESIAN_POINT('Ctrl Pts',(15.1293011648268,-3.07237832761852,5.9650077802152));
#81385=CARTESIAN_POINT('Ctrl Pts',(15.0299846568516,-3.07495779380533,5.9598740177469));
#81386=CARTESIAN_POINT('Ctrl Pts',(14.9307009746042,-3.07271864886442,5.95474025527859));
#81387=CARTESIAN_POINT('Ctrl Pts',(14.8346927168438,-3.07055337457379,5.94977585851992));
#81388=CARTESIAN_POINT('Ctrl Pts',(14.7387156335956,-3.06388244854816,5.94481146176125));
#81389=CARTESIAN_POINT('Ctrl Pts',(14.6432254126159,-3.05272241512341,5.93984706500257));
#81390=CARTESIAN_POINT('Ctrl Pts',(14.5477665125112,-3.04156604219928,5.93488429657033));
#81391=CARTESIAN_POINT('Ctrl Pts',(14.4527945968673,-3.0259235385553,5.92992152813808));
#81392=CARTESIAN_POINT('Ctrl Pts',(14.3587608067155,-3.00586336133162,5.92495875970583));
#81393=CARTESIAN_POINT('Ctrl Pts',(14.2647316542963,-2.98580417347293,5.91999623603659));
#81394=CARTESIAN_POINT('Ctrl Pts',(14.1716409683242,-2.96132783829202,5.91503371236735));
#81395=CARTESIAN_POINT('Ctrl Pts',(14.0799291539908,-2.93255381678222,5.91007118869811));
#81396=CARTESIAN_POINT('Ctrl Pts',(13.988196304435,-2.90377319559986,5.90510752681358));
#81397=CARTESIAN_POINT('Ctrl Pts',(13.8978433768556,-2.87069306354472,5.90014386492905));
#81398=CARTESIAN_POINT('Ctrl Pts',(13.8092940107979,-2.83348222109797,5.89518020304453));
#81399=CARTESIAN_POINT('Ctrl Pts',(13.7206496084393,-2.79623144182301,5.89021121387099));
#81400=CARTESIAN_POINT('Ctrl Pts',(13.6338130385796,-2.75484127792406,5.88524222469745));
#81401=CARTESIAN_POINT('Ctrl Pts',(13.5491860704935,-2.70952785406421,5.88027323552391));
#81402=CARTESIAN_POINT('Ctrl Pts',(13.4645045392964,-2.66418521444219,5.87530104260204));
#81403=CARTESIAN_POINT('Ctrl Pts',(13.382035824584,-2.61491450741817,5.87032884968017));
#81404=CARTESIAN_POINT('Ctrl Pts',(13.302153493731,-2.56197570073375,5.86535665675831));
#81405=CARTESIAN_POINT('Ctrl Pts',(13.2221525535056,-2.5089582904511,5.86037708111894));
#81406=CARTESIAN_POINT('Ctrl Pts',(13.1447460146018,-2.45226217550332,5.85539750547957));
#81407=CARTESIAN_POINT('Ctrl Pts',(13.0702748154839,-2.39218790278783,5.8504179298402));
#81408=CARTESIAN_POINT('Ctrl Pts',(13.0528932997578,-2.3781666176694,5.84925570104154));
#81409=CARTESIAN_POINT('Ctrl Pts',(13.0356715282748,-2.36396146459253,5.84809347224288));
#81410=CARTESIAN_POINT('Ctrl Pts',(13.0186135388797,-2.3495765451862,5.84693124344422));
#81411=CARTESIAN_POINT('Ctrl Pts',(12.9461274939369,-2.28844941640039,5.8419924803238));
#81412=CARTESIAN_POINT('Ctrl Pts',(12.8763338057764,-2.22384729599405,5.83705371720339));
#81413=CARTESIAN_POINT('Ctrl Pts',(12.8095899402503,-2.15603942917273,5.83211495408297));
#81414=CARTESIAN_POINT('Ctrl Pts',(12.7399398316576,-2.08527898923837,5.82696114129524));
#81415=CARTESIAN_POINT('Ctrl Pts',(12.6736116136119,-2.01102751315833,5.82180732850751));
#81416=CARTESIAN_POINT('Ctrl Pts',(12.6109747270326,-1.93363918431624,5.81665351571978));
#81417=CARTESIAN_POINT('Ctrl Pts',(12.5510981539129,-1.85966124282541,5.81172682371635));
#81418=CARTESIAN_POINT('Ctrl Pts',(12.4945948013533,-1.78281744761207,5.80680013171291));
#81419=CARTESIAN_POINT('Ctrl Pts',(12.4417498504224,-1.70345484888395,5.80187343970948));
#81420=CARTESIAN_POINT('Ctrl Pts',(12.3889350558613,-1.62413753902143,5.79694955916));
#81421=CARTESIAN_POINT('Ctrl Pts',(12.3397747666994,-1.54230465394821,5.79202567861052));
#81422=CARTESIAN_POINT('Ctrl Pts',(12.2945124128363,-1.45833438062172,5.78710179806104));
#81423=CARTESIAN_POINT('Ctrl Pts',(12.2492628016601,-1.37438774740224,5.78217930372907));
#81424=CARTESIAN_POINT('Ctrl Pts',(12.2079091590888,-1.28830531801229,5.77725680939711));
#81425=CARTESIAN_POINT('Ctrl Pts',(12.1706496583682,-1.20049110546804,5.77233431506514));
#81426=CARTESIAN_POINT('Ctrl Pts',(12.1333898750263,-1.11267622683443,5.76741178339501));
#81427=CARTESIAN_POINT('Ctrl Pts',(12.1002244689673,-1.02312995478895,5.76248925172488));
#81428=CARTESIAN_POINT('Ctrl Pts',(12.0713035446006,-0.932276419379552,
5.75756672005475));
#81429=CARTESIAN_POINT('Ctrl Pts',(12.0423595738702,-0.841350485052403,
5.75264026574183));
#81430=CARTESIAN_POINT('Ctrl Pts',(12.0176669722261,-0.749115638273084,
5.74771381142891));
#81431=CARTESIAN_POINT('Ctrl Pts',(11.997325838759,-0.656010770807662,5.742787357116));
#81432=CARTESIAN_POINT('Ctrl Pts',(11.9769751316778,-0.562862083263512,
5.73785858415292));
#81433=CARTESIAN_POINT('Ctrl Pts',(11.9609800447889,-0.468843004043297,
5.73292981118984));
#81434=CARTESIAN_POINT('Ctrl Pts',(11.9493891151334,-0.374400159098826,
5.72800103822676));
#81435=CARTESIAN_POINT('Ctrl Pts',(11.937782976746,-0.279833393473294,5.7230657981046));
#81436=CARTESIAN_POINT('Ctrl Pts',(11.9305925596139,-0.18484220117705,5.71813055798245));
#81437=CARTESIAN_POINT('Ctrl Pts',(11.927814348961,-0.0898753333799633,
5.71319531786029));
#81438=CARTESIAN_POINT('Ctrl Pts',(11.9269189341053,-0.059267595217704,
5.71160469429934));
#81439=CARTESIAN_POINT('Ctrl Pts',(11.9264814406799,-0.0286623583123479,
5.7100140707384));
#81440=CARTESIAN_POINT('Ctrl Pts',(11.9265006031257,0.00192546446421238,
5.70842344717746));
#81441=CARTESIAN_POINT('Ctrl Pts',(11.923315925464,0.00192745957886042,
5.70842344717746));
#81442=CARTESIAN_POINT('Ctrl Pts',(11.9223646639316,0.127164633308888,5.70191765635247));
#81443=CARTESIAN_POINT('Ctrl Pts',(11.985990549022,1.26546775157098,5.64273680928023));
#81444=CARTESIAN_POINT('Ctrl Pts',(13.405195535622,3.25791114562133,5.53088090596076));
#81445=CARTESIAN_POINT('Ctrl Pts',(15.8434703833997,3.157100543563,5.41926966138385));
#81446=CARTESIAN_POINT('Ctrl Pts',(16.7793150670081,2.51416252948969,5.3603334730542));
#81447=CARTESIAN_POINT('Ctrl Pts',(16.8743174193178,2.43995797974749,5.35407234097178));
#81448=CARTESIAN_POINT('Origin',(-15.,0.,8.20842344717746));
#81449=CARTESIAN_POINT('',(-13.1276888212995,2.43738653071546,0.437234105223613));
#81450=CARTESIAN_POINT('',(-13.1274106822325,2.43775135620018,0.35431326766678));
#81451=CARTESIAN_POINT('',(-13.1276888212995,2.43738653071547,8.20842344717746));
#81452=CARTESIAN_POINT('',(-14.2062007174672,-2.96922295374571,0.));
#81453=CARTESIAN_POINT('Ctrl Pts',(-13.1274106822327,2.43775135620036,0.354313267666796));
#81454=CARTESIAN_POINT('Ctrl Pts',(-12.9306016871905,2.28966113378113,0.341558957605688));
#81455=CARTESIAN_POINT('Ctrl Pts',(-12.0147638306694,1.41166373576771,0.276129591297334));
#81456=CARTESIAN_POINT('Ctrl Pts',(-11.5559315165978,-1.13347874614163,
0.158025168741734));
#81457=CARTESIAN_POINT('Ctrl Pts',(-13.2234854900246,-2.70650147589444,
0.052675056247244));
#81458=CARTESIAN_POINT('Ctrl Pts',(-14.2062007174672,-2.96922295374571,
-1.11022302462516E-15));
#81459=CARTESIAN_POINT('',(-15.793800408736,-2.96922265266357,2.23784480712919E-5));
#81460=CARTESIAN_POINT('Origin',(-15.,0.,0.));
#81461=CARTESIAN_POINT('Ctrl Pts',(-13.1276888212995,2.43738653071546,0.437234105223613));
#81462=CARTESIAN_POINT('Ctrl Pts',(-13.051399308353,2.37878371737117,0.432252081048935));
#81463=CARTESIAN_POINT('Ctrl Pts',(-12.9777841872235,2.31653453736228,0.427270056874259));
#81464=CARTESIAN_POINT('Ctrl Pts',(-12.9072078238328,2.2509160707084,0.422288032699581));
#81465=CARTESIAN_POINT('Ctrl Pts',(-12.8366777068085,2.1853406016745,0.417309273081256));
#81466=CARTESIAN_POINT('Ctrl Pts',(-12.7691827111166,2.11640053297353,0.41233051346293));
#81467=CARTESIAN_POINT('Ctrl Pts',(-12.7050537698248,2.04441288652875,0.407351753844606));
#81468=CARTESIAN_POINT('Ctrl Pts',(-12.6409455242956,1.97244847201648,0.402374600977066));
#81469=CARTESIAN_POINT('Ctrl Pts',(-12.580201467203,1.89743876208184,0.397397448109526));
#81470=CARTESIAN_POINT('Ctrl Pts',(-12.5231146160657,1.81973653171346,0.392420295241986));
#81471=CARTESIAN_POINT('Ctrl Pts',(-12.4660305235926,1.74203805622663,0.387443382890316));
#81472=CARTESIAN_POINT('Ctrl Pts',(-12.4126035458098,1.66164767378587,0.382466470538644));
#81473=CARTESIAN_POINT('Ctrl Pts',(-12.3630847891828,1.57894915084718,0.377489558186974));
#81474=CARTESIAN_POINT('Ctrl Pts',(-12.3135548378086,1.49623193218328,0.372511520700507));
#81475=CARTESIAN_POINT('Ctrl Pts',(-12.2679350883388,1.41120591403631,0.367533483214042));
#81476=CARTESIAN_POINT('Ctrl Pts',(-12.2264313533922,1.32428063965096,0.362555445727575));
#81477=CARTESIAN_POINT('Ctrl Pts',(-12.1848815229759,1.23725882307816,0.357571879462148));
#81478=CARTESIAN_POINT('Ctrl Pts',(-12.1474570211995,1.14833393753415,0.35258831319672));
#81479=CARTESIAN_POINT('Ctrl Pts',(-12.1143159219649,1.05793650649491,0.347604746931292));
#81480=CARTESIAN_POINT('Ctrl Pts',(-12.0811538596383,0.967481895406963,
0.342618028357679));
#81481=CARTESIAN_POINT('Ctrl Pts',(-12.0522807251901,0.875553303798613,
0.337631309784064));
#81482=CARTESIAN_POINT('Ctrl Pts',(-12.0278044011559,0.782595407737358,
0.332644591210451));
#81483=CARTESIAN_POINT('Ctrl Pts',(-12.0032892032294,0.689489873688219,
0.327649952609304));
#81484=CARTESIAN_POINT('Ctrl Pts',(-11.9831848464325,0.595352201397336,
0.322655314008159));
#81485=CARTESIAN_POINT('Ctrl Pts',(-11.967547889997,0.500636045983782,0.317660675407011));
#81486=CARTESIAN_POINT('Ctrl Pts',(-11.9606949426945,0.459126381080979,
0.315471758703847));
#81487=CARTESIAN_POINT('Ctrl Pts',(-11.9546993565402,0.417505658357757,
0.313282842000683));
#81488=CARTESIAN_POINT('Ctrl Pts',(-11.9495627393769,0.375812145894949,
0.311093925297518));
#81489=CARTESIAN_POINT('Ctrl Pts',(-11.9378061418289,0.28038477982827,0.306083971873502));
#81490=CARTESIAN_POINT('Ctrl Pts',(-11.9305115409651,0.184241362270561,
0.301074018449483));
#81491=CARTESIAN_POINT('Ctrl Pts',(-11.9277553015649,0.0878337232349656,
0.296064065025466));
#81492=CARTESIAN_POINT('Ctrl Pts',(-11.9250027908209,-0.00844349500458069,
0.291060889094605));
#81493=CARTESIAN_POINT('Ctrl Pts',(-11.9267764507165,-0.10498379110377,
0.286057713163746));
#81494=CARTESIAN_POINT('Ctrl Pts',(-11.9331010727877,-0.201328637466599,
0.281054537232885));
#81495=CARTESIAN_POINT('Ctrl Pts',(-11.9394190239762,-0.297571864291274,
0.276056638392046));
#81496=CARTESIAN_POINT('Ctrl Pts',(-11.9502783655214,-0.393619617480418,
0.271058739551204));
#81497=CARTESIAN_POINT('Ctrl Pts',(-11.9656518423827,-0.489012789571698,
0.266060840710365));
#81498=CARTESIAN_POINT('Ctrl Pts',(-11.9810141469647,-0.584336637125618,
0.261066573964123));
#81499=CARTESIAN_POINT('Ctrl Pts',(-12.0008839948583,-0.679006419251,0.256072307217882));
#81500=CARTESIAN_POINT('Ctrl Pts',(-12.0251823410208,-0.772568537946865,
0.25107804047164));
#81501=CARTESIAN_POINT('Ctrl Pts',(-12.0494716577823,-0.866095888437748,
0.246085629622767));
#81502=CARTESIAN_POINT('Ctrl Pts',(-12.0781860928816,-0.958515970974263,
0.241093218773895));
#81503=CARTESIAN_POINT('Ctrl Pts',(-12.1111957749357,-1.04938667766029,
0.236100807925022));
#81504=CARTESIAN_POINT('Ctrl Pts',(-12.1442020994384,-1.14024814151051,
0.231108904874926));
#81505=CARTESIAN_POINT('Ctrl Pts',(-12.1815026527877,-1.22956013227293,
0.226117001824831));
#81506=CARTESIAN_POINT('Ctrl Pts',(-12.2229184401607,-1.31689796871308,
0.221125098774736));
#81507=CARTESIAN_POINT('Ctrl Pts',(-12.2643411924436,-1.40425049279284,
0.216132356234265));
#81508=CARTESIAN_POINT('Ctrl Pts',(-12.3098803659345,-1.48962780842408,
0.211139613693793));
#81509=CARTESIAN_POINT('Ctrl Pts',(-12.3593102542769,-1.57262834669633,
0.206146871153322));
#81510=CARTESIAN_POINT('Ctrl Pts',(-12.4087914080391,-1.65571496765213,
0.201148950469611));
#81511=CARTESIAN_POINT('Ctrl Pts',(-12.4621711086895,-1.73641951396408,
0.196151029785898));
#81512=CARTESIAN_POINT('Ctrl Pts',(-12.5191795264361,-1.81436821729934,
0.191153109102187));
#81513=CARTESIAN_POINT('Ctrl Pts',(-12.5762206812606,-1.89236168266945,
0.186152318363039));
#81514=CARTESIAN_POINT('Ctrl Pts',(-12.6368944289551,-1.9675958133395,0.181151527623891));
#81515=CARTESIAN_POINT('Ctrl Pts',(-12.700891057101,-2.03973045245736,0.176150736884743));
#81516=CARTESIAN_POINT('Ctrl Pts',(-12.7649871612133,-2.11197721721588,
0.171142172947139));
#81517=CARTESIAN_POINT('Ctrl Pts',(-12.8324161544441,-2.18111455760436,
0.166133609009538));
#81518=CARTESIAN_POINT('Ctrl Pts',(-12.9028320208184,-2.24683971771357,
0.161125045071934));
#81519=CARTESIAN_POINT('Ctrl Pts',(-12.9405867240755,-2.28207941643806,
0.158439615566548));
#81520=CARTESIAN_POINT('Ctrl Pts',(-12.9791995150684,-2.31633888882833,
0.15575418606116));
#81521=CARTESIAN_POINT('Ctrl Pts',(-13.018613470118,-2.34957648719979,0.153068756555774));
#81522=CARTESIAN_POINT('Ctrl Pts',(-13.0916972789461,-2.41120771101968,
0.148089266008675));
#81523=CARTESIAN_POINT('Ctrl Pts',(-13.1677905197507,-2.46953626920912,
0.143109775461575));
#81524=CARTESIAN_POINT('Ctrl Pts',(-13.2465609561695,-2.52425311123324,
0.138130284914476));
#81525=CARTESIAN_POINT('Ctrl Pts',(-13.325226390291,-2.57889701480006,0.133157432110807));
#81526=CARTESIAN_POINT('Ctrl Pts',(-13.4065615679657,-2.62993851859708,
0.12818457930714));
#81527=CARTESIAN_POINT('Ctrl Pts',(-13.4902003138964,-2.67710798397105,
0.12321172650347));
#81528=CARTESIAN_POINT('Ctrl Pts',(-13.5765307278305,-2.72579546039684,
0.118078837001162));
#81529=CARTESIAN_POINT('Ctrl Pts',(-13.6653151432676,-2.77035711985146,
0.112945947498849));
#81530=CARTESIAN_POINT('Ctrl Pts',(-13.7561171347479,-2.8105440162951,0.107813057996541));
#81531=CARTESIAN_POINT('Ctrl Pts',(-13.8439376419678,-2.84941137560889,
0.102848706970231));
#81532=CARTESIAN_POINT('Ctrl Pts',(-13.9336448601417,-2.88418658323434,
0.0978843559439239));
#81533=CARTESIAN_POINT('Ctrl Pts',(-14.0248191542394,-2.91469116169477,
0.0929200049176142));
#81534=CARTESIAN_POINT('Ctrl Pts',(-14.1159645905075,-2.94518608506617,
0.0879572251718644));
#81535=CARTESIAN_POINT('Ctrl Pts',(-14.2085757605611,-2.97141292435503,
0.0829944454261152));
#81536=CARTESIAN_POINT('Ctrl Pts',(-14.3022151173914,-2.99324213982146,
0.0780316656803652));
#81537=CARTESIAN_POINT('Ctrl Pts',(-14.3958509308654,-3.01507052926033,
0.0730690737284831));
#81538=CARTESIAN_POINT('Ctrl Pts',(-14.4905144223162,-3.03250152590661,
0.0681064817766009));
#81539=CARTESIAN_POINT('Ctrl Pts',(-14.5857561229236,-3.04545633038871,
0.063143889824719));
#81540=CARTESIAN_POINT('Ctrl Pts',(-14.6810207609007,-3.05841425481867,
0.0581801027156136));
#81541=CARTESIAN_POINT('Ctrl Pts',(-14.7768634458436,-3.06689378697388,
0.0532163156065092));
#81542=CARTESIAN_POINT('Ctrl Pts',(-14.8728289534792,-3.07086791883448,
0.0482525284974038));
#81543=CARTESIAN_POINT('Ctrl Pts',(-14.9688990315199,-3.07484638117369,
0.0432833325154427));
#81544=CARTESIAN_POINT('Ctrl Pts',(-15.0650917564406,-3.07430962911643,
0.03831413653348));
#81545=CARTESIAN_POINT('Ctrl Pts',(-15.1609516192215,-3.06928278695039,
0.0333449405515189));
#81546=CARTESIAN_POINT('Ctrl Pts',(-15.2568742304286,-3.06425265428898,
0.0283724918085184));
#81547=CARTESIAN_POINT('Ctrl Pts',(-15.3524631060846,-3.05472662614582,
0.0234000430655198));
#81548=CARTESIAN_POINT('Ctrl Pts',(-15.4472696718276,-3.04078149340974,
0.0184275943225192));
#81549=CARTESIAN_POINT('Ctrl Pts',(-15.5422182387491,-3.02681547366795,
0.0134476978508148));
#81550=CARTESIAN_POINT('Ctrl Pts',(-15.6363817250837,-3.00841722912106,
0.00846780137910505));
#81551=CARTESIAN_POINT('Ctrl Pts',(-15.7293238804778,-2.98571414026272,
0.00348790490740036));
#81552=CARTESIAN_POINT('Ctrl Pts',(-15.7508834651356,-2.9804477553359,0.00233272942095613));
#81553=CARTESIAN_POINT('Ctrl Pts',(-15.7723774072569,-2.97494993866391,
0.00117755393451479));
#81554=CARTESIAN_POINT('Ctrl Pts',(-15.793800408736,-2.96922265266357,2.23784480706257E-5));
#81555=CARTESIAN_POINT('Origin',(-15.,0.,8.20842344717746));
#81556=CARTESIAN_POINT('',(-13.1276888212995,2.43738653071547,1.43740553117474));
#81557=CARTESIAN_POINT('',(-13.1276888212995,2.43738653071547,1.35414034322078));
#81558=CARTESIAN_POINT('',(-13.1276888212995,2.43738653071547,8.20842344717746));
#81559=CARTESIAN_POINT('',(-18.0729669117909,0.00038412414453365,0.708423426334819));
#81560=CARTESIAN_POINT('Ctrl Pts',(-13.1276888212995,2.43738653071547,1.35414034322078));
#81561=CARTESIAN_POINT('Ctrl Pts',(-13.0511528609175,2.37859440546573,1.34915698327503));
#81562=CARTESIAN_POINT('Ctrl Pts',(-12.9773706598892,2.31618001504235,1.34417362332928));
#81563=CARTESIAN_POINT('Ctrl Pts',(-12.9066944270949,2.25043863023291,1.33919026338353));
#81564=CARTESIAN_POINT('Ctrl Pts',(-12.8360138629279,2.18469321648145,1.33420659803398));
#81565=CARTESIAN_POINT('Ctrl Pts',(-12.7684399658257,2.11562070261525,1.32922293268444));
#81566=CARTESIAN_POINT('Ctrl Pts',(-12.7042891787565,2.04355427508681,1.3242392673349));
#81567=CARTESIAN_POINT('Ctrl Pts',(-12.6398874552402,1.97120594777026,1.31923610755148));
#81568=CARTESIAN_POINT('Ctrl Pts',(-12.5789359777004,1.89584056428445,1.31423294776806));
#81569=CARTESIAN_POINT('Ctrl Pts',(-12.5217140883649,1.81782870210342,1.30922978798464));
#81570=CARTESIAN_POINT('Ctrl Pts',(-12.464630368716,1.74000520969961,1.30423870898058));
#81571=CARTESIAN_POINT('Ctrl Pts',(-12.4112584556626,1.65954839497049,1.29924762997651));
#81572=CARTESIAN_POINT('Ctrl Pts',(-12.3618313474449,1.57685395984401,1.29425655097245));
#81573=CARTESIAN_POINT('Ctrl Pts',(-12.3122247836463,1.49385928506286,1.28924735079935));
#81574=CARTESIAN_POINT('Ctrl Pts',(-12.2665919228553,1.40861110815873,1.28423815062626));
#81575=CARTESIAN_POINT('Ctrl Pts',(-12.2251204633718,1.32153161415148,1.27922895045317));
#81576=CARTESIAN_POINT('Ctrl Pts',(-12.1836490038882,1.23445212014421,1.27421975028007));
#81577=CARTESIAN_POINT('Ctrl Pts',(-12.1463390605124,1.14554173821997,1.26921055010698));
#81578=CARTESIAN_POINT('Ctrl Pts',(-12.1133282369444,1.05523854287914,1.26420134993389));
#81579=CARTESIAN_POINT('Ctrl Pts',(-12.0803779751112,0.965101017993265,
1.25920133965123));
#81580=CARTESIAN_POINT('Ctrl Pts',(-12.0515960334417,0.873261122870222,
1.25420132936858));
#81581=CARTESIAN_POINT('Ctrl Pts',(-12.0271589963609,0.780140126568347,
1.24920131908592));
#81582=CARTESIAN_POINT('Ctrl Pts',(-12.0027549758747,0.687144944953781,
1.24420806425859));
#81583=CARTESIAN_POINT('Ctrl Pts',(-11.9826843033618,0.592872523079586,
1.23921480943126));
#81584=CARTESIAN_POINT('Ctrl Pts',(-11.9670748685875,0.497762390349688,
1.23422155460393));
#81585=CARTESIAN_POINT('Ctrl Pts',(-11.9514818203138,0.402752102506203,
1.22923354160465));
#81586=CARTESIAN_POINT('Ctrl Pts',(-11.9403407701969,0.306906282816328,
1.22424552860537));
#81587=CARTESIAN_POINT('Ctrl Pts',(-11.9337290537548,0.210676847833027,
1.21925751560608));
#81588=CARTESIAN_POINT('Ctrl Pts',(-11.927122028302,0.114515687290051,1.2142730415842));
#81589=CARTESIAN_POINT('Ctrl Pts',(-11.9250379781261,0.0179718890919223,
1.20928856756232));
#81590=CARTESIAN_POINT('Ctrl Pts',(-11.9275025484609,-0.0784962437677143,
1.20430409354044));
#81591=CARTESIAN_POINT('Ctrl Pts',(-11.9299662316253,-0.174929651031547,
1.19932141377771));
#81592=CARTESIAN_POINT('Ctrl Pts',(-11.9369752707827,-0.271287008817974,
1.19433873401497));
#81593=CARTESIAN_POINT('Ctrl Pts',(-11.9485032013853,-0.367109708458424,
1.18935605425224));
#81594=CARTESIAN_POINT('Ctrl Pts',(-11.9600301272186,-0.462924056233761,
1.18437380877773));
#81595=CARTESIAN_POINT('Ctrl Pts',(-11.9760751087741,-0.558203402842771,
1.17939156330321));
#81596=CARTESIAN_POINT('Ctrl Pts',(-11.9965598908141,-0.652495027209744,
1.1744093178287));
#81597=CARTESIAN_POINT('Ctrl Pts',(-12.0170484757832,-0.746804156491061,
1.16942614741752));
#81598=CARTESIAN_POINT('Ctrl Pts',(-12.0419784049871,-0.840124770540819,
1.16444297700634));
#81599=CARTESIAN_POINT('Ctrl Pts',(-12.0712207052525,-0.932016143990043,
1.15945980659517));
#81600=CARTESIAN_POINT('Ctrl Pts',(-12.1004944921847,-1.02400646153868,
1.15447127055183));
#81601=CARTESIAN_POINT('Ctrl Pts',(-12.1340897866456,-1.11456404737922,
1.14948273450849));
#81602=CARTESIAN_POINT('Ctrl Pts',(-12.1718283629447,-1.20326532458815,
1.14449419846516));
#81603=CARTESIAN_POINT('Ctrl Pts',(-12.2095893537256,-1.29201928510813,
1.13950269952654));
#81604=CARTESIAN_POINT('Ctrl Pts',(-12.2514983357602,-1.37891434662163,
1.13451120058792));
#81605=CARTESIAN_POINT('Ctrl Pts',(-12.2973306779117,-1.46355074576965,
1.12951970164929));
#81606=CARTESIAN_POINT('Ctrl Pts',(-12.3432365532322,-1.54832293511182,
1.124520194376));
#81607=CARTESIAN_POINT('Ctrl Pts',(-12.3930781303693,-1.63082885118772,
1.1195206871027));
#81608=CARTESIAN_POINT('Ctrl Pts',(-12.4465870068629,-1.71069703234628,
1.11452117982941));
#81609=CARTESIAN_POINT('Ctrl Pts',(-12.4763587074866,-1.75513473567015,
1.11173951361699));
#81610=CARTESIAN_POINT('Ctrl Pts',(-12.5072649463413,-1.7987564516688,1.10895784740456));
#81611=CARTESIAN_POINT('Ctrl Pts',(-12.5392542688128,-1.84150283639315,
1.10617618119214));
#81612=CARTESIAN_POINT('Ctrl Pts',(-12.5967762887544,-1.91836780897057,
1.10117429159339));
#81613=CARTESIAN_POINT('Ctrl Pts',(-12.6580034329227,-1.99266890753169,
1.09617240199463));
#81614=CARTESIAN_POINT('Ctrl Pts',(-12.7226790194845,-2.06402795564982,
1.09117051239587));
#81615=CARTESIAN_POINT('Ctrl Pts',(-12.7872672215848,-2.13529058914964,
1.08617538094887));
#81616=CARTESIAN_POINT('Ctrl Pts',(-12.8552943138539,-2.20361875046076,
1.08118024950187));
#81617=CARTESIAN_POINT('Ctrl Pts',(-12.9264617303691,-2.26866509083559,
1.07618511805487));
#81618=CARTESIAN_POINT('Ctrl Pts',(-12.9975543911876,-2.33364310521622,
1.07119523359517));
#81619=CARTESIAN_POINT('Ctrl Pts',(-13.071780496557,-2.3953458575995,1.06620534913548));
#81620=CARTESIAN_POINT('Ctrl Pts',(-13.1488034987124,-2.4534615879652,1.06121546467578));
#81621=CARTESIAN_POINT('Ctrl Pts',(-13.2257716378871,-2.51153592287618,
1.05622913447816));
#81622=CARTESIAN_POINT('Ctrl Pts',(-13.3055323642548,-2.56602805183336,
1.05124280428054));
#81623=CARTESIAN_POINT('Ctrl Pts',(-13.3877155532199,-2.61666603002201,
1.04625647408292));
#81624=CARTESIAN_POINT('Ctrl Pts',(-13.469869002451,-2.66728568378177,1.04127194829488));
#81625=CARTESIAN_POINT('Ctrl Pts',(-13.5544427995286,-2.71405372823244,
1.03628742250684));
#81626=CARTESIAN_POINT('Ctrl Pts',(-13.641038102371,-2.75674170186339,1.0313028967188));
#81627=CARTESIAN_POINT('Ctrl Pts',(-13.7276256457696,-2.7994258504031,1.02631881757332));
#81628=CARTESIAN_POINT('Ctrl Pts',(-13.8162339413956,-2.83803046134822,
1.02133473842784));
#81629=CARTESIAN_POINT('Ctrl Pts',(-13.9064407874791,-2.87237366975653,
1.01635065928236));
#81630=CARTESIAN_POINT('Ctrl Pts',(-13.9966641103045,-2.9067231511276,1.01136566976933));
#81631=CARTESIAN_POINT('Ctrl Pts',(-14.088486153683,-2.93680952812858,1.00638068025629));
#81632=CARTESIAN_POINT('Ctrl Pts',(-14.1814670537934,-2.96249996894082,
1.00139569074325));
#81633=CARTESIAN_POINT('Ctrl Pts',(-14.2745474178067,-2.98821789143486,
0.996405368667162));
#81634=CARTESIAN_POINT('Ctrl Pts',(-14.3687886900333,-3.00953037299097,
0.991415046591069));
#81635=CARTESIAN_POINT('Ctrl Pts',(-14.463738460438,-3.02635520241537,0.986424724514978));
#81636=CARTESIAN_POINT('Ctrl Pts',(-14.5587442987757,-3.04318996691812,
0.981431455648782));
#81637=CARTESIAN_POINT('Ctrl Pts',(-14.6544590336937,-3.05553174657388,
0.976438186782588));
#81638=CARTESIAN_POINT('Ctrl Pts',(-14.7504248369792,-3.06335020655542,
0.971444917916392));
#81639=CARTESIAN_POINT('Ctrl Pts',(-14.8465437369471,-3.07118113952467,
0.9664436831616));
#81640=CARTESIAN_POINT('Ctrl Pts',(-14.9429140671563,-3.07447432925586,
0.961442448406806));
#81641=CARTESIAN_POINT('Ctrl Pts',(-15.0390777808304,-3.07325156423052,
0.956441213652014));
#81642=CARTESIAN_POINT('Ctrl Pts',(-15.0922124281551,-3.0725759332061,0.953677813251482));
#81643=CARTESIAN_POINT('Ctrl Pts',(-15.1452840680108,-3.07052248433969,
0.95091441285095));
#81644=CARTESIAN_POINT('Ctrl Pts',(-15.1982164315189,-3.06710164426872,
0.948151012450418));
#81645=CARTESIAN_POINT('Ctrl Pts',(-15.2940290516472,-3.06090959788129,
0.943148994492202));
#81646=CARTESIAN_POINT('Ctrl Pts',(-15.3897176588972,-3.05021288875187,
0.938146976533989));
#81647=CARTESIAN_POINT('Ctrl Pts',(-15.4848252204982,-3.03502005851178,
0.933144958575774));
#81648=CARTESIAN_POINT('Ctrl Pts',(-15.5798046352281,-3.01984769892225,
0.928149680280945));
#81649=CARTESIAN_POINT('Ctrl Pts',(-15.6742041310068,-3.00019132713698,
0.923154401986114));
#81650=CARTESIAN_POINT('Ctrl Pts',(-15.7675696339611,-2.9761114070244,0.918159123691285));
#81651=CARTESIAN_POINT('Ctrl Pts',(-15.8608374034989,-2.95205669336165,
0.913169074368608));
#81652=CARTESIAN_POINT('Ctrl Pts',(-15.9530729096405,-2.92358774575591,
0.90817902504593));
#81653=CARTESIAN_POINT('Ctrl Pts',(-16.0438311560454,-2.89081628051124,
0.903188975723253));
#81654=CARTESIAN_POINT('Ctrl Pts',(-16.1345252279343,-2.85806798773857,
0.898202454829265));
#81655=CARTESIAN_POINT('Ctrl Pts',(-16.2237437054578,-2.82102337386311,
0.893215933935281));
#81656=CARTESIAN_POINT('Ctrl Pts',(-16.3110566129781,-2.7798440257623,0.888229413041294));
#81657=CARTESIAN_POINT('Ctrl Pts',(-16.3983382035833,-2.73867944764435,
0.883244680685288));
#81658=CARTESIAN_POINT('Ctrl Pts',(-16.4837151860966,-2.69338326887045,
0.878259948329282));
#81659=CARTESIAN_POINT('Ctrl Pts',(-16.5667783337623,-2.64416487815208,
0.873275215973276));
#81660=CARTESIAN_POINT('Ctrl Pts',(-16.6498342971844,-2.59495074439866,
0.86829091475349));
#81661=CARTESIAN_POINT('Ctrl Pts',(-16.7305764465929,-2.54181529688789,
0.863306613533704));
#81662=CARTESIAN_POINT('Ctrl Pts',(-16.8086218371115,-2.48501293765718,
0.858322312313918));
#81663=CARTESIAN_POINT('Ctrl Pts',(-16.8866817196699,-2.42820003094824,
0.853337085572564));
#81664=CARTESIAN_POINT('Ctrl Pts',(-16.9620434943531,-2.36771911822442,
0.848351858831209));
#81665=CARTESIAN_POINT('Ctrl Pts',(-17.0343556498668,-2.30386617229709,
0.843366632089855));
#81666=CARTESIAN_POINT('Ctrl Pts',(-17.106745465764,-2.23994465084152,0.83837605141295));
#81667=CARTESIAN_POINT('Ctrl Pts',(-17.1760787949031,-2.17264415716956,
0.833385470736046));
#81668=CARTESIAN_POINT('Ctrl Pts',(-17.2420396810971,-2.1022988175771,0.828394890059141));
#81669=CARTESIAN_POINT('Ctrl Pts',(-17.3080396798945,-2.03191176554673,
0.823401350134505));
#81670=CARTESIAN_POINT('Ctrl Pts',(-17.370662969492,-1.95847660590655,0.81840781020987));
#81671=CARTESIAN_POINT('Ctrl Pts',(-17.4296340943692,-1.88236033146656,
0.813414270285233));
#81672=CARTESIAN_POINT('Ctrl Pts',(-17.4886994892553,-1.80612237913951,
0.808412747791935));
#81673=CARTESIAN_POINT('Ctrl Pts',(-17.5441008104129,-1.72719511273795,
0.803411225298637));
#81674=CARTESIAN_POINT('Ctrl Pts',(-17.5956061479273,-1.64597417198513,
0.79840970280534));
#81675=CARTESIAN_POINT('Ctrl Pts',(-17.6240416865902,-1.60113297081111,
0.795648416439785));
#81676=CARTESIAN_POINT('Ctrl Pts',(-17.6512905328349,-1.55559309417903,
0.792887130074228));
#81677=CARTESIAN_POINT('Ctrl Pts',(-17.6773198464595,-1.50942395957991,
0.790125843708673));
#81678=CARTESIAN_POINT('Ctrl Pts',(-17.7264573005471,-1.42226708082616,
0.7849131598874));
#81679=CARTESIAN_POINT('Ctrl Pts',(-17.7714055398365,-1.33258368240962,
0.779700476066124));
#81680=CARTESIAN_POINT('Ctrl Pts',(-17.8119086602719,-1.24079488082752,
0.774487792244851));
#81681=CARTESIAN_POINT('Ctrl Pts',(-17.8523389474109,-1.14917113519486,
0.769284481946953));
#81682=CARTESIAN_POINT('Ctrl Pts',(-17.8883398717102,-1.05544987303415,
0.764081171649055));
#81683=CARTESIAN_POINT('Ctrl Pts',(-17.919700908017,-0.960077526934394,
0.758877861351157));
#81684=CARTESIAN_POINT('Ctrl Pts',(-17.9509937778641,-0.864912482504336,
0.753685860986975));
#81685=CARTESIAN_POINT('Ctrl Pts',(-17.9776667349434,-0.768103869508663,
0.748493860622791));
#81686=CARTESIAN_POINT('Ctrl Pts',(-17.9995573856055,-0.670117706421588,
0.743301860258608));
#81687=CARTESIAN_POINT('Ctrl Pts',(-18.0214192330996,-0.572260471064923,
0.738116691397999));
#81688=CARTESIAN_POINT('Ctrl Pts',(-18.0385112123576,-0.473229143462907,
0.73293152253739));
#81689=CARTESIAN_POINT('Ctrl Pts',(-18.0507206053183,-0.373505071299328,
0.72774635367678));
#81690=CARTESIAN_POINT('Ctrl Pts',(-18.0629117058791,-0.273930408088415,
0.722568953358229));
#81691=CARTESIAN_POINT('Ctrl Pts',(-18.0702347462959,-0.173665449625611,
0.717391553039679));
#81692=CARTESIAN_POINT('Ctrl Pts',(-18.0726281689781,-0.0732009918108132,
0.712214152721128));
#81693=CARTESIAN_POINT('Ctrl Pts',(-18.0732122948632,-0.048682175818936,
0.71095058420657));
#81694=CARTESIAN_POINT('Ctrl Pts',(-18.0735030397513,-0.0241515163599685,
0.709687015692014));
#81695=CARTESIAN_POINT('Ctrl Pts',(-18.0734999760384,0.000383786650054932,
0.708423447177457));
#81696=CARTESIAN_POINT('Ctrl Pts',(-18.0685384920293,0.000386927872650887,
0.708423253185047));
#81697=CARTESIAN_POINT('Ctrl Pts',(-18.0689057127741,0.493586641182848,
0.682982393779012));
#81698=CARTESIAN_POINT('Ctrl Pts',(-17.7245434653973,2.00734820677417,0.604866478125731));
#81699=CARTESIAN_POINT('Ctrl Pts',(-15.5876863906459,3.45239524460836,0.486829816286313));
#81700=CARTESIAN_POINT('Ctrl Pts',(-13.7434190668955,2.90127091574708,0.394234013852931));
#81701=CARTESIAN_POINT('Ctrl Pts',(-13.1274106822327,2.43775135620036,0.354313267666796));
#81702=CARTESIAN_POINT('',(-18.0734999054211,0.000762480339119835,0.791576552865793));
#81703=CARTESIAN_POINT('Ctrl Pts',(-18.0734999054209,0.000762481169335827,
0.791576552822548));
#81704=CARTESIAN_POINT('Ctrl Pts',(-18.0734897331699,0.0417660022134045,
0.789440845722604));
#81705=CARTESIAN_POINT('Ctrl Pts',(-18.0726590539714,0.0827584360577896,
0.787305138622661));
#81706=CARTESIAN_POINT('Ctrl Pts',(-18.0710089906967,0.1237175373978,0.785169431522718));
#81707=CARTESIAN_POINT('Ctrl Pts',(-18.0671444936551,0.21964496538364,0.780167542264262));
#81708=CARTESIAN_POINT('Ctrl Pts',(-18.0587743123539,0.315558236027131,
0.775165653005807));
#81709=CARTESIAN_POINT('Ctrl Pts',(-18.0458957639553,0.411000298198215,
0.770163763747351));
#81710=CARTESIAN_POINT('Ctrl Pts',(-18.0330346160107,0.50631340676763,0.765168632637455));
#81711=CARTESIAN_POINT('Ctrl Pts',(-18.0156772656074,0.601156141341239,
0.760173501527557));
#81712=CARTESIAN_POINT('Ctrl Pts',(-17.9938730087447,0.695073131051469,
0.755178370417661));
#81713=CARTESIAN_POINT('Ctrl Pts',(-17.9720916555014,0.788891468512587,
0.750188486291512));
#81714=CARTESIAN_POINT('Ctrl Pts',(-17.9458727806176,0.881785569398113,
0.745198602165363));
#81715=CARTESIAN_POINT('Ctrl Pts',(-17.915317139935,0.973307877087693,0.740208718039215));
#81716=CARTESIAN_POINT('Ctrl Pts',(-17.8847832637967,1.06476499415235,0.735222388168555));
#81717=CARTESIAN_POINT('Ctrl Pts',(-17.8499189014104,1.15485184581244,0.730236058297896));
#81718=CARTESIAN_POINT('Ctrl Pts',(-17.8108750323348,1.24313466792495,0.725249728427236));
#81719=CARTESIAN_POINT('Ctrl Pts',(-17.7718452920814,1.33138554309363,0.720265202961968));
#81720=CARTESIAN_POINT('Ctrl Pts',(-17.72863922749,1.41783328525055,0.715280677496699));
#81721=CARTESIAN_POINT('Ctrl Pts',(-17.6814561150035,1.50206369815343,0.710296152031431));
#81722=CARTESIAN_POINT('Ctrl Pts',(-17.634277230356,1.5862865635968,0.705312073204175));
#81723=CARTESIAN_POINT('Ctrl Pts',(-17.5831222208386,1.66829211237906,0.700327994376919));
#81724=CARTESIAN_POINT('Ctrl Pts',(-17.5282360078883,1.7476913166853,0.695343915549662));
#81725=CARTESIAN_POINT('Ctrl Pts',(-17.4733397696355,1.82710502374163,0.690358926349937));
#81726=CARTESIAN_POINT('Ctrl Pts',(-17.4147112237775,1.90391108018195,0.685373937150211));
#81727=CARTESIAN_POINT('Ctrl Pts',(-17.3526376214765,1.97775086196756,0.680388947950486));
#81728=CARTESIAN_POINT('Ctrl Pts',(-17.2904976174322,2.051669632084,0.675398626178445));
#81729=CARTESIAN_POINT('Ctrl Pts',(-17.2249054824184,2.12261545669681,0.670408304406402));
#81730=CARTESIAN_POINT('Ctrl Pts',(-17.1561874805781,2.19026432162835,0.665417982634361));
#81731=CARTESIAN_POINT('Ctrl Pts',(-17.0874289006215,2.25795313334886,0.660424714067412));
#81732=CARTESIAN_POINT('Ctrl Pts',(-17.0155411048374,2.32234081635242,0.655431445500464));
#81733=CARTESIAN_POINT('Ctrl Pts',(-16.9408842074238,2.38314303879831,0.650438176933514));
#81734=CARTESIAN_POINT('Ctrl Pts',(-16.8661082078042,2.44404226070539,0.645436942467604));
#81735=CARTESIAN_POINT('Ctrl Pts',(-16.7885546382178,2.50134434053398,0.640435708001695));
#81736=CARTESIAN_POINT('Ctrl Pts',(-16.7086133177834,2.55480777756239,0.635434473535785));
#81737=CARTESIAN_POINT('Ctrl Pts',(-16.6644421970374,2.58434869482076,0.632671069950852));
#81738=CARTESIAN_POINT('Ctrl Pts',(-16.6195425459766,2.61271845698118,0.629907666365919));
#81739=CARTESIAN_POINT('Ctrl Pts',(-16.5739831242587,2.6398824546841,0.627144262780987));
#81740=CARTESIAN_POINT('Ctrl Pts',(-16.4915163487453,2.68905180794064,0.622142246194769));
#81741=CARTESIAN_POINT('Ctrl Pts',(-16.4066001453163,2.73443861633628,0.617140229608553));
#81742=CARTESIAN_POINT('Ctrl Pts',(-16.3196159936231,2.77579103669102,0.612138213022337));
#81743=CARTESIAN_POINT('Ctrl Pts',(-16.2327490435889,2.81708773916869,0.607142936108014));
#81744=CARTESIAN_POINT('Ctrl Pts',(-16.1438200757757,2.85436067080395,0.602147659193694));
#81745=CARTESIAN_POINT('Ctrl Pts',(-16.0532375423307,2.88740245366405,0.597152382279371));
#81746=CARTESIAN_POINT('Ctrl Pts',(-15.9627498292833,2.92040964889597,0.592162334343801));
#81747=CARTESIAN_POINT('Ctrl Pts',(-15.8706124014376,2.94919435098315,0.58717228640823));
#81748=CARTESIAN_POINT('Ctrl Pts',(-15.7772552616524,2.97359656110805,0.582182238472661));
#81749=CARTESIAN_POINT('Ctrl Pts',(-15.6839641341344,2.99798151657821,0.577195718969713));
#81750=CARTESIAN_POINT('Ctrl Pts',(-15.5894554322189,3.01799003000409,0.572209199466765));
#81751=CARTESIAN_POINT('Ctrl Pts',(-15.4941750289515,3.03351170934955,0.567222679963817));
#81752=CARTESIAN_POINT('Ctrl Pts',(-15.3989288003828,3.04902782145664,0.562237949000759));
#81753=CARTESIAN_POINT('Ctrl Pts',(-15.3029118527341,3.06006022673292,0.557253218037698));
#81754=CARTESIAN_POINT('Ctrl Pts',(-15.2065800368109,3.06654967975267,0.55226848707464));
#81755=CARTESIAN_POINT('Ctrl Pts',(-15.1102565527621,3.07303857149049,0.54728418724798));
#81756=CARTESIAN_POINT('Ctrl Pts',(-15.0136186920404,3.07498526297084,0.542299887421322));
#81757=CARTESIAN_POINT('Ctrl Pts',(-14.9171261439273,3.07238249148436,0.537315587594661));
#81758=CARTESIAN_POINT('Ctrl Pts',(-14.8206156783357,3.06977923669525,0.532330362244866));
#81759=CARTESIAN_POINT('Ctrl Pts',(-14.7242510172003,3.06262485300488,0.52734513689507));
#81760=CARTESIAN_POINT('Ctrl Pts',(-14.6284894927425,3.05096414154563,0.522359911545275));
#81761=CARTESIAN_POINT('Ctrl Pts',(-14.532625123974,3.03929090691658,0.517369332249125));
#81762=CARTESIAN_POINT('Ctrl Pts',(-14.437365620933,3.0231017359599,0.512378752952973));
#81763=CARTESIAN_POINT('Ctrl Pts',(-14.3431606265272,3.0024930120578,0.507388173656824));
#81764=CARTESIAN_POINT('Ctrl Pts',(-14.2488997716114,2.98187206785,0.50239463510881));
#81765=CARTESIAN_POINT('Ctrl Pts',(-14.1556950936047,2.95682646614238,0.497401096560798));
#81766=CARTESIAN_POINT('Ctrl Pts',(-14.0639814756913,2.92750261693324,0.492407558012784));
#81767=CARTESIAN_POINT('Ctrl Pts',(-13.9721212458973,2.89813189110122,0.487406036876205));
#81768=CARTESIAN_POINT('Ctrl Pts',(-13.8817572460333,2.86446941494189,0.482404515739625));
#81769=CARTESIAN_POINT('Ctrl Pts',(-13.7933047000624,2.82670987246808,0.477402994603045));
#81770=CARTESIAN_POINT('Ctrl Pts',(-13.7444707503213,2.80586312827126,0.47464169441511));
#81771=CARTESIAN_POINT('Ctrl Pts',(-13.6962190030361,2.78376839987139,0.471880394227175));
#81772=CARTESIAN_POINT('Ctrl Pts',(-13.6486158438361,2.76046429291688,0.46911909403924));
#81773=CARTESIAN_POINT('Ctrl Pts',(-13.5625000336455,2.71830633355279,0.464123803666508));
#81774=CARTESIAN_POINT('Ctrl Pts',(-13.4782063288343,2.6720401092025,0.45912851329378));
#81775=CARTESIAN_POINT('Ctrl Pts',(-13.396153501264,2.62184642160679,0.454133222921047));
#81776=CARTESIAN_POINT('Ctrl Pts',(-13.3142210451482,2.57172636812416,0.449145260636641));
#81777=CARTESIAN_POINT('Ctrl Pts',(-13.2345233024221,2.51769053448111,0.444157298352234));
#81778=CARTESIAN_POINT('Ctrl Pts',(-13.157456487099,2.45996659592493,0.43916933606783));
#81779=CARTESIAN_POINT('Ctrl Pts',(-13.1474896863913,2.45250134659235,0.438524259119758));
#81780=CARTESIAN_POINT('Ctrl Pts',(-13.1375668557,2.44497447542531,0.437879182171686));
#81781=CARTESIAN_POINT('Ctrl Pts',(-13.1276888212995,2.43738653071546,0.437234105223613));
#81782=CARTESIAN_POINT('Ctrl Pts',(-13.1276888212995,2.43738653071547,1.43740553117474));
#81783=CARTESIAN_POINT('Ctrl Pts',(-13.0512577645854,2.37867498862629,1.43240468041753));
#81784=CARTESIAN_POINT('Ctrl Pts',(-12.977690155484,2.31644121794465,1.42740382966033));
#81785=CARTESIAN_POINT('Ctrl Pts',(-12.9073088484283,2.25100999423224,1.42240297890312));
#81786=CARTESIAN_POINT('Ctrl Pts',(-12.8832290610115,2.22862379506477,1.42069202143197));
#81787=CARTESIAN_POINT('Ctrl Pts',(-12.8595219093937,2.20586361481061,1.41898106396081));
#81788=CARTESIAN_POINT('Ctrl Pts',(-12.8361992417048,2.1827433491827,1.41727010648965));
#81789=CARTESIAN_POINT('Ctrl Pts',(-12.768032105381,2.11516779050628,1.41226934616771));
#81790=CARTESIAN_POINT('Ctrl Pts',(-12.7029146328237,2.04427796376991,1.40726858584576));
#81791=CARTESIAN_POINT('Ctrl Pts',(-12.641185842504,1.97038017153966,1.40226782552381));
#81792=CARTESIAN_POINT('Ctrl Pts',(-12.579540424382,1.89658218721594,1.39727381933353));
#81793=CARTESIAN_POINT('Ctrl Pts',(-12.5212748710505,1.81978464557945,1.39227981314325));
#81794=CARTESIAN_POINT('Ctrl Pts',(-12.4666918889697,1.7403310790158,1.38728580695297));
#81795=CARTESIAN_POINT('Ctrl Pts',(-12.4121661951544,1.66096090395694,1.38229704228563));
#81796=CARTESIAN_POINT('Ctrl Pts',(-12.3613156359765,1.57894060547886,1.37730827761828));
#81797=CARTESIAN_POINT('Ctrl Pts',(-12.31440242706,1.49464642180646,1.37231951295094));
#81798=CARTESIAN_POINT('Ctrl Pts',(-12.2675225226475,1.41041208004298,1.36733428989451));
#81799=CARTESIAN_POINT('Ctrl Pts',(-12.2245746244422,1.32390744446607,1.36234906683807));
#81800=CARTESIAN_POINT('Ctrl Pts',(-12.1857768784946,1.23553651195931,1.35736384378164));
#81801=CARTESIAN_POINT('Ctrl Pts',(-12.1469931113263,1.14719741938873,1.35238041689482));
#81802=CARTESIAN_POINT('Ctrl Pts',(-12.1123567015251,1.0569937672414,1.34739699000801));
#81803=CARTESIAN_POINT('Ctrl Pts',(-12.0820387614793,0.965351987873125,
1.34241356312119));
#81804=CARTESIAN_POINT('Ctrl Pts',(-12.0517234806571,0.873718246517522,
1.33743057333685));
#81805=CARTESIAN_POINT('Ctrl Pts',(-12.0257260540698,0.780647045298507,
1.33244758355251));
#81806=CARTESIAN_POINT('Ctrl Pts',(-12.0041682162928,0.686581512807936,
1.32746459376817));
#81807=CARTESIAN_POINT('Ctrl Pts',(-11.9826063930718,0.59249859021968,1.32248068276776));
#81808=CARTESIAN_POINT('Ctrl Pts',(-11.9654858866696,0.497421398884258,
1.31749677176736));
#81809=CARTESIAN_POINT('Ctrl Pts',(-11.9528774275583,0.401803781112274,
1.31251286076696));
#81810=CARTESIAN_POINT('Ctrl Pts',(-11.9402554199237,0.306083416644196,
1.30752359426408));
#81811=CARTESIAN_POINT('Ctrl Pts',(-11.9321551962721,0.209821902045561,
1.3025343277612));
#81812=CARTESIAN_POINT('Ctrl Pts',(-11.9285956178948,0.113478507149245,
1.29754506125833));
#81813=CARTESIAN_POINT('Ctrl Pts',(-11.9250339289747,0.017077988392859,
1.29255283652295));
#81814=CARTESIAN_POINT('Ctrl Pts',(-11.9260182415748,-0.0794040688892739,
1.28756061178758));
#81815=CARTESIAN_POINT('Ctrl Pts',(-11.9315152897072,-0.175510206823777,
1.2825683870522));
#81816=CARTESIAN_POINT('Ctrl Pts',(-11.9370211401419,-0.27177023740481,
1.27756816837707));
#81817=CARTESIAN_POINT('Ctrl Pts',(-11.9470541089325,-0.367652710765975,
1.27256794970194));
#81818=CARTESIAN_POINT('Ctrl Pts',(-11.961529277627,-0.462707163637923,
1.26756773102681));
#81819=CARTESIAN_POINT('Ctrl Pts',(-11.9695605154953,-0.515446094532162,
1.26479346660052));
#81820=CARTESIAN_POINT('Ctrl Pts',(-11.9789583085164,-0.567930333086632,
1.26201920217422));
#81821=CARTESIAN_POINT('Ctrl Pts',(-11.9897015145351,-0.620084896129376,
1.25924493774793));
#81822=CARTESIAN_POINT('Ctrl Pts',(-12.0090675753953,-0.714100447936634,
1.254243956325));
#81823=CARTESIAN_POINT('Ctrl Pts',(-12.0328759778584,-0.807371879480203,
1.24924297490208));
#81824=CARTESIAN_POINT('Ctrl Pts',(-12.0610553300471,-0.899447873395274,
1.24424199347916));
#81825=CARTESIAN_POINT('Ctrl Pts',(-12.0891966211125,-0.991399502643214,
1.23924776675269));
#81826=CARTESIAN_POINT('Ctrl Pts',(-12.1216970011,-1.08215848743051,1.23425354002622));
#81827=CARTESIAN_POINT('Ctrl Pts',(-12.1584340584121,-1.17128359059939,
1.22925931329976));
#81828=CARTESIAN_POINT('Ctrl Pts',(-12.1951325533239,-1.26031514033326,
1.22427032894664));
#81829=CARTESIAN_POINT('Ctrl Pts',(-12.2360587183488,-1.34771581454367,
1.21928134459352));
#81830=CARTESIAN_POINT('Ctrl Pts',(-12.2810406288576,-1.43306042722451,
1.2142923602404));
#81831=CARTESIAN_POINT('Ctrl Pts',(-12.3259905879064,-1.51834441809222,
1.20930691965259));
#81832=CARTESIAN_POINT('Ctrl Pts',(-12.3749903613579,-1.60157486384683,
1.20432147906477));
#81833=CARTESIAN_POINT('Ctrl Pts',(-12.4278207005252,-1.68234832937574,
1.19933603847696));
#81834=CARTESIAN_POINT('Ctrl Pts',(-12.480631990839,-1.76309267069424,1.19435239547229));
#81835=CARTESIAN_POINT('Ctrl Pts',(-12.5372708626804,-1.84138142530105,
1.18936875246763));
#81836=CARTESIAN_POINT('Ctrl Pts',(-12.5974735826146,-1.91683829880488,
1.18438510946296));
#81837=CARTESIAN_POINT('Ctrl Pts',(-12.657671002151,-1.9922885288972,1.17940190523067));
#81838=CARTESIAN_POINT('Ctrl Pts',(-12.7214313721858,-2.06490703085392,
1.17441870099837));
#81839=CARTESIAN_POINT('Ctrl Pts',(-12.7884500009607,-2.13434974916232,
1.16943549676608));
#81840=CARTESIAN_POINT('Ctrl Pts',(-12.8554809931549,-2.2038052780797,1.16445137324545));
#81841=CARTESIAN_POINT('Ctrl Pts',(-12.9257711332084,-2.27008354421172,
1.15946724972482));
#81842=CARTESIAN_POINT('Ctrl Pts',(-12.9989788932715,-2.33287736077724,
1.15448312620419));
#81843=CARTESIAN_POINT('Ctrl Pts',(-13.0722652542397,-2.39573859711926,
1.14949365138447));
#81844=CARTESIAN_POINT('Ctrl Pts',(-13.148475155439,-2.455107629182,1.14450417656474));
#81845=CARTESIAN_POINT('Ctrl Pts',(-13.2272341880939,-2.5107177511893,1.13951470174502));
#81846=CARTESIAN_POINT('Ctrl Pts',(-13.306039883813,-2.56636082101982,1.1345222707668));
#81847=CARTESIAN_POINT('Ctrl Pts',(-13.3873973486272,-2.61824031055167,
1.12952983978859));
#81848=CARTESIAN_POINT('Ctrl Pts',(-13.4709052146561,-2.66613416531015,
1.12453740881038));
#81849=CARTESIAN_POINT('Ctrl Pts',(-13.5545467066022,-2.71410465788225,
1.11953698914558));
#81850=CARTESIAN_POINT('Ctrl Pts',(-13.640345080331,-2.75807658150661,1.11453656948078));
#81851=CARTESIAN_POINT('Ctrl Pts',(-13.7278766093667,-2.79787496664945,
1.10953614981599));
#81852=CARTESIAN_POINT('Ctrl Pts',(-13.7764022383554,-2.81993834990194,
1.10676402287938));
#81853=CARTESIAN_POINT('Ctrl Pts',(-13.8254602007446,-2.84071992500492,
1.10399189594279));
#81854=CARTESIAN_POINT('Ctrl Pts',(-13.8749763169397,-2.86019649020019,
1.10121976900618));
#81855=CARTESIAN_POINT('Ctrl Pts',(-13.9643065805911,-2.89533346857428,
1.09621867342054));
#81856=CARTESIAN_POINT('Ctrl Pts',(-14.0554402537431,-2.92634271790657,
1.09121757783489));
#81857=CARTESIAN_POINT('Ctrl Pts',(-14.1479602771984,-2.95303751428391,
1.08621648224925));
#81858=CARTESIAN_POINT('Ctrl Pts',(-14.2403553867585,-2.97969626926316,
1.08122213878392));
#81859=CARTESIAN_POINT('Ctrl Pts',(-14.3341327086799,-3.00205202791187,
1.07622779531858));
#81860=CARTESIAN_POINT('Ctrl Pts',(-14.428855760121,-3.01996630895992,1.07123345185325));
#81861=CARTESIAN_POINT('Ctrl Pts',(-14.5234794295356,-3.0378617946089,1.06624434837931));
#81862=CARTESIAN_POINT('Ctrl Pts',(-14.6190464271741,-3.0513249854539,1.06125524490537));
#81863=CARTESIAN_POINT('Ctrl Pts',(-14.7151066707566,-3.06026764204581,
1.05626614143143));
#81864=CARTESIAN_POINT('Ctrl Pts',(-14.8110987407271,-3.06920395206626,
1.05128057870641));
#81865=CARTESIAN_POINT('Ctrl Pts',(-14.9075829252319,-3.07362606516694,
1.04629501598139));
#81866=CARTESIAN_POINT('Ctrl Pts',(-15.0041015120033,-3.0734972633141,1.04130945325637));
#81867=CARTESIAN_POINT('Ctrl Pts',(-15.1005853333848,-3.07336850785489,
1.0363256862998));
#81868=CARTESIAN_POINT('Ctrl Pts',(-15.1971030942253,-3.06869209506222,
1.03134191934323));
#81869=CARTESIAN_POINT('Ctrl Pts',(-15.2931955178381,-3.05948339402581,
1.02635815238666));
#81870=CARTESIAN_POINT('Ctrl Pts',(-15.3892795132487,-3.05027550067839,
1.02137482255295));
#81871=CARTESIAN_POINT('Ctrl Pts',(-15.4849378090008,-3.03653615152407,
1.01639149271924));
#81872=CARTESIAN_POINT('Ctrl Pts',(-15.579715760275,-3.01833263363878,1.01140816288553));
#81873=CARTESIAN_POINT('Ctrl Pts',(-15.6745112237502,-3.00012575227431,
1.00642391227782));
#81874=CARTESIAN_POINT('Ctrl Pts',(-15.7684255889595,-2.97745314676545,
1.0014396616701));
#81875=CARTESIAN_POINT('Ctrl Pts',(-15.8610149724201,-2.95043309825327,
0.99645541106239));
#81876=CARTESIAN_POINT('Ctrl Pts',(-15.953703790842,-2.92338403197063,0.991465807694484));
#81877=CARTESIAN_POINT('Ctrl Pts',(-16.0450643650687,-2.89197832502405,
0.986476204326578));
#81878=CARTESIAN_POINT('Ctrl Pts',(-16.1346687587719,-2.85638391289878,
0.981486600958672));
#81879=CARTESIAN_POINT('Ctrl Pts',(-16.2243262579988,-2.82076840515736,
0.976494040419932));
#81880=CARTESIAN_POINT('Ctrl Pts',(-16.312225104865,-2.78095942996662,0.971501479881193));
#81881=CARTESIAN_POINT('Ctrl Pts',(-16.3979600378624,-2.73717189495649,
0.966508919342453));
#81882=CARTESIAN_POINT('Ctrl Pts',(-16.4838321619879,-2.6933142921092,0.961508369819661));
#81883=CARTESIAN_POINT('Ctrl Pts',(-16.5675330778827,-2.64546563514151,
0.956507820296869));
#81884=CARTESIAN_POINT('Ctrl Pts',(-16.6486847501473,-2.5938852797747,0.951507270774077));
#81885=CARTESIAN_POINT('Ctrl Pts',(-16.6936522821998,-2.5653037210894,0.948736380604204));
#81886=CARTESIAN_POINT('Ctrl Pts',(-16.7378376294089,-2.53557710926649,
0.945965490434332));
#81887=CARTESIAN_POINT('Ctrl Pts',(-16.7811809181293,-2.50475483568596,
0.943194600264459));
#81888=CARTESIAN_POINT('Ctrl Pts',(-16.8588974660735,-2.44948905468059,
0.938226264333042));
#81889=CARTESIAN_POINT('Ctrl Pts',(-16.9341838418177,-2.39049999289044,
0.933257928401624));
#81890=CARTESIAN_POINT('Ctrl Pts',(-17.0066586192695,-2.32802994733994,
0.928289592470207));
#81891=CARTESIAN_POINT('Ctrl Pts',(-17.0790351989641,-2.26564454390325,
0.923327988252394));
#81892=CARTESIAN_POINT('Ctrl Pts',(-17.1486074151297,-2.19978781560031,
0.918366384034581));
#81893=CARTESIAN_POINT('Ctrl Pts',(-17.2150233744915,-2.13074486986504,
0.913404779816767));
#81894=CARTESIAN_POINT('Ctrl Pts',(-17.2829729916507,-2.06010760473582,
0.90832860369381));
#81895=CARTESIAN_POINT('Ctrl Pts',(-17.3476183845453,-1.98613540779927,
0.903252427570853));
#81896=CARTESIAN_POINT('Ctrl Pts',(-17.4086190435062,-1.90917693084204,
0.898176251447896));
#81897=CARTESIAN_POINT('Ctrl Pts',(-17.4681388199416,-1.83408673638613,
0.893223307116927));
#81898=CARTESIAN_POINT('Ctrl Pts',(-17.5241885178778,-1.75615397477629,
0.888270362785958));
#81899=CARTESIAN_POINT('Ctrl Pts',(-17.5764905960058,-1.67573818321774,
0.883317418454989));
#81900=CARTESIAN_POINT('Ctrl Pts',(-17.6287754491663,-1.59534887549015,
0.87836610530787));
#81901=CARTESIAN_POINT('Ctrl Pts',(-17.6773148918573,-1.51247853509114,
0.873414792160749));
#81902=CARTESIAN_POINT('Ctrl Pts',(-17.7218742095594,-1.42751638776421,
0.868463479013631));
#81903=CARTESIAN_POINT('Ctrl Pts',(-17.7664314111598,-1.34255827525095,
0.863512401002118));
#81904=CARTESIAN_POINT('Ctrl Pts',(-17.8070086575104,-1.25550894786147,
0.858561322990605));
#81905=CARTESIAN_POINT('Ctrl Pts',(-17.8434173326361,-1.16678195155079,
0.853610244979092));
#81906=CARTESIAN_POINT('Ctrl Pts',(-17.8814320258966,-1.07414113072894,
0.848440770636316));
#81907=CARTESIAN_POINT('Ctrl Pts',(-17.914901702574,-0.979671707568172,
0.843271296293546));
#81908=CARTESIAN_POINT('Ctrl Pts',(-17.9436684417483,-0.88386557521798,
0.838101821950771));
#81909=CARTESIAN_POINT('Ctrl Pts',(-17.9712565102632,-0.791984944347023,
0.833144158466879));
#81910=CARTESIAN_POINT('Ctrl Pts',(-17.9945194094835,-0.698875450581568,
0.828186494982984));
#81911=CARTESIAN_POINT('Ctrl Pts',(-18.0133698527397,-0.604982958933142,
0.823228831499092));
#81912=CARTESIAN_POINT('Ctrl Pts',(-18.0322328518359,-0.511027927688841,
0.818267865831338));
#81913=CARTESIAN_POINT('Ctrl Pts',(-18.0466774803284,-0.416289299842081,
0.813306900163584));
#81914=CARTESIAN_POINT('Ctrl Pts',(-18.0566682323481,-0.321218877642427,
0.808345934495829));
#81915=CARTESIAN_POINT('Ctrl Pts',(-18.066673516729,-0.226010167783542,
0.803377752700137));
#81916=CARTESIAN_POINT('Ctrl Pts',(-18.0722119787107,-0.130469143381661,
0.798409570904445));
#81917=CARTESIAN_POINT('Ctrl Pts',(-18.0733001629596,-0.035047943623454,
0.793441389108753));
#81918=CARTESIAN_POINT('Ctrl Pts',(-18.0734363150779,-0.0231089741993823,
0.792819777027766));
#81919=CARTESIAN_POINT('Ctrl Pts',(-18.0735028661208,-0.0111718734142489,
0.79219816494678));
#81920=CARTESIAN_POINT('Ctrl Pts',(-18.0734999054211,0.000762480339109222,
0.791576552865792));
#81921=CARTESIAN_POINT('Origin',(-15.,0.,8.20842344717746));
#81922=CARTESIAN_POINT('',(-13.1276888212995,2.43738653071547,2.43734746082558));
#81923=CARTESIAN_POINT('',(-13.1254325828889,2.44028101900739,2.35408149450477));
#81924=CARTESIAN_POINT('',(-13.1276888212995,2.43738653071547,8.20842344717746));
#81925=CARTESIAN_POINT('',(-18.073498904786,-0.00259466362292773,1.70842344717746));
#81926=CARTESIAN_POINT('Ctrl Pts',(-13.1254325828889,2.44028101900739,2.35408149450477));
#81927=CARTESIAN_POINT('Ctrl Pts',(-12.4084487444517,1.88105036108211,2.30683845046461));
#81928=CARTESIAN_POINT('Ctrl Pts',(-11.4280462758325,-0.0162669500815165,
2.20692035017721));
#81929=CARTESIAN_POINT('Ctrl Pts',(-12.9443038197492,-2.98822585588414,
2.05432719364256));
#81930=CARTESIAN_POINT('Ctrl Pts',(-16.3800295351377,-3.35423238380087,
1.89630202490083));
#81931=CARTESIAN_POINT('Ctrl Pts',(-17.9731131493935,-1.40035444911347,
1.78100077607913));
#81932=CARTESIAN_POINT('Ctrl Pts',(-18.076577770913,-0.194497574487465,
1.71837458350467));
#81933=CARTESIAN_POINT('Ctrl Pts',(-18.0748543381996,-0.00259580788680448,
1.70842344717746));
#81934=CARTESIAN_POINT('Ctrl Pts',(-18.073498904786,-0.00259466362292773,
1.70842344717746));
#81935=CARTESIAN_POINT('Ctrl Pts',(-18.0735789633664,0.0922384226565076,
1.70350363328471));
#81936=CARTESIAN_POINT('Ctrl Pts',(-18.0692656912357,0.187216825807511,
1.69858381939197));
#81937=CARTESIAN_POINT('Ctrl Pts',(-18.0605453982257,0.281893801634021,
1.69366400549922));
#81938=CARTESIAN_POINT('Ctrl Pts',(-18.0518336958937,0.376477507725467,
1.68874903829421));
#81939=CARTESIAN_POINT('Ctrl Pts',(-18.0387236414728,0.47075992793125,1.68383407108921));
#81940=CARTESIAN_POINT('Ctrl Pts',(-18.0212535976478,0.564295090090703,
1.6789191038842));
#81941=CARTESIAN_POINT('Ctrl Pts',(-18.0037927532641,0.657780998152678,
1.67400672482112));
#81942=CARTESIAN_POINT('Ctrl Pts',(-17.9819765600055,0.750519985203623,
1.66909434575803));
#81943=CARTESIAN_POINT('Ctrl Pts',(-17.9558950091817,0.842073004373502,
1.66418196669494));
#81944=CARTESIAN_POINT('Ctrl Pts',(-17.9298195878756,0.933604507343941,
1.65927074210746));
#81945=CARTESIAN_POINT('Ctrl Pts',(-17.899480924029,1.02395016074908,1.65435951751998));
#81946=CARTESIAN_POINT('Ctrl Pts',(-17.8650194238835,1.11268411994169,1.64944829293251));
#81947=CARTESIAN_POINT('Ctrl Pts',(-17.8305559748702,1.20142309721957,1.64453679060532));
#81948=CARTESIAN_POINT('Ctrl Pts',(-17.7919693921325,1.28854977782556,1.63962528827814));
#81949=CARTESIAN_POINT('Ctrl Pts',(-17.7494485017389,1.37365759426636,1.63471378595096));
#81950=CARTESIAN_POINT('Ctrl Pts',(-17.7068863483411,1.45884800079765,1.62979751741735));
#81951=CARTESIAN_POINT('Ctrl Pts',(-17.6603824677528,1.54201522605512,1.62488124888374));
#81952=CARTESIAN_POINT('Ctrl Pts',(-17.6101718132093,1.62277705046865,1.61996498035013));
#81953=CARTESIAN_POINT('Ctrl Pts',(-17.5599354305212,1.70358025757101,1.61504619270044));
#81954=CARTESIAN_POINT('Ctrl Pts',(-17.5059887511946,1.78197523848825,1.61012740505074));
#81955=CARTESIAN_POINT('Ctrl Pts',(-17.4486089501875,1.85761041638489,1.60520861740105));
#81956=CARTESIAN_POINT('Ctrl Pts',(-17.391136305883,1.93336797566299,1.60028187091468));
#81957=CARTESIAN_POINT('Ctrl Pts',(-17.3302197396758,2.00635646943507,1.59535512442832));
#81958=CARTESIAN_POINT('Ctrl Pts',(-17.2661752905315,2.07625908850132,1.59042837794195));
#81959=CARTESIAN_POINT('Ctrl Pts',(-17.2220785395579,2.12438938592067,1.58703614776709));
#81960=CARTESIAN_POINT('Ctrl Pts',(-17.1764997129828,2.1710575011714,1.58364391759222));
#81961=CARTESIAN_POINT('Ctrl Pts',(-17.129551019269,2.21617118163968,1.58025168741735));
#81962=CARTESIAN_POINT('Ctrl Pts',(-17.0603370994175,2.28267984071285,1.57525070594442));
#81963=CARTESIAN_POINT('Ctrl Pts',(-16.9878837377594,2.34605894210612,1.57024972447148));
#81964=CARTESIAN_POINT('Ctrl Pts',(-16.9125054133723,2.40597699361855,1.56524874299855));
#81965=CARTESIAN_POINT('Ctrl Pts',(-16.8372289005508,2.46581411535857,1.56025451622278));
#81966=CARTESIAN_POINT('Ctrl Pts',(-16.7590356173462,2.52219920752529,1.555260289447));
#81967=CARTESIAN_POINT('Ctrl Pts',(-16.6782763784391,2.57483798472318,1.55026606267123));
#81968=CARTESIAN_POINT('Ctrl Pts',(-16.5976019114416,2.62742150768985,1.54527707826953));
#81969=CARTESIAN_POINT('Ctrl Pts',(-16.5143672088258,2.67626629507595,1.54028809386783));
#81970=CARTESIAN_POINT('Ctrl Pts',(-16.4289547970201,2.7211193355076,1.53529910946614));
#81971=CARTESIAN_POINT('Ctrl Pts',(-16.3436030552084,2.76594051600651,1.53031366883106));
#81972=CARTESIAN_POINT('Ctrl Pts',(-16.2560770666207,2.80677538294738,1.52532822819598));
#81973=CARTESIAN_POINT('Ctrl Pts',(-16.1667860369241,2.84341565622033,1.5203427875609));
#81974=CARTESIAN_POINT('Ctrl Pts',(-16.0775272026012,2.88004271823016,1.5153591445098));
#81975=CARTESIAN_POINT('Ctrl Pts',(-15.9865049971013,2.91247802533915,1.51037550145869));
#81976=CARTESIAN_POINT('Ctrl Pts',(-15.8941499124283,2.94056086216633,1.50539185840759));
#81977=CARTESIAN_POINT('Ctrl Pts',(-15.8018029589437,2.96864122650556,1.50040865412972));
#81978=CARTESIAN_POINT('Ctrl Pts',(-15.7081237793487,2.99236975505983,1.49542544985186));
#81979=CARTESIAN_POINT('Ctrl Pts',(-15.6135583580429,3.0116355010651,1.490442245574));
#81980=CARTESIAN_POINT('Ctrl Pts',(-15.5189754915764,3.03090480116058,1.48545812200874));
#81981=CARTESIAN_POINT('Ctrl Pts',(-15.4235064885192,3.04570959611494,1.48047399844347));
#81982=CARTESIAN_POINT('Ctrl Pts',(-15.3276068059865,3.05599018824854,1.47548987487821));
#81983=CARTESIAN_POINT('Ctrl Pts',(-15.2316041589666,3.0662818183321,1.4705004000155));
#81984=CARTESIAN_POINT('Ctrl Pts',(-15.1351703461965,3.07203950146474,1.46551092515279));
#81985=CARTESIAN_POINT('Ctrl Pts',(-15.0387649919052,3.07325552556285,1.46052145029008));
#81986=CARTESIAN_POINT('Ctrl Pts',(-14.9423025194942,3.07447227012934,1.45552901926975));
#81987=CARTESIAN_POINT('Ctrl Pts',(-14.8458689772977,3.07114201283781,1.45053658824942));
#81988=CARTESIAN_POINT('Ctrl Pts',(-14.749920914246,3.06330910958533,1.44554415722909));
#81989=CARTESIAN_POINT('Ctrl Pts',(-14.6538193190112,3.05546367244005,1.44054373752395));
#81990=CARTESIAN_POINT('Ctrl Pts',(-14.5582051887255,3.04310125939591,1.43554331781881));
#81991=CARTESIAN_POINT('Ctrl Pts',(-14.4635268272169,3.02631769397796,1.43054289811367));
#81992=CARTESIAN_POINT('Ctrl Pts',(-14.4110391544942,3.01701324178062,1.42777077163432));
#81993=CARTESIAN_POINT('Ctrl Pts',(-14.3588388540241,3.00635091370299,1.42499864515497));
#81994=CARTESIAN_POINT('Ctrl Pts',(-14.3070001997571,2.9943536075192,1.42222651867561));
#81995=CARTESIAN_POINT('Ctrl Pts',(-14.2134709796855,2.97270762333628,1.41722494540526));
#81996=CARTESIAN_POINT('Ctrl Pts',(-14.1207938463946,2.94663759779816,1.41222337213489));
#81997=CARTESIAN_POINT('Ctrl Pts',(-14.0294183957941,2.91622591710196,1.40722179886454));
#81998=CARTESIAN_POINT('Ctrl Pts',(-13.9381896884165,2.88586307565098,1.40222825780607));
#81999=CARTESIAN_POINT('Ctrl Pts',(-13.8482589179546,2.85117258671998,1.39723471674761));
#82000=CARTESIAN_POINT('Ctrl Pts',(-13.7600640209766,2.81228750627017,1.39224117568915));
#82001=CARTESIAN_POINT('Ctrl Pts',(-13.6719511175242,2.77343857671967,1.38725227705389));
#82002=CARTESIAN_POINT('Ctrl Pts',(-13.5855712807978,2.7304029780461,1.38226337841863));
#82003=CARTESIAN_POINT('Ctrl Pts',(-13.5013453567284,2.68336291064037,1.37727447978338));
#82004=CARTESIAN_POINT('Ctrl Pts',(-13.4171795407834,2.63635641354282,1.37228914149303));
#82005=CARTESIAN_POINT('Ctrl Pts',(-13.3351649633428,2.58535134241823,1.36730380320269));
#82006=CARTESIAN_POINT('Ctrl Pts',(-13.2556995740404,2.53057666827089,1.36231846491235));
#82007=CARTESIAN_POINT('Ctrl Pts',(-13.2122469812482,2.50062524373329,1.35959242434849));
#82008=CARTESIAN_POINT('Ctrl Pts',(-13.169556182852,2.46954750644487,1.35686638378463));
#82009=CARTESIAN_POINT('Ctrl Pts',(-13.1276888212995,2.43738653071547,1.35414034322078));
#82010=CARTESIAN_POINT('',(-18.0734993815183,0.00194982225149054,1.79157655278713));
#82011=CARTESIAN_POINT('Ctrl Pts',(-18.0734993815183,0.00194982225148788,
1.79157655278713));
#82012=CARTESIAN_POINT('Ctrl Pts',(-18.0734301645551,0.111056328367583,
1.78594824754486));
#82013=CARTESIAN_POINT('Ctrl Pts',(-18.0675471115686,0.21994398135138,1.78031994230258));
#82014=CARTESIAN_POINT('Ctrl Pts',(-18.0559442096784,0.328035420851308,
1.77469163706031));
#82015=CARTESIAN_POINT('Ctrl Pts',(-18.0442899661858,0.436605153433593,
1.76903842716809));
#82016=CARTESIAN_POINT('Ctrl Pts',(-18.0268652646068,0.544371409516094,
1.76338521727588));
#82017=CARTESIAN_POINT('Ctrl Pts',(-18.0038150252988,0.650766888977212,
1.75773200738366));
#82018=CARTESIAN_POINT('Ctrl Pts',(-17.9806384718765,0.757745410140075,
1.75204781819484));
#82019=CARTESIAN_POINT('Ctrl Pts',(-17.9517746673911,0.863337893675431,
1.74636362900601));
#82020=CARTESIAN_POINT('Ctrl Pts',(-17.9174192949469,0.966988576701586,
1.74067943981719));
#82021=CARTESIAN_POINT('Ctrl Pts',(-17.9025933139296,1.01171878771819,1.73822644120251));
#82022=CARTESIAN_POINT('Ctrl Pts',(-17.886745218295,1.05608765124302,1.73577344258782));
#82023=CARTESIAN_POINT('Ctrl Pts',(-17.8698934155499,1.10005183213486,1.73332044397313));
#82024=CARTESIAN_POINT('Ctrl Pts',(-17.8355379352173,1.18968085134503,1.72831955789956));
#82025=CARTESIAN_POINT('Ctrl Pts',(-17.7969197229677,1.27785526329013,1.72331867182598));
#82026=CARTESIAN_POINT('Ctrl Pts',(-17.7541824063681,1.36414131322687,1.71831778575241));
#82027=CARTESIAN_POINT('Ctrl Pts',(-17.711502810146,1.45031082652141,1.7133236538004));
#82028=CARTESIAN_POINT('Ctrl Pts',(-17.6647153593443,1.53459665687628,1.7083295218484));
#82029=CARTESIAN_POINT('Ctrl Pts',(-17.6140123914159,1.61658326959187,1.70333538989639));
#82030=CARTESIAN_POINT('Ctrl Pts',(-17.5633626396951,1.69848383179036,1.69834649962498));
#82031=CARTESIAN_POINT('Ctrl Pts',(-17.5088057701728,1.77808960258467,1.69335760935357));
#82032=CARTESIAN_POINT('Ctrl Pts',(-17.4505803751013,1.85500891511829,1.68836871908216));
#82033=CARTESIAN_POINT('Ctrl Pts',(-17.3923963229419,1.93187361113333,1.68338337116974));
#82034=CARTESIAN_POINT('Ctrl Pts',(-17.330549187613,2.00605529222922,1.67839802325732));
#82035=CARTESIAN_POINT('Ctrl Pts',(-17.2653207318563,2.077191428786,1.6734126753449));
#82036=CARTESIAN_POINT('Ctrl Pts',(-17.2001157839113,2.1483019284503,1.66842912411184));
#82037=CARTESIAN_POINT('Ctrl Pts',(-17.1315322330067,2.21636874143207,1.66344557287878));
#82038=CARTESIAN_POINT('Ctrl Pts',(-17.0598913363535,2.28106333371431,1.65846202164572));
#82039=CARTESIAN_POINT('Ctrl Pts',(-16.9882567327318,2.34575224313761,1.65347890817443));
#82040=CARTESIAN_POINT('Ctrl Pts',(-16.9135656430403,2.40706922698091,1.64849579470313));
#82041=CARTESIAN_POINT('Ctrl Pts',(-16.8361745122614,2.46472420577267,1.64351268123183));
#82042=CARTESIAN_POINT('Ctrl Pts',(-16.7587690869431,2.52238983373514,1.63852864735388));
#82043=CARTESIAN_POINT('Ctrl Pts',(-16.6786629818744,2.57639185127706,1.63354461347593));
#82044=CARTESIAN_POINT('Ctrl Pts',(-16.5962430110992,2.62648253364017,1.62856057959798));
#82045=CARTESIAN_POINT('Ctrl Pts',(-16.5137345100379,2.67662702022576,1.6235711921881));
#82046=CARTESIAN_POINT('Ctrl Pts',(-16.4289075569818,2.72285155613003,1.61858180477821));
#82047=CARTESIAN_POINT('Ctrl Pts',(-16.3421748464228,2.7649536943012,1.61359241736833));
#82048=CARTESIAN_POINT('Ctrl Pts',(-16.2553907279245,2.80708078711923,1.60860007266444));
#82049=CARTESIAN_POINT('Ctrl Pts',(-16.1666990057432,2.84508044425425,1.60360772796055));
#82050=CARTESIAN_POINT('Ctrl Pts',(-16.0765317345408,2.87879865126525,1.59861538325666));
#82051=CARTESIAN_POINT('Ctrl Pts',(-15.98622013161,2.91257083137568,1.59361504725249));
#82052=CARTESIAN_POINT('Ctrl Pts',(-15.8944286809185,2.94204774322958,1.58861471124831));
#82053=CARTESIAN_POINT('Ctrl Pts',(-15.8016038631026,2.9671254602155,1.58361437524414));
#82054=CARTESIAN_POINT('Ctrl Pts',(-15.7501260595822,2.9810327946775,1.58084134190656));
#82055=CARTESIAN_POINT('Ctrl Pts',(-15.6983306289836,2.99358808105795,1.57806830856899));
#82056=CARTESIAN_POINT('Ctrl Pts',(-15.646294608805,3.00478044599428,1.57529527523141));
#82057=CARTESIAN_POINT('Ctrl Pts',(-15.5524441428783,3.02496662972798,1.57029392290144));
#82058=CARTESIAN_POINT('Ctrl Pts',(-15.457483318007,3.04078686615163,1.56529257057148));
#82059=CARTESIAN_POINT('Ctrl Pts',(-15.3618540344134,3.05212449087169,1.56029121824152));
#82060=CARTESIAN_POINT('Ctrl Pts',(-15.2639515952095,3.0637316165675,1.55517098128041));
#82061=CARTESIAN_POINT('Ctrl Pts',(-15.1653489425364,3.07064013593149,1.55005074431929));
#82062=CARTESIAN_POINT('Ctrl Pts',(-15.0665345243961,3.07277975244946,1.54493050735818));
#82063=CARTESIAN_POINT('Ctrl Pts',(-14.970264993654,3.07486426483166,1.53994213806135));
#82064=CARTESIAN_POINT('Ctrl Pts',(-14.873794943287,3.072422506583,1.53495376876452));
#82065=CARTESIAN_POINT('Ctrl Pts',(-14.7775827112181,3.06544169731719,1.5299653994677));
#82066=CARTESIAN_POINT('Ctrl Pts',(-14.6814337557568,3.05846547917165,1.52498031090847));
#82067=CARTESIAN_POINT('Ctrl Pts',(-14.5855427178046,3.04695617374525,1.51999522234924));
#82068=CARTESIAN_POINT('Ctrl Pts',(-14.4903670173818,3.03095306348146,1.51501013379001));
#82069=CARTESIAN_POINT('Ctrl Pts',(-14.3952279716976,3.01495611644863,1.51002696512332));
#82070=CARTESIAN_POINT('Ctrl Pts',(-14.3008041478561,2.994468878059,1.50504379645664));
#82071=CARTESIAN_POINT('Ctrl Pts',(-14.2075458682047,2.96958224317842,1.50006062778995));
#82072=CARTESIAN_POINT('Ctrl Pts',(-14.1098318279932,2.9435065569172,1.49483936973869));
#82073=CARTESIAN_POINT('Ctrl Pts',(-14.0133979870556,2.91260071370465,1.48961811168742));
#82074=CARTESIAN_POINT('Ctrl Pts',(-13.9187468951899,2.87702867092744,1.48439685363615));
#82075=CARTESIAN_POINT('Ctrl Pts',(-13.8283716120819,2.843063574769,1.47941146292103));
#82076=CARTESIAN_POINT('Ctrl Pts',(-13.7396219250735,2.80484491284714,1.47442607220591));
#82077=CARTESIAN_POINT('Ctrl Pts',(-13.6529153365808,2.76256496024635,1.46944068149079));
#82078=CARTESIAN_POINT('Ctrl Pts',(-13.5661780948845,2.72027006049997,1.46445352830064));
#82079=CARTESIAN_POINT('Ctrl Pts',(-13.4814857768715,2.67391121750432,1.45946637511049));
#82080=CARTESIAN_POINT('Ctrl Pts',(-13.399230810013,2.62372640539905,1.45447922192034));
#82081=CARTESIAN_POINT('Ctrl Pts',(-13.3168923970172,2.57349068173336,1.44948700935584));
#82082=CARTESIAN_POINT('Ctrl Pts',(-13.2369966334426,2.51942148722912,1.44449479679134));
#82083=CARTESIAN_POINT('Ctrl Pts',(-13.1599060793514,2.46179946648623,1.43950258422684));
#82084=CARTESIAN_POINT('Ctrl Pts',(-13.1491117351832,2.45373113787068,1.4388035665428));
#82085=CARTESIAN_POINT('Ctrl Pts',(-13.1383723355347,2.44559321557167,1.43810454885877));
#82086=CARTESIAN_POINT('Ctrl Pts',(-13.1276888212995,2.43738653071547,1.43740553117474));
#82087=CARTESIAN_POINT('Ctrl Pts',(-13.1276888212995,2.43738653071547,2.43734746082558));
#82088=CARTESIAN_POINT('Ctrl Pts',(-13.0511401214871,2.37858461950126,2.43236378975877));
#82089=CARTESIAN_POINT('Ctrl Pts',(-12.9773761852912,2.3161823609361,2.42738011869197));
#82090=CARTESIAN_POINT('Ctrl Pts',(-12.9067421325381,2.25048300378137,2.42239644762517));
#82091=CARTESIAN_POINT('Ctrl Pts',(-12.8360348813808,2.18471556207091,2.41740761195638));
#82092=CARTESIAN_POINT('Ctrl Pts',(-12.7684643130332,2.11564449755975,2.41241877628759));
#82093=CARTESIAN_POINT('Ctrl Pts',(-12.7043392668803,2.0436105422542,2.4074299406188));
#82094=CARTESIAN_POINT('Ctrl Pts',(-12.6401800993334,1.97153825716767,2.402438450355));
#82095=CARTESIAN_POINT('Ctrl Pts',(-12.5794703816786,1.89650028227443,2.39744696009119));
#82096=CARTESIAN_POINT('Ctrl Pts',(-12.5224777998822,1.81886942849767,2.39245546982739));
#82097=CARTESIAN_POINT('Ctrl Pts',(-12.4653897842713,1.74110858221558,2.38745562133625));
#82098=CARTESIAN_POINT('Ctrl Pts',(-12.4120315817031,1.66074654935091,2.3824557728451));
#82099=CARTESIAN_POINT('Ctrl Pts',(-12.3626268417748,1.5781841065837,2.37745592435396));
#82100=CARTESIAN_POINT('Ctrl Pts',(-12.3229872118532,1.51194057040738,2.37344432254933));
#82101=CARTESIAN_POINT('Ctrl Pts',(-12.2858918067237,1.44428108992528,2.36943272074471));
#82102=CARTESIAN_POINT('Ctrl Pts',(-12.2514338178258,1.37542218689698,2.36542111894008));
#82103=CARTESIAN_POINT('Ctrl Pts',(-12.2084783871509,1.2895824751208,2.36042024428879));
#82104=CARTESIAN_POINT('Ctrl Pts',(-12.1694731270101,1.20157879356472,2.3554193696375));
#82105=CARTESIAN_POINT('Ctrl Pts',(-12.1346411926523,1.11180985566544,2.3504184949862));
#82106=CARTESIAN_POINT('Ctrl Pts',(-12.0998563011424,1.02216215669733,2.34542437434929));
#82107=CARTESIAN_POINT('Ctrl Pts',(-12.0692336906521,0.930754345222873,
2.34043025371238));
#82108=CARTESIAN_POINT('Ctrl Pts',(-12.0429501984913,0.83800878360397,2.33543613307547));
#82109=CARTESIAN_POINT('Ctrl Pts',(-12.0166942920677,0.74536056272929,2.33044725399849));
#82110=CARTESIAN_POINT('Ctrl Pts',(-11.9947685694811,0.651377802730684,
2.32545837492152));
#82111=CARTESIAN_POINT('Ctrl Pts',(-11.977301039206,0.556500891656688,2.32046949584454));
#82112=CARTESIAN_POINT('Ctrl Pts',(-11.9598459109866,0.461691343782987,
2.31548415890291));
#82113=CARTESIAN_POINT('Ctrl Pts',(-11.94684276163,0.365989337112503,2.31049882196128));
#82114=CARTESIAN_POINT('Ctrl Pts',(-11.9383689637715,0.269847453207505,
2.30551348501965));
#82115=CARTESIAN_POINT('Ctrl Pts',(-11.9298982195667,0.173740215398392,
2.30052994461512));
#82116=CARTESIAN_POINT('Ctrl Pts',(-11.9259536222082,0.0771938518569984,
2.29554640421059));
#82117=CARTESIAN_POINT('Ctrl Pts',(-11.9265608041214,-0.0193328538229716,
2.29056286380607));
#82118=CARTESIAN_POINT('Ctrl Pts',(-11.9271679327176,-0.115851083445451,
2.28557976100868));
#82119=CARTESIAN_POINT('Ctrl Pts',(-11.9323260429192,-0.212349219977606,
2.28059665821128));
#82120=CARTESIAN_POINT('Ctrl Pts',(-11.9420086429596,-0.3083684650972,2.27561355541389));
#82121=CARTESIAN_POINT('Ctrl Pts',(-11.9516930317545,-0.404405448722155,
2.27062953204276));
#82122=CARTESIAN_POINT('Ctrl Pts',(-11.9659035263656,-0.499962928787207,
2.26564550867162));
#82123=CARTESIAN_POINT('Ctrl Pts',(-11.9845618847413,-0.594588280279178,
2.26066148530049));
#82124=CARTESIAN_POINT('Ctrl Pts',(-12.0032402859632,-0.689315278514189,
2.25567210808142));
#82125=CARTESIAN_POINT('Ctrl Pts',(-12.0263760043518,-0.783107718157338,
2.25068273086235));
#82126=CARTESIAN_POINT('Ctrl Pts',(-12.0538399197974,-0.875524432452098,
2.24569335364328));
#82127=CARTESIAN_POINT('Ctrl Pts',(-12.0813201145038,-0.96799592683787,
2.24070101896635));
#82128=CARTESIAN_POINT('Ctrl Pts',(-12.1131334701694,-1.05908965821645,
2.23570868428941));
#82129=CARTESIAN_POINT('Ctrl Pts',(-12.1491020608473,-1.14838285886504,
2.23071634961248));
#82130=CARTESIAN_POINT('Ctrl Pts',(-12.1851282294996,-1.23781899871455,
2.22571602328194));
#82131=CARTESIAN_POINT('Ctrl Pts',(-12.2253227317514,-1.32544845441526,
2.2207156969514));
#82132=CARTESIAN_POINT('Ctrl Pts',(-12.2694609442956,-1.41087161544655,
2.21571537062085));
#82133=CARTESIAN_POINT('Ctrl Pts',(-12.2939396364568,-1.45824660282806,
2.21294223048002));
#82134=CARTESIAN_POINT('Ctrl Pts',(-12.3196305078895,-1.50494347668573,
2.21016909033918));
#82135=CARTESIAN_POINT('Ctrl Pts',(-12.3464895870466,-1.55089804253787,
2.20739595019835));
#82136=CARTESIAN_POINT('Ctrl Pts',(-12.394925277042,-1.6337691302794,2.20239507301304));
#82137=CARTESIAN_POINT('Ctrl Pts',(-12.4473313701558,-1.71451358993703,
2.19739419582773));
#82138=CARTESIAN_POINT('Ctrl Pts',(-12.5034957991935,-1.79272670124466,
2.19239331864242));
#82139=CARTESIAN_POINT('Ctrl Pts',(-12.559584374276,-1.87083418032301,2.18739919548845));
#82140=CARTESIAN_POINT('Ctrl Pts',(-12.619420943369,-1.94641675244406,2.18240507233449));
#82141=CARTESIAN_POINT('Ctrl Pts',(-12.6827483288791,-2.01909557542172,
2.17741094918052));
#82142=CARTESIAN_POINT('Ctrl Pts',(-12.7460092491569,-2.09169811836956,
2.17242206760653));
#82143=CARTESIAN_POINT('Ctrl Pts',(-12.8127534156523,-2.16140264180255,
2.16743318603254));
#82144=CARTESIAN_POINT('Ctrl Pts',(-12.8826818788696,-2.22786135653291,
2.16244430445855));
#82145=CARTESIAN_POINT('Ctrl Pts',(-12.9525606919073,-2.29427288465337,
2.15745896505973));
#82146=CARTESIAN_POINT('Ctrl Pts',(-13.0256189899682,-2.35744288417238,
2.1524736256609));
#82147=CARTESIAN_POINT('Ctrl Pts',(-13.1015199496688,-2.41705931836488,
2.14748828626208));
#82148=CARTESIAN_POINT('Ctrl Pts',(-13.1773935570037,-2.47665426863257,
2.14250474342586));
#82149=CARTESIAN_POINT('Ctrl Pts',(-13.2561074459012,-2.53269792735683,
2.13752120058965));
#82150=CARTESIAN_POINT('Ctrl Pts',(-13.337291334359,-2.58491820822289,2.13253765775343));
#82151=CARTESIAN_POINT('Ctrl Pts',(-13.4184680935616,-2.63713390330583,
2.12755455255268));
#82152=CARTESIAN_POINT('Ctrl Pts',(-13.5021140520083,-2.68552665096215,
2.12257144735193));
#82153=CARTESIAN_POINT('Ctrl Pts',(-13.5878304418918,-2.72986801680091,
2.11758834215118));
#82154=CARTESIAN_POINT('Ctrl Pts',(-13.6735626663974,-2.77421757394089,
2.11260431640783));
#82155=CARTESIAN_POINT('Ctrl Pts',(-13.7613656923181,-2.81451406135458,
2.10762029066449));
#82156=CARTESIAN_POINT('Ctrl Pts',(-13.8508176534763,-2.85057576367272,
2.10263626492115));
#82157=CARTESIAN_POINT('Ctrl Pts',(-13.9403657029619,-2.88667620308076,
2.09764688539135));
#82158=CARTESIAN_POINT('Ctrl Pts',(-14.0315658162599,-2.91853261176117,
2.09265750586156));
#82159=CARTESIAN_POINT('Ctrl Pts',(-14.1239779320351,-2.94601214974386,
2.08766812633176));
#82160=CARTESIAN_POINT('Ctrl Pts',(-14.2164448245683,-2.97350797606701,
2.08267578937552));
#82161=CARTESIAN_POINT('Ctrl Pts',(-14.3101247243823,-2.99662166081349,
2.07768345241928));
#82162=CARTESIAN_POINT('Ctrl Pts',(-14.4045663206393,-3.01527129517112,
2.07269111546304));
#82163=CARTESIAN_POINT('Ctrl Pts',(-14.4991590961543,-3.03395078330078,
2.06769078692442));
#82164=CARTESIAN_POINT('Ctrl Pts',(-14.5945155691579,-3.04815188821779,
2.0626904583858));
#82165=CARTESIAN_POINT('Ctrl Pts',(-14.6901783166036,-3.05784446538693,
2.05769012984717));
#82166=CARTESIAN_POINT('Ctrl Pts',(-14.7432316121923,-3.06321984060142,
2.05491701371699));
#82167=CARTESIAN_POINT('Ctrl Pts',(-14.7963790757514,-3.06720947326471,
2.0521438975868));
#82168=CARTESIAN_POINT('Ctrl Pts',(-14.8495429191303,-3.06981512746552,
2.04937078145661));
#82169=CARTESIAN_POINT('Ctrl Pts',(-14.945415621551,-3.07451401855257,2.04436989888999));
#82170=CARTESIAN_POINT('Ctrl Pts',(-15.0416759073252,-3.07472553622459,
2.03936901632337));
#82171=CARTESIAN_POINT('Ctrl Pts',(-15.1378689317255,-3.07040622844354,
2.03436813375675));
#82172=CARTESIAN_POINT('Ctrl Pts',(-15.2339320418076,-3.06609275414083,
2.02937400517518));
#82173=CARTESIAN_POINT('Ctrl Pts',(-15.3299276365342,-3.05726063553923,
2.02437987659362));
#82174=CARTESIAN_POINT('Ctrl Pts',(-15.4253979050383,-3.0439183419384,2.01938574801205));
#82175=CARTESIAN_POINT('Ctrl Pts',(-15.5207679736017,-3.0305900516189,2.01439686097213));
#82176=CARTESIAN_POINT('Ctrl Pts',(-15.6156133798509,-3.01276105702709,
2.00940797393221));
#82177=CARTESIAN_POINT('Ctrl Pts',(-15.7094795050446,-2.99049177927672,
2.00441908689228));
#82178=CARTESIAN_POINT('Ctrl Pts',(-15.8032789847001,-2.96823831285338,
1.99943374199349));
#82179=CARTESIAN_POINT('Ctrl Pts',(-15.8961001399201,-2.94155093162123,
1.99444839709469));
#82180=CARTESIAN_POINT('Ctrl Pts',(-15.9874976097487,-2.9105413106054,1.98946305219589));
#82181=CARTESIAN_POINT('Ctrl Pts',(-16.0788621431295,-2.87954286437116,
1.98447950384082));
#82182=CARTESIAN_POINT('Ctrl Pts',(-16.1688035955202,-2.84422541399118,
1.97949595548576));
#82183=CARTESIAN_POINT('Ctrl Pts',(-16.2568917918904,-2.80475048328343,
1.9745124071307));
#82184=CARTESIAN_POINT('Ctrl Pts',(-16.3449722529158,-2.76527901901284,
1.96952929639913));
#82185=CARTESIAN_POINT('Ctrl Pts',(-16.4311993812673,-2.72165097987983,
1.96454618566756));
#82186=CARTESIAN_POINT('Ctrl Pts',(-16.5151640047239,-2.67407559518967,
1.95956307493599));
#82187=CARTESIAN_POINT('Ctrl Pts',(-16.5991441392613,-2.62649142173107,
1.95457904365682));
#82188=CARTESIAN_POINT('Ctrl Pts',(-16.6808605571871,-2.57495867076684,
1.94959501237765));
#82189=CARTESIAN_POINT('Ctrl Pts',(-16.7599306010706,-2.51973143993866,
1.94461098109848));
#82190=CARTESIAN_POINT('Ctrl Pts',(-16.8390855806278,-2.46444488497419,
1.9396215960591));
#82191=CARTESIAN_POINT('Ctrl Pts',(-16.9155881509083,-2.40545617910367,
1.93463221101972));
#82192=CARTESIAN_POINT('Ctrl Pts',(-16.9890866539137,-2.34306135925256,
1.92964282598034));
#82193=CARTESIAN_POINT('Ctrl Pts',(-17.0626287225914,-2.28062955535191,
1.92465048352135));
#82194=CARTESIAN_POINT('Ctrl Pts',(-17.1331628579191,-2.21478791655874,
1.91965814106237));
#82195=CARTESIAN_POINT('Ctrl Pts',(-17.2003739173934,-2.14586972429713,
1.91466579860338));
#82196=CARTESIAN_POINT('Ctrl Pts',(-17.2676925653125,-2.07684121088909,
1.90966546462684));
#82197=CARTESIAN_POINT('Ctrl Pts',(-17.3316772251645,-2.00472663850662,
1.9046651306503));
#82198=CARTESIAN_POINT('Ctrl Pts',(-17.3920527740801,-1.92989268510343,
1.89966479667376));
#82199=CARTESIAN_POINT('Ctrl Pts',(-17.4255355574571,-1.88839162886379,
1.89689173535412));
#82200=CARTESIAN_POINT('Ctrl Pts',(-17.4579091067308,-1.8460547513915,1.89411867403449));
#82201=CARTESIAN_POINT('Ctrl Pts',(-17.4891324092414,-1.80294816876802,
1.89134561271486));
#82202=CARTESIAN_POINT('Ctrl Pts',(-17.5458129998629,-1.72469550597112,
1.88631159194231));
#82203=CARTESIAN_POINT('Ctrl Pts',(-17.5988982171272,-1.64363182743569,
1.88127757116976));
#82204=CARTESIAN_POINT('Ctrl Pts',(-17.6480998096016,-1.56011847254879,
1.87624355039721));
#82205=CARTESIAN_POINT('Ctrl Pts',(-17.6972334799748,-1.47672040666498,
1.87121647901901));
#82206=CARTESIAN_POINT('Ctrl Pts',(-17.7424939640519,-1.39087975307624,
1.86618940764081));
#82207=CARTESIAN_POINT('Ctrl Pts',(-17.783634744614,-1.30298881751823,1.8611623362626));
#82208=CARTESIAN_POINT('Ctrl Pts',(-17.8247294327806,-1.21519635125798,
1.85614089700318));
#82209=CARTESIAN_POINT('Ctrl Pts',(-17.8617134114388,-1.12535855738384,
1.85111945774376));
#82210=CARTESIAN_POINT('Ctrl Pts',(-17.8943852860642,-1.03389364337698,
1.84609801848433));
#82211=CARTESIAN_POINT('Ctrl Pts',(-17.9270269589727,-0.942513279077256,
1.84108122101814));
#82212=CARTESIAN_POINT('Ctrl Pts',(-17.9553643136507,-0.849509191330882,
1.83606442355194));
#82213=CARTESIAN_POINT('Ctrl Pts',(-17.97924386297,-0.755319968593296,1.83104762608575));
#82214=CARTESIAN_POINT('Ctrl Pts',(-18.0031103269534,-0.661182358957654,
1.8260335776865));
#82215=CARTESIAN_POINT('Ctrl Pts',(-18.0225237378336,-0.565861322705995,
1.82101952928725));
#82216=CARTESIAN_POINT('Ctrl Pts',(-18.0373805448444,-0.469810255103615,
1.81600548088801));
#82217=CARTESIAN_POINT('Ctrl Pts',(-18.0522352245164,-0.373772941005991,
1.81099215044787));
#82218=CARTESIAN_POINT('Ctrl Pts',(-18.0625345258306,-0.277006228114954,
1.80597882000772));
#82219=CARTESIAN_POINT('Ctrl Pts',(-18.068226216715,-0.179972589753701,
1.80096548956758));
#82220=CARTESIAN_POINT('Ctrl Pts',(-18.0717793388245,-0.119397907674138,
1.7978358439859));
#82221=CARTESIAN_POINT('Ctrl Pts',(-18.0735378699228,-0.0587193639364806,
1.79470619840423));
#82222=CARTESIAN_POINT('Ctrl Pts',(-18.0734993815187,0.00194982156482441,
1.79157655282255));
#82223=CARTESIAN_POINT('Origin',(-15.,0.,8.20842344717746));
#82224=CARTESIAN_POINT('',(-13.1276888212995,2.43738653071547,3.43723390425693));
#82225=CARTESIAN_POINT('',(-13.1276888212995,2.43738653071547,3.3542649531753));
#82226=CARTESIAN_POINT('',(-13.1276888212995,2.43738653071547,8.20842344717746));
#82227=CARTESIAN_POINT('',(-18.073499222413,0.00218628150294359,2.70842344717746));
#82228=CARTESIAN_POINT('Ctrl Pts',(-13.1276888212995,2.43738653071547,3.3542649531753));
#82229=CARTESIAN_POINT('Ctrl Pts',(-13.0512005964765,2.37863107417608,3.34927198847025));
#82230=CARTESIAN_POINT('Ctrl Pts',(-12.9775534946703,2.31632766092925,3.3442790237652));
#82231=CARTESIAN_POINT('Ctrl Pts',(-12.9070773460554,2.25079475177229,3.33928605906015));
#82232=CARTESIAN_POINT('Ctrl Pts',(-12.8364918224869,2.18516013928675,3.33428534555933));
#82233=CARTESIAN_POINT('Ctrl Pts',(-12.7690873807666,2.11628633992039,3.3292846320585));
#82234=CARTESIAN_POINT('Ctrl Pts',(-12.7051552920996,2.04452684419193,3.32428391855767));
#82235=CARTESIAN_POINT('Ctrl Pts',(-12.680628582491,2.01699725224389,3.3223654602306));
#82236=CARTESIAN_POINT('Ctrl Pts',(-12.6566124837819,1.98904327447208,3.32044700190352));
#82237=CARTESIAN_POINT('Ctrl Pts',(-12.6331217549234,1.9606860082591,3.31852854357645));
#82238=CARTESIAN_POINT('Ctrl Pts',(-12.5718880904872,1.88676666186203,3.31352766709695));
#82239=CARTESIAN_POINT('Ctrl Pts',(-12.5140137541319,1.80984705634736,3.30852679061746));
#82240=CARTESIAN_POINT('Ctrl Pts',(-12.4598061902056,1.73026519894555,3.30352591413796));
#82241=CARTESIAN_POINT('Ctrl Pts',(-12.4056718372278,1.65079082217648,3.29853179167736));
#82242=CARTESIAN_POINT('Ctrl Pts',(-12.3551946591348,1.56866169907131,3.29353766921675));
#82243=CARTESIAN_POINT('Ctrl Pts',(-12.3086423207339,1.48424933628268,3.28854354675615));
#82244=CARTESIAN_POINT('Ctrl Pts',(-12.2621388412056,1.39992556824611,3.28355466586238));
#82245=CARTESIAN_POINT('Ctrl Pts',(-12.2195522230033,1.31332370657085,3.27856578496861));
#82246=CARTESIAN_POINT('Ctrl Pts',(-12.1811066352899,1.22484384653443,3.27357690407484));
#82247=CARTESIAN_POINT('Ctrl Pts',(-12.1426883443105,1.13642680804277,3.2685915653341));
#82248=CARTESIAN_POINT('Ctrl Pts',(-12.1084054131327,1.04613482315557,3.26360622659336));
#82249=CARTESIAN_POINT('Ctrl Pts',(-12.0784354376814,0.95439130245612,3.25862088785262));
#82250=CARTESIAN_POINT('Ctrl Pts',(-12.048476262403,0.862680843041611,3.2536373456606));
#82251=CARTESIAN_POINT('Ctrl Pts',(-12.0228270907301,0.769520303724429,
3.24865380346858));
#82252=CARTESIAN_POINT('Ctrl Pts',(-12.0016165162505,0.675350823186146,
3.24367026127656));
#82253=CARTESIAN_POINT('Ctrl Pts',(-11.9804078043398,0.581189611973402,
3.23868715670544));
#82254=CARTESIAN_POINT('Ctrl Pts',(-11.9636370108476,0.4860200636921,3.23370405213432));
#82255=CARTESIAN_POINT('Ctrl Pts',(-11.9513819554675,0.390295104441535,
3.2287209475632));
#82256=CARTESIAN_POINT('Ctrl Pts',(-11.9391246361399,0.294552461363366,
3.22373692243424));
#82257=CARTESIAN_POINT('Ctrl Pts',(-11.9313847673773,0.198254638653824,
3.21875289730527));
#82258=CARTESIAN_POINT('Ctrl Pts',(-11.9281883615582,0.101860237252839,
3.2137688721763));
#82259=CARTESIAN_POINT('Ctrl Pts',(-11.9249885221769,0.00536228950122442,
3.20877949323419));
#82260=CARTESIAN_POINT('Ctrl Pts',(-11.926341903648,-0.0912320049161493,
3.20379011429208));
#82261=CARTESIAN_POINT('Ctrl Pts',(-11.9322223670329,-0.187463715600849,
3.19880073534997));
#82262=CARTESIAN_POINT('Ctrl Pts',(-11.9381063160463,-0.283752467368255,
3.19380839896716));
#82263=CARTESIAN_POINT('Ctrl Pts',(-11.9485226428087,-0.379677771578006,
3.18881606258436));
#82264=CARTESIAN_POINT('Ctrl Pts',(-11.96339350805,-0.474787597823518,3.18382372620156));
#82265=CARTESIAN_POINT('Ctrl Pts',(-11.9782881782089,-0.570049673554757,
3.17882339820867));
#82266=CARTESIAN_POINT('Ctrl Pts',(-11.9976515367199,-0.664493235451254,
3.17382307021578));
#82267=CARTESIAN_POINT('Ctrl Pts',(-12.0213550232632,-0.757678264542756,
3.16882274222289));
#82268=CARTESIAN_POINT('Ctrl Pts',(-12.0345006951214,-0.809357573926145,
3.16604961976017));
#82269=CARTESIAN_POINT('Ctrl Pts',(-12.0489803672796,-0.860650087863547,
3.16327649729744));
#82270=CARTESIAN_POINT('Ctrl Pts',(-12.0647657044095,-0.91148334048911,
3.16050337483472));
#82271=CARTESIAN_POINT('Ctrl Pts',(-12.0932319989279,-1.00315286446984,
3.15550249838146));
#82272=CARTESIAN_POINT('Ctrl Pts',(-12.126046426735,-1.09364749385214,3.15050162192819));
#82273=CARTESIAN_POINT('Ctrl Pts',(-12.1630938131952,-1.18252506834685,
3.14550074547493));
#82274=CARTESIAN_POINT('Ctrl Pts',(-12.2000911647162,-1.27128260781442,
3.1405066230352));
#82275=CARTESIAN_POINT('Ctrl Pts',(-12.2413099453687,-1.35842703143618,
3.13551250059547));
#82276=CARTESIAN_POINT('Ctrl Pts',(-12.2865851908717,-1.44353119938691,
3.13051837815574));
#82277=CARTESIAN_POINT('Ctrl Pts',(-12.3318129179195,-1.52854604659407,
3.1255294972775));
#82278=CARTESIAN_POINT('Ctrl Pts',(-12.3810884411476,-1.61152450983249,
3.12054061639926));
#82279=CARTESIAN_POINT('Ctrl Pts',(-12.4341990900186,-1.69206026498422,
3.11555173552103));
#82280=CARTESIAN_POINT('Ctrl Pts',(-12.4872720299071,-1.77253883911039,
3.11056639678782));
#82281=CARTESIAN_POINT('Ctrl Pts',(-12.5441744414,-1.85057778781918,3.10558105805462));
#82282=CARTESIAN_POINT('Ctrl Pts',(-12.6046486835395,-1.92579706114918,
3.10059571932141));
#82283=CARTESIAN_POINT('Ctrl Pts',(-12.6651011328523,-2.00098922805294,
3.09561217713198));
#82284=CARTESIAN_POINT('Ctrl Pts',(-12.7291225806967,-2.07336339700366,
3.09062863494254));
#82285=CARTESIAN_POINT('Ctrl Pts',(-12.7964137686971,-2.14257087892379,
3.0856450927531));
#82286=CARTESIAN_POINT('Ctrl Pts',(-12.8636990477083,-2.21177228358065,
3.08066198817962));
#82287=CARTESIAN_POINT('Ctrl Pts',(-12.9342531900463,-2.2778072397267,3.07567888360613));
#82288=CARTESIAN_POINT('Ctrl Pts',(-13.0077393281836,-2.34036314821731,
3.07069577903264));
#82289=CARTESIAN_POINT('Ctrl Pts',(-13.0812390419149,-2.40293061308626,
3.06571175389636));
#82290=CARTESIAN_POINT('Ctrl Pts',(-13.1576714931271,-2.46201746954657,
3.06072772876008));
#82291=CARTESIAN_POINT('Ctrl Pts',(-13.2366667606056,-2.51735141306231,
3.0557437036238));
#82292=CARTESIAN_POINT('Ctrl Pts',(-13.3157468844965,-2.57274479608733,
3.05075432466689));
#82293=CARTESIAN_POINT('Ctrl Pts',(-13.397394960687,-2.62437696604428,3.04576494570998));
#82294=CARTESIAN_POINT('Ctrl Pts',(-13.481212303729,-2.67201912112464,3.04077556675307));
#82295=CARTESIAN_POINT('Ctrl Pts',(-13.5650793293426,-2.71968951600236,
3.03578323035122));
#82296=CARTESIAN_POINT('Ctrl Pts',(-13.651117791172,-2.76336498825401,3.03079089394936));
#82297=CARTESIAN_POINT('Ctrl Pts',(-13.7389065413854,-2.80286381021972,
3.02579855754751));
#82298=CARTESIAN_POINT('Ctrl Pts',(-13.8268358217984,-2.84242586098552,
3.02079822952907));
#82299=CARTESIAN_POINT('Ctrl Pts',(-13.9165205772469,-2.87779775093621,
3.01579790151064));
#82300=CARTESIAN_POINT('Ctrl Pts',(-14.0075220138788,-2.90884679848645,
3.01079757349221));
#82301=CARTESIAN_POINT('Ctrl Pts',(-14.0579903286513,-2.92606623109265,
3.0080244510258));
#82302=CARTESIAN_POINT('Ctrl Pts',(-14.1088633714619,-2.9419569941894,3.00525132855939));
#82303=CARTESIAN_POINT('Ctrl Pts',(-14.1600649653456,-2.95650323652116,
3.00247820609297));
#82304=CARTESIAN_POINT('Ctrl Pts',(-14.252398734525,-2.9827350250264,2.99747732955187));
#82305=CARTESIAN_POINT('Ctrl Pts',(-14.3461236146214,-3.00468295413524,
2.99247645301077));
#82306=CARTESIAN_POINT('Ctrl Pts',(-14.4408063302793,-3.02220196044941,
2.98747557646967));
#82307=CARTESIAN_POINT('Ctrl Pts',(-14.5353611706074,-3.03969730617577,
2.98248145394627));
#82308=CARTESIAN_POINT('Ctrl Pts',(-14.6308708477552,-3.0527755381568,2.97748733142286));
#82309=CARTESIAN_POINT('Ctrl Pts',(-14.7268874695359,-3.06134150262651,
2.97249320889945));
#82310=CARTESIAN_POINT('Ctrl Pts',(-14.8228033173709,-3.06989847671494,
2.96750432794175));
#82311=CARTESIAN_POINT('Ctrl Pts',(-14.9192246174675,-3.07395255926622,
2.96251544698405));
#82312=CARTESIAN_POINT('Ctrl Pts',(-15.0156948530631,-3.07345992679054,
2.95752656602635));
#82313=CARTESIAN_POINT('Ctrl Pts',(-15.1120965939003,-3.07296764408847,
2.95254122722022));
#82314=CARTESIAN_POINT('Ctrl Pts',(-15.208546763739,-3.06793506622035,2.94755588841409));
#82315=CARTESIAN_POINT('Ctrl Pts',(-15.3045862878005,-3.05837039013981,
2.94257054960795));
#82316=CARTESIAN_POINT('Ctrl Pts',(-15.4005912024592,-3.04880916084568,
2.93758700734965));
#82317=CARTESIAN_POINT('Ctrl Pts',(-15.4961853293009,-3.03471912188065,
2.93260346509135));
#82318=CARTESIAN_POINT('Ctrl Pts',(-15.5909131278633,-3.01616046080423,
2.92761992283305));
#82319=CARTESIAN_POINT('Ctrl Pts',(-15.6856326080882,-2.99760342942058,
2.92263681819482));
#82320=CARTESIAN_POINT('Ctrl Pts',(-15.7794854808445,-2.97457864067198,
2.9176537135566));
#82321=CARTESIAN_POINT('Ctrl Pts',(-15.8720258906693,-2.94719749864211,
2.91267060891838));
#82322=CARTESIAN_POINT('Ctrl Pts',(-15.9645833960353,-2.91981129833078,
2.90768658372155));
#82323=CARTESIAN_POINT('Ctrl Pts',(-16.0558275363149,-2.88806727092228,
2.90270255852472));
#82324=CARTESIAN_POINT('Ctrl Pts',(-16.1453281514182,-2.85212651815606,
2.8977185333279));
#82325=CARTESIAN_POINT('Ctrl Pts',(-16.2349249076165,-2.81614715802023,
2.89272915431714));
#82326=CARTESIAN_POINT('Ctrl Pts',(-16.3227739919592,-2.77596223648105,
2.88773977530638));
#82327=CARTESIAN_POINT('Ctrl Pts',(-16.4084659700617,-2.73178071249838,
2.88275039629561));
#82328=CARTESIAN_POINT('Ctrl Pts',(-16.4942087418581,-2.68757300003394,
2.87775805984361));
#82329=CARTESIAN_POINT('Ctrl Pts',(-16.5777914816568,-2.63936418712446,
2.87276572339161));
#82330=CARTESIAN_POINT('Ctrl Pts',(-16.6588319147118,-2.58740776236247,
2.8677733869396));
#82331=CARTESIAN_POINT('Ctrl Pts',(-16.7400020753135,-2.53536816702421,
2.86277305887729));
#82332=CARTESIAN_POINT('Ctrl Pts',(-16.8186214458339,-2.47956923514097,
2.85777273081498));
#82333=CARTESIAN_POINT('Ctrl Pts',(-16.8943391938762,-2.42030602787013,
2.85277240275267));
#82334=CARTESIAN_POINT('Ctrl Pts',(-16.9363313462235,-2.38743936592297,
2.8499992809522));
#82335=CARTESIAN_POINT('Ctrl Pts',(-16.9774316737466,-2.35350789689179,
2.84722615915172));
#82336=CARTESIAN_POINT('Ctrl Pts',(-17.0175852866678,-2.31856676872189,
2.84445303735124));
#82337=CARTESIAN_POINT('Ctrl Pts',(-17.0889589316375,-2.25645839302651,
2.83952377205118));
#82338=CARTESIAN_POINT('Ctrl Pts',(-17.1576039115037,-2.19092748187001,
2.83459450675111));
#82339=CARTESIAN_POINT('Ctrl Pts',(-17.2231671496839,-2.12224646885475,
2.82966524145105));
#82340=CARTESIAN_POINT('Ctrl Pts',(-17.2903594199941,-2.05185895719735,
2.82461350002298));
#82341=CARTESIAN_POINT('Ctrl Pts',(-17.3543143585099,-1.97816296494052,
2.81956175859491));
#82342=CARTESIAN_POINT('Ctrl Pts',(-17.4146868794231,-1.90149665378145,
2.81451001716685));
#82343=CARTESIAN_POINT('Ctrl Pts',(-17.4734480008263,-1.82687663875776,
2.80959311148091));
#82344=CARTESIAN_POINT('Ctrl Pts',(-17.52881521957,-1.74944324297213,2.80467620579497));
#82345=CARTESIAN_POINT('Ctrl Pts',(-17.5805078919353,-1.66954522839601,
2.79975930010903));
#82346=CARTESIAN_POINT('Ctrl Pts',(-17.6321694728631,-1.58969526984033,
2.79484535177968));
#82347=CARTESIAN_POINT('Ctrl Pts',(-17.6801606504181,-1.50738401458739,
2.78993140345033));
#82348=CARTESIAN_POINT('Ctrl Pts',(-17.724242835189,-1.42299094337295,2.78501745512099));
#82349=CARTESIAN_POINT('Ctrl Pts',(-17.7683113470811,-1.33862404818035,
2.78010503094069));
#82350=CARTESIAN_POINT('Ctrl Pts',(-17.8084730657097,-1.25217702067679,
2.77519260676039));
#82351=CARTESIAN_POINT('Ctrl Pts',(-17.8445349215123,-1.1640546938597,2.77028018258008));
#82352=CARTESIAN_POINT('Ctrl Pts',(-17.8823755169536,-1.07158576112708,
2.76512545462987));
#82353=CARTESIAN_POINT('Ctrl Pts',(-17.9157011777319,-0.977272502073842,
2.75997072667965));
#82354=CARTESIAN_POINT('Ctrl Pts',(-17.9443460255526,-0.881605768931114,
2.75481599872943));
#82355=CARTESIAN_POINT('Ctrl Pts',(-17.9716643411015,-0.790369326695886,
2.74989998431753));
#82356=CARTESIAN_POINT('Ctrl Pts',(-17.9947256424304,-0.69790244673538,
2.74498396990564));
#82357=CARTESIAN_POINT('Ctrl Pts',(-18.0134378458492,-0.604644192234935,
2.74006795549375));
#82358=CARTESIAN_POINT('Ctrl Pts',(-18.032158764123,-0.511342504466295,
2.73514965154112));
#82359=CARTESIAN_POINT('Ctrl Pts',(-18.0465264852592,-0.417249155543324,
2.73023134758849));
#82360=CARTESIAN_POINT('Ctrl Pts',(-18.056500603696,-0.322810020919425,
2.72531304363586));
#82361=CARTESIAN_POINT('Ctrl Pts',(-18.0664867611952,-0.228256895406328,
2.72038880314175));
#82362=CARTESIAN_POINT('Ctrl Pts',(-18.0720687134541,-0.133357602149294,
2.71546456264763));
#82363=CARTESIAN_POINT('Ctrl Pts',(-18.0732581163465,-0.0385590496523394,
2.71054032215352));
#82364=CARTESIAN_POINT('Ctrl Pts',(-18.0734285532713,-0.0249747765184603,
2.7098346971615));
#82365=CARTESIAN_POINT('Ctrl Pts',(-18.0735088814944,-0.0113925642842438,
2.70912907216948));
#82366=CARTESIAN_POINT('Ctrl Pts',(-18.073499222413,0.00218628150294359,
2.70842344717746));
#82367=CARTESIAN_POINT('Ctrl Pts',(-18.0762767414075,0.00218825724393669,
2.70842344717746));
#82368=CARTESIAN_POINT('Ctrl Pts',(-18.0774175670185,0.143408855469269,
2.70109158765481));
#82369=CARTESIAN_POINT('Ctrl Pts',(-18.0046436801636,1.2980338168667,2.64108467188491));
#82370=CARTESIAN_POINT('Ctrl Pts',(-16.5438880884248,3.28204007054153,2.52840269986777));
#82371=CARTESIAN_POINT('Ctrl Pts',(-14.1255737879022,3.14463322099092,2.41762057516619));
#82372=CARTESIAN_POINT('Ctrl Pts',(-13.2078714909188,2.50458144295651,2.35951350671185));
#82373=CARTESIAN_POINT('Ctrl Pts',(-13.1254325828889,2.44028101900739,2.35408149450477));
#82374=CARTESIAN_POINT('',(-18.0734989461686,-0.00254517198238653,2.79157655284933));
#82375=CARTESIAN_POINT('Ctrl Pts',(-18.073498946169,-0.00254517146422184,
2.79157655282255));
#82376=CARTESIAN_POINT('Ctrl Pts',(-18.0735783970018,0.0933980898477828,
2.78661850057295));
#82377=CARTESIAN_POINT('Ctrl Pts',(-18.0691610737691,0.189417023051302,
2.78166044832335));
#82378=CARTESIAN_POINT('Ctrl Pts',(-18.0602524559986,0.285056407671365,
2.77670239607375));
#82379=CARTESIAN_POINT('Ctrl Pts',(-18.0513467904042,0.380664098900641,
2.77174598684483));
#82380=CARTESIAN_POINT('Ctrl Pts',(-18.0379528279,0.47589204991766,2.76678957761592));
#82381=CARTESIAN_POINT('Ctrl Pts',(-18.0201280577465,0.570288317267858,
2.76183316838701));
#82382=CARTESIAN_POINT('Ctrl Pts',(-18.0023042035091,0.664679734117188,
2.75687701384049));
#82383=CARTESIAN_POINT('Ctrl Pts',(-17.980050077036,0.75823911624815,2.75192085929396));
#82384=CARTESIAN_POINT('Ctrl Pts',(-17.9534744186567,0.850524019849157,
2.74696470474744));
#82385=CARTESIAN_POINT('Ctrl Pts',(-17.9268926845698,0.942830021557655,
2.74200741712848));
#82386=CARTESIAN_POINT('Ctrl Pts',(-17.895987579697,1.03386053982986,2.73705012950952));
#82387=CARTESIAN_POINT('Ctrl Pts',(-17.8609175744308,1.12318871179908,2.73209284189055));
#82388=CARTESIAN_POINT('Ctrl Pts',(-17.8258083482045,1.21261678499865,2.72713001022964));
#82389=CARTESIAN_POINT('Ctrl Pts',(-17.7865250883768,1.3003382988599,2.72216717856873));
#82390=CARTESIAN_POINT('Ctrl Pts',(-17.743274126476,1.38594708304738,2.71720434690782));
#82391=CARTESIAN_POINT('Ctrl Pts',(-17.6999952881571,1.47161104441819,2.7122383165673));
#82392=CARTESIAN_POINT('Ctrl Pts',(-17.652743876713,1.55515918054058,2.70727228622678));
#82393=CARTESIAN_POINT('Ctrl Pts',(-17.6017707263958,1.63621249759002,2.70230625588626));
#82394=CARTESIAN_POINT('Ctrl Pts',(-17.5507164815259,1.71739476453662,2.6973323249548));
#82395=CARTESIAN_POINT('Ctrl Pts',(-17.4959289345585,1.79607392841621,2.69235839402335));
#82396=CARTESIAN_POINT('Ctrl Pts',(-17.4377003472425,1.87190257947729,2.6873844630919));
#82397=CARTESIAN_POINT('Ctrl Pts',(-17.4146263084971,1.90195093395825,2.68541346086911));
#82398=CARTESIAN_POINT('Ctrl Pts',(-17.391012352214,1.93155207610088,2.68344245864633));
#82399=CARTESIAN_POINT('Ctrl Pts',(-17.3668782450813,1.96068600825349,2.68147145642355));
#82400=CARTESIAN_POINT('Ctrl Pts',(-17.305644579888,2.03460535556479,2.67647057988226));
#82401=CARTESIAN_POINT('Ctrl Pts',(-17.2408379417085,2.10578234896841,2.67146970334098));
#82402=CARTESIAN_POINT('Ctrl Pts',(-17.1727332236773,2.17385201629014,2.6664688267997));
#82403=CARTESIAN_POINT('Ctrl Pts',(-17.1047204856153,2.24182975098103,2.6614747042761));
#82404=CARTESIAN_POINT('Ctrl Pts',(-17.0334188281061,2.30670819283883,2.6564805817525));
#82405=CARTESIAN_POINT('Ctrl Pts',(-16.9591434609307,2.36815522073461,2.6514864592289));
#82406=CARTESIAN_POINT('Ctrl Pts',(-16.8849460492348,2.42953775709419,2.646497578271));
#82407=CARTESIAN_POINT('Ctrl Pts',(-16.8077814686798,2.48749576090924,2.64150869731309));
#82408=CARTESIAN_POINT('Ctrl Pts',(-16.7280011121749,2.5417345271138,2.63651981635519));
#82409=CARTESIAN_POINT('Ctrl Pts',(-16.6482774004602,2.59593478329323,2.63153447754886));
#82410=CARTESIAN_POINT('Ctrl Pts',(-16.5659419666771,2.64642080558076,2.62654913874253));
#82411=CARTESIAN_POINT('Ctrl Pts',(-16.4813777783395,2.6929393100926,2.6215637999362));
#82412=CARTESIAN_POINT('Ctrl Pts',(-16.3968440640809,2.73944105090565,2.6165802576777));
#82413=CARTESIAN_POINT('Ctrl Pts',(-16.3100835750895,2.78197790357921,2.6115967154192));
#82414=CARTESIAN_POINT('Ctrl Pts',(-16.2215058158792,2.82034143177264,2.6066131731607));
#82415=CARTESIAN_POINT('Ctrl Pts',(-16.1329358349526,2.85870159114742,2.60163006852227));
#82416=CARTESIAN_POINT('Ctrl Pts',(-16.0425493037159,2.89288898053685,2.59664696388384));
#82417=CARTESIAN_POINT('Ctrl Pts',(-15.9507767564214,2.92274285722311,2.59166385924542));
#82418=CARTESIAN_POINT('Ctrl Pts',(-15.8589872554378,2.95260224899378,2.5866798340484));
#82419=CARTESIAN_POINT('Ctrl Pts',(-15.7658116470334,2.97812640246882,2.58169580885138));
#82420=CARTESIAN_POINT('Ctrl Pts',(-15.6716956816881,2.99920442137602,2.57671178365436));
#82421=CARTESIAN_POINT('Ctrl Pts',(-15.5774786174622,3.02030508218155,2.57172240464339));
#82422=CARTESIAN_POINT('Ctrl Pts',(-15.4823196084789,3.03694997776553,2.56673302563242));
#82423=CARTESIAN_POINT('Ctrl Pts',(-15.3866744334398,3.0490793909841,2.56174364662145));
#82424=CARTESIAN_POINT('Ctrl Pts',(-15.2909725649758,3.06121599388034,2.55675131016924));
#82425=CARTESIAN_POINT('Ctrl Pts',(-15.1947843937238,3.0688317503288,2.55175897371703));
#82426=CARTESIAN_POINT('Ctrl Pts',(-15.0985685395066,3.07191902448934,2.54676663726483));
#82427=CARTESIAN_POINT('Ctrl Pts',(-15.0021986652989,3.07501124068298,2.54176630920231));
#82428=CARTESIAN_POINT('Ctrl Pts',(-14.9058014579086,3.07356050693218,2.53676598113979));
#82429=CARTESIAN_POINT('Ctrl Pts',(-14.8098331738837,3.06761125767997,2.53176565307727));
#82430=CARTESIAN_POINT('Ctrl Pts',(-14.75661031789,3.0643118756035,2.52899253127878));
#82431=CARTESIAN_POINT('Ctrl Pts',(-14.7035192655416,3.05962981734055,2.52621940948029));
#82432=CARTESIAN_POINT('Ctrl Pts',(-14.6506364896964,3.05357943857178,2.52344628768181));
#82433=CARTESIAN_POINT('Ctrl Pts',(-14.5552763385047,3.04266917478673,2.51844569325858));
#82434=CARTESIAN_POINT('Ctrl Pts',(-14.4602614050597,3.02726860095593,2.51344509883535));
#82435=CARTESIAN_POINT('Ctrl Pts',(-14.366047481739,3.00740859455288,2.50844450441211));
#82436=CARTESIAN_POINT('Ctrl Pts',(-14.2719552305796,2.98757423626868,2.50345036798479));
#82437=CARTESIAN_POINT('Ctrl Pts',(-14.1786623596624,2.96329197809384,2.49845623155747));
#82438=CARTESIAN_POINT('Ctrl Pts',(-14.0866192495522,2.93464441708216,2.49346209513014));
#82439=CARTESIAN_POINT('Ctrl Pts',(-13.9946812594751,2.90602957370198,2.48847366237564));
#82440=CARTESIAN_POINT('Ctrl Pts',(-13.903990607949,2.8730594729685,2.48348522962115));
#82441=CARTESIAN_POINT('Ctrl Pts',(-13.8149859797168,2.83586741963234,2.47849679686665));
#82442=CARTESIAN_POINT('Ctrl Pts',(-13.726041367859,2.79870044512907,2.47351172784338));
#82443=CARTESIAN_POINT('Ctrl Pts',(-13.638780923381,2.75731734429835,2.46852665882011));
#82444=CARTESIAN_POINT('Ctrl Pts',(-13.5536259359272,2.71190049905551,2.46354158979685));
#82445=CARTESIAN_POINT('Ctrl Pts',(-13.4684942244174,2.66649606788231,2.45855788337359));
#82446=CARTESIAN_POINT('Ctrl Pts',(-13.3854672157398,2.61706028423352,2.45357417695034));
#82447=CARTESIAN_POINT('Ctrl Pts',(-13.3049432397788,2.56382230851289,2.44859047052709));
#82448=CARTESIAN_POINT('Ctrl Pts',(-13.244390459308,2.52378817683913,2.44484280062658));
#82449=CARTESIAN_POINT('Ctrl Pts',(-13.1852526641704,2.48160496925117,2.44109513072608));
#82450=CARTESIAN_POINT('Ctrl Pts',(-13.1276888212995,2.43738653071547,2.43734746082558));
#82451=CARTESIAN_POINT('Ctrl Pts',(-13.1276888212995,2.43738653071547,3.43723390425693));
#82452=CARTESIAN_POINT('Ctrl Pts',(-13.0487694023508,2.37676351977643,3.4320813303875));
#82453=CARTESIAN_POINT('Ctrl Pts',(-12.9727177480323,2.31224249060819,3.42692875651806));
#82454=CARTESIAN_POINT('Ctrl Pts',(-12.8999347369254,2.24413193480849,3.42177618264863));
#82455=CARTESIAN_POINT('Ctrl Pts',(-12.8295244108795,2.17824174466537,3.41679157977764));
#82456=CARTESIAN_POINT('Ctrl Pts',(-12.7621732628445,2.10899276086274,3.41180697690666));
#82457=CARTESIAN_POINT('Ctrl Pts',(-12.698210607387,2.03670514362153,3.40682237403567));
#82458=CARTESIAN_POINT('Ctrl Pts',(-12.6342653270429,1.96443716292499,3.4018391252054));
#82459=CARTESIAN_POINT('Ctrl Pts',(-12.5737070006539,1.88913251742462,3.39685587637513));
#82460=CARTESIAN_POINT('Ctrl Pts',(-12.5168267268034,1.81114680390137,3.39187262754486));
#82461=CARTESIAN_POINT('Ctrl Pts',(-12.4599464013209,1.73316101958798,3.38688937419114));
#82462=CARTESIAN_POINT('Ctrl Pts',(-12.4067443928656,1.65249451735772,3.38190612083741));
#82463=CARTESIAN_POINT('Ctrl Pts',(-12.357469641323,1.56953354646232,3.37692286748369));
#82464=CARTESIAN_POINT('Ctrl Pts',(-12.3081814153039,1.48654988939138,3.37193825142941));
#82465=CARTESIAN_POINT('Ctrl Pts',(-12.2628228034069,1.40127089438487,3.36695363537514));
#82466=CARTESIAN_POINT('Ctrl Pts',(-12.2215972575323,1.31410823399282,3.36196901932087));
#82467=CARTESIAN_POINT('Ctrl Pts',(-12.1803254865548,1.22684784043912,3.35697881414983));
#82468=CARTESIAN_POINT('Ctrl Pts',(-12.1431962169842,1.13769996377204,3.35198860897879));
#82469=CARTESIAN_POINT('Ctrl Pts',(-12.110365000904,1.04709685416357,3.34699840380776));
#82470=CARTESIAN_POINT('Ctrl Pts',(-12.0775117119113,0.956432830743878,
3.34200484364794));
#82471=CARTESIAN_POINT('Ctrl Pts',(-12.0489623581175,0.864312045096493,
3.33701128348813));
#82472=CARTESIAN_POINT('Ctrl Pts',(-12.0248222175848,0.771180532056574,
3.33201772332832));
#82473=CARTESIAN_POINT('Ctrl Pts',(-12.000645641924,0.677908454027049,3.32701662630253));
#82474=CARTESIAN_POINT('Ctrl Pts',(-11.9808916476761,0.58362303269245,3.32201552927674));
#82475=CARTESIAN_POINT('Ctrl Pts',(-11.9656141365388,0.488778765523918,
3.31701443225095));
#82476=CARTESIAN_POINT('Ctrl Pts',(-11.9621089196193,0.467018039773852,
3.3158669986308));
#82477=CARTESIAN_POINT('Ctrl Pts',(-11.9588391329913,0.445227906867683,
3.31471956501064));
#82478=CARTESIAN_POINT('Ctrl Pts',(-11.9558050410964,0.423413866312542,
3.31357213139049));
#82479=CARTESIAN_POINT('Ctrl Pts',(-11.9425815121966,0.328341401241128,
3.30857125397406));
#82480=CARTESIAN_POINT('Ctrl Pts',(-11.9337929567606,0.232483018086391,
3.30357037655762));
#82481=CARTESIAN_POINT('Ctrl Pts',(-11.9295231862109,0.136287879077004,
3.29856949914118));
#82482=CARTESIAN_POINT('Ctrl Pts',(-11.9252591822595,0.0402226577582837,
3.29357537572969));
#82483=CARTESIAN_POINT('Ctrl Pts',(-11.9255018531107,-0.0561779809558096,
3.2885812523182));
#82484=CARTESIAN_POINT('Ctrl Pts',(-11.930283559738,-0.152457293643444,
3.28358712890672));
#82485=CARTESIAN_POINT('Ctrl Pts',(-11.9350602477518,-0.248635556916652,
3.27859824704954));
#82486=CARTESIAN_POINT('Ctrl Pts',(-11.9443664793168,-0.344692311475923,
3.27360936519236));
#82487=CARTESIAN_POINT('Ctrl Pts',(-11.9581825858215,-0.440169363768726,
3.26862048333518));
#82488=CARTESIAN_POINT('Ctrl Pts',(-11.9719888828012,-0.535578626736652,
3.2636351436164));
#82489=CARTESIAN_POINT('Ctrl Pts',(-11.9902986264711,-0.630408572754681,
3.25864980389762));
#82490=CARTESIAN_POINT('Ctrl Pts',(-12.0130402732352,-0.724205661870558,
3.25366446417884));
#82491=CARTESIAN_POINT('Ctrl Pts',(-12.0357737247145,-0.817968949834355,
3.2486809210001));
#82492=CARTESIAN_POINT('Ctrl Pts',(-12.0629358026725,-0.910699694556035,
3.24369737782135));
#82493=CARTESIAN_POINT('Ctrl Pts',(-12.0944039597898,-1.00195503946786,
3.23871383464261));
#82494=CARTESIAN_POINT('Ctrl Pts',(-12.1258693536345,-1.09320237109201,
3.2337307290773));
#82495=CARTESIAN_POINT('Ctrl Pts',(-12.1616399316239,-1.18297414586291,
3.228747623512));
#82496=CARTESIAN_POINT('Ctrl Pts',(-12.2015437591438,-1.27084417534677,
3.22376451794669));
#82497=CARTESIAN_POINT('Ctrl Pts',(-12.241454958378,-1.35873043767837,3.21878049181729));
#82498=CARTESIAN_POINT('Ctrl Pts',(-12.2855007421938,-1.44471385759508,
3.2137964656879));
#82499=CARTESIAN_POINT('Ctrl Pts',(-12.3334621233701,-1.52839065768477,
3.2088124395585));
#82500=CARTESIAN_POINT('Ctrl Pts',(-12.3814750244284,-1.61215734298556,
3.20382305961251));
#82501=CARTESIAN_POINT('Ctrl Pts',(-12.4334117012619,-1.69361208076667,
3.19883367966651));
#82502=CARTESIAN_POINT('Ctrl Pts',(-12.4890086318113,-1.77237823245545,
3.19384429972052));
#82503=CARTESIAN_POINT('Ctrl Pts',(-12.5446385173203,-1.85119107260919,
3.18885196233043));
#82504=CARTESIAN_POINT('Ctrl Pts',(-12.6039327071977,-1.92731180752927,
3.18385962494033));
#82505=CARTESIAN_POINT('Ctrl Pts',(-12.6665873291252,-2.00039684997779,
3.17886728755024));
#82506=CARTESIAN_POINT('Ctrl Pts',(-12.7293422469639,-2.07359888508704,
3.17386695855454));
#82507=CARTESIAN_POINT('Ctrl Pts',(-12.7954680370553,-2.14375520587752,
3.16886662955885));
#82508=CARTESIAN_POINT('Ctrl Pts',(-12.8646239972249,-2.2105591095404,3.16386630056315));
#82509=CARTESIAN_POINT('Ctrl Pts',(-12.9029769270648,-2.24760762168504,
3.16109318792502));
#82510=CARTESIAN_POINT('Ctrl Pts',(-12.942261233082,-2.28362575600063,3.15832007528689));
#82511=CARTESIAN_POINT('Ctrl Pts',(-12.9824147133364,-2.31856676872561,
3.15554696264875));
#82512=CARTESIAN_POINT('Ctrl Pts',(-13.0548252580608,-2.38157744049307,
3.15054608612606));
#82513=CARTESIAN_POINT('Ctrl Pts',(-13.1303167553614,-2.44130263322672,
3.14554520960336));
#82514=CARTESIAN_POINT('Ctrl Pts',(-13.2085587636618,-2.49742678506238,
3.14054433308066));
#82515=CARTESIAN_POINT('Ctrl Pts',(-13.2866951009647,-2.55347513752583,
3.13555021057184));
#82516=CARTESIAN_POINT('Ctrl Pts',(-13.3675742128677,-2.60593186153271,
3.13055608806303));
#82517=CARTESIAN_POINT('Ctrl Pts',(-13.4508312022446,-2.65452034952854,
3.12556196555422));
#82518=CARTESIAN_POINT('Ctrl Pts',(-13.534000809571,-2.70305784166514,3.12057308460733));
#82519=CARTESIAN_POINT('Ctrl Pts',(-13.6195429561016,-2.74773494882954,
3.11558420366044));
#82520=CARTESIAN_POINT('Ctrl Pts',(-13.7070631082673,-2.78831785203852,
3.11059532271355));
#82521=CARTESIAN_POINT('Ctrl Pts',(-13.7945211204159,-2.8288719410574,3.10560998391255));
#82522=CARTESIAN_POINT('Ctrl Pts',(-13.8839539494324,-2.86533742101005,
3.10062464511156));
#82523=CARTESIAN_POINT('Ctrl Pts',(-13.9749426223322,-2.89752646622749,
3.09563930631056));
#82524=CARTESIAN_POINT('Ctrl Pts',(-14.0658985060495,-2.92970391162219,
3.09065576405388));
#82525=CARTESIAN_POINT('Ctrl Pts',(-14.1584087064832,-2.95760783816921,
3.08567222179721));
#82526=CARTESIAN_POINT('Ctrl Pts',(-14.252035337805,-2.98109897757648,3.08068867954053));
#82527=CARTESIAN_POINT('Ctrl Pts',(-14.3456537475521,-3.00458805417153,
3.07570557490043));
#82528=CARTESIAN_POINT('Ctrl Pts',(-14.4403879677316,-3.0236650075225,3.07072247026032));
#82529=CARTESIAN_POINT('Ctrl Pts',(-14.5357870955796,-3.03824104201257,
3.06573936562021));
#82530=CARTESIAN_POINT('Ctrl Pts',(-14.631203847144,-3.05281976923058,3.06075534041799));
#82531=CARTESIAN_POINT('Ctrl Pts',(-14.7272853166938,-3.06289586001435,
3.05577131521577));
#82532=CARTESIAN_POINT('Ctrl Pts',(-14.8235736702086,-3.06843217297634,
3.05078729001355));
#82533=CARTESIAN_POINT('Ctrl Pts',(-14.9199654562741,-3.07397443302281,
3.04579791099209));
#82534=CARTESIAN_POINT('Ctrl Pts',(-15.0165641313095,-3.07496715457057,
3.04080853197063));
#82535=CARTESIAN_POINT('Ctrl Pts',(-15.1129102654888,-3.0714253241691,3.03581915294917));
#82536=CARTESIAN_POINT('Ctrl Pts',(-15.2093135086429,-3.06788139435487,
3.03082681648345));
#82537=CARTESIAN_POINT('Ctrl Pts',(-15.3054634759748,-3.05979759733429,
3.02583448001773));
#82538=CARTESIAN_POINT('Ctrl Pts',(-15.4009063801237,-3.04724077230142,
3.02084214355202));
#82539=CARTESIAN_POINT('Ctrl Pts',(-15.4965020670309,-3.03466384659808,
3.01584181547139));
#82540=CARTESIAN_POINT('Ctrl Pts',(-15.591387999395,-3.01759967345029,3.01084148739077));
#82541=CARTESIAN_POINT('Ctrl Pts',(-15.6851211660381,-2.99616608982991,
3.00584115931014));
#82542=CARTESIAN_POINT('Ctrl Pts',(-15.7371044526759,-2.98427928219375,
3.0030680375091));
#82543=CARTESIAN_POINT('Ctrl Pts',(-15.7887334530627,-2.97104947536094,
3.00029491570806));
#82544=CARTESIAN_POINT('Ctrl Pts',(-15.8399350346618,-2.95650323651907,
2.99752179390702));
#82545=CARTESIAN_POINT('Ctrl Pts',(-15.9322688027063,-2.93027144833599,
2.99252091742743));
#82546=CARTESIAN_POINT('Ctrl Pts',(-16.0235336132318,-2.89966427791211,
2.98752004094784));
#82547=CARTESIAN_POINT('Ctrl Pts',(-16.1132846394274,-2.86478612842476,
2.98251916446826));
#82548=CARTESIAN_POINT('Ctrl Pts',(-16.2029144508463,-2.82995508421613,
2.97752504200756));
#82549=CARTESIAN_POINT('Ctrl Pts',(-16.2910341358345,-2.79086468273055,
2.97253091954686));
#82550=CARTESIAN_POINT('Ctrl Pts',(-16.3772126745151,-2.74766946686733,
2.96753679708616));
#82551=CARTESIAN_POINT('Ctrl Pts',(-16.463300764759,-2.70451958641832,2.96254791619228));
#82552=CARTESIAN_POINT('Ctrl Pts',(-16.5474513687489,-2.65727365173485,
2.9575590352984));
#82553=CARTESIAN_POINT('Ctrl Pts',(-16.6292531176695,-2.60613440339599,
2.95257015440452));
#82554=CARTESIAN_POINT('Ctrl Pts',(-16.710996786568,-2.55503146441131,2.94758481566367));
#82555=CARTESIAN_POINT('Ctrl Pts',(-16.7903945448615,-2.50004093901466,
2.94259947692282));
#82556=CARTESIAN_POINT('Ctrl Pts',(-16.867060198074,-2.44141116298914,2.93761413818197));
#82557=CARTESIAN_POINT('Ctrl Pts',(-16.9436982235588,-2.3828025151666,2.93263059598983));
#82558=CARTESIAN_POINT('Ctrl Pts',(-17.0176057521235,-2.32055748873695,
2.9276470537977));
#82559=CARTESIAN_POINT('Ctrl Pts',(-17.0884269302826,-2.25496678620115,
2.92266351160556));
#82560=CARTESIAN_POINT('Ctrl Pts',(-17.159241889406,-2.18938184339621,2.91768040703432));
#82561=CARTESIAN_POINT('Ctrl Pts',(-17.2269707152862,-2.12045210685458,
2.91269730246307));
#82562=CARTESIAN_POINT('Ctrl Pts',(-17.2912927204202,-2.04850675355227,
2.90771419789183));
#82563=CARTESIAN_POINT('Ctrl Pts',(-17.3556266081319,-1.97654810936699,
2.90273017276274));
#82564=CARTESIAN_POINT('Ctrl Pts',(-17.4165521328222,-1.90157306906267,
2.89774614763365));
#82565=CARTESIAN_POINT('Ctrl Pts',(-17.4737880870322,-1.82394483207617,
2.89276212250455));
#82566=CARTESIAN_POINT('Ctrl Pts',(-17.5310855237983,-1.74623320725247,
2.88777274356231));
#82567=CARTESIAN_POINT('Ctrl Pts',(-17.5846852171434,-1.66586304967478,
2.88278336462006));
#82568=CARTESIAN_POINT('Ctrl Pts',(-17.6343487509913,-1.58322737095795,
2.87779398567782));
#82569=CARTESIAN_POINT('Ctrl Pts',(-17.6840417227628,-1.50054271016905,
2.87280164929488));
#82570=CARTESIAN_POINT('Ctrl Pts',(-17.7297936814228,-1.41559024033998,
2.86780931291195));
#82571=CARTESIAN_POINT('Ctrl Pts',(-17.7714127256809,-1.32878657200253,
2.86281697652901));
#82572=CARTESIAN_POINT('Ctrl Pts',(-17.8130983926879,-1.24184395047389,
2.85781664853598));
#82573=CARTESIAN_POINT('Ctrl Pts',(-17.850637764712,-1.15304461722821,2.85281632054295));
#82574=CARTESIAN_POINT('Ctrl Pts',(-17.8838875435545,-1.0628240146569,2.84781599254992));
#82575=CARTESIAN_POINT('Ctrl Pts',(-17.9023274756305,-1.01278874100421,
2.84504287008838));
#82576=CARTESIAN_POINT('Ctrl Pts',(-17.9194489584675,-0.962316593092614,
2.84226974762683));
#82577=CARTESIAN_POINT('Ctrl Pts',(-17.9352342955905,-0.911483340489207,
2.83949662516529));
#82578=CARTESIAN_POINT('Ctrl Pts',(-17.9696909433996,-0.800523183712012,
2.83344338073697));
#82579=CARTESIAN_POINT('Ctrl Pts',(-17.9978758533101,-0.687529803808016,
2.82739013630864));
#82580=CARTESIAN_POINT('Ctrl Pts',(-18.0195867091523,-0.57314776097502,
2.82133689188032));
#82581=CARTESIAN_POINT('Ctrl Pts',(-18.0410343069052,-0.460152673970379,
2.81535704693352));
#82582=CARTESIAN_POINT('Ctrl Pts',(-18.0561638683813,-0.345802413307247,
2.80937720198673));
#82583=CARTESIAN_POINT('Ctrl Pts',(-18.0648265530853,-0.230738920651397,
2.80339735703993));
#82584=CARTESIAN_POINT('Ctrl Pts',(-18.0705346107669,-0.154920733152448,
2.7994570889764));
#82585=CARTESIAN_POINT('Ctrl Pts',(-18.0734358049133,-0.0787932931042968,
2.79551682091286));
#82586=CARTESIAN_POINT('Ctrl Pts',(-18.0734989461686,-0.0025451719823722,
2.79157655284932));
#82587=CARTESIAN_POINT('Origin',(-15.,0.,8.20842344717746));
#82588=CARTESIAN_POINT('',(-13.1255958151414,2.44015351965519,4.43742368090164));
#82589=CARTESIAN_POINT('',(-13.1276888212995,2.43738653071546,4.35414767240703));
#82590=CARTESIAN_POINT('',(-13.1276888212995,2.43738653071547,8.20842344717746));
#82591=CARTESIAN_POINT('',(-18.073499953472,0.000534796702364866,3.70842344715139));
#82592=CARTESIAN_POINT('Ctrl Pts',(-13.1276888212995,2.43738653071546,4.35414767240703));
#82593=CARTESIAN_POINT('Ctrl Pts',(-13.0511512711489,2.37859318426367,4.34916457209983));
#82594=CARTESIAN_POINT('Ctrl Pts',(-12.9773717129505,2.31618058657907,4.34418147179263));
#82595=CARTESIAN_POINT('Ctrl Pts',(-12.9067013923136,2.25044510909689,4.33919837148543));
#82596=CARTESIAN_POINT('Ctrl Pts',(-12.8360235558487,2.18470264061002,4.33421474122274));
#82597=CARTESIAN_POINT('Ctrl Pts',(-12.7684559346109,2.11563688957496,4.32923111096004));
#82598=CARTESIAN_POINT('Ctrl Pts',(-12.7043138542653,2.04358199499847,4.32424748069735));
#82599=CARTESIAN_POINT('Ctrl Pts',(-12.6401056992207,1.9714528744934,4.31925871664622));
#82600=CARTESIAN_POINT('Ctrl Pts',(-12.5793304249195,1.8963287890356,4.3142699525951));
#82601=CARTESIAN_POINT('Ctrl Pts',(-12.5222637472399,1.81857782669818,4.30928118854398));
#82602=CARTESIAN_POINT('Ctrl Pts',(-12.4651672554918,1.74078624393895,4.30428981814955));
#82603=CARTESIAN_POINT('Ctrl Pts',(-12.4117834624104,1.66036541632739,4.29929844775512));
#82604=CARTESIAN_POINT('Ctrl Pts',(-12.3623441210296,1.5777115433858,4.29430707736069));
#82605=CARTESIAN_POINT('Ctrl Pts',(-12.3128213942626,1.49491826476197,4.28930728842071));
#82606=CARTESIAN_POINT('Ctrl Pts',(-12.2672566178983,1.40988480347299,4.28430749948072));
#82607=CARTESIAN_POINT('Ctrl Pts',(-12.2258351047685,1.32303113495693,4.27930771054073));
#82608=CARTESIAN_POINT('Ctrl Pts',(-12.1909618148304,1.24990794520622,4.27509832570277));
#82609=CARTESIAN_POINT('Ctrl Pts',(-12.1590245475239,1.17549506976768,4.27088894086482));
#82610=CARTESIAN_POINT('Ctrl Pts',(-12.1301065846113,1.10005183255543,4.26667955602686));
#82611=CARTESIAN_POINT('Ctrl Pts',(-12.0957512667359,1.01042323721447,4.2616786936008));
#82612=CARTESIAN_POINT('Ctrl Pts',(-12.0655387715763,0.919027325800495,
4.25667783117473));
#82613=CARTESIAN_POINT('Ctrl Pts',(-12.0396521966435,0.826282719873983,
4.25167696874867));
#82614=CARTESIAN_POINT('Ctrl Pts',(-12.0138005845027,0.733663376187409,
4.24668286056155));
#82615=CARTESIAN_POINT('Ctrl Pts',(-11.9922633974088,0.639699377256914,
4.24168875237442));
#82616=CARTESIAN_POINT('Ctrl Pts',(-11.9751753244573,0.5448283511603,4.2366946441873));
#82617=CARTESIAN_POINT('Ctrl Pts',(-11.9581051869753,0.450056900738318,
4.2317057777659));
#82618=CARTESIAN_POINT('Ctrl Pts',(-11.9454749576285,0.354380745180614,
4.22671691134449));
#82619=CARTESIAN_POINT('Ctrl Pts',(-11.9373689680756,0.258250677238143,
4.22172804492308));
#82620=CARTESIAN_POINT('Ctrl Pts',(-11.9292687342535,0.162188867314636,
4.21674272089113));
#82621=CARTESIAN_POINT('Ctrl Pts',(-11.92568639063,0.0656742216298454,4.21175739685917));
#82622=CARTESIAN_POINT('Ctrl Pts',(-11.9266546833621,-0.0308352833618727,
4.20677207282722));
#82623=CARTESIAN_POINT('Ctrl Pts',(-11.9276226271257,-0.12731000674011,
4.20178854548476));
#82624=CARTESIAN_POINT('Ctrl Pts',(-11.9331379441961,-0.223779154894447,
4.1968050181423));
#82625=CARTESIAN_POINT('Ctrl Pts',(-11.9431812820208,-0.319783638436798,
4.19182149079983));
#82626=CARTESIAN_POINT('Ctrl Pts',(-11.9532237376579,-0.415779689129582,
4.18683840120085));
#82627=CARTESIAN_POINT('Ctrl Pts',(-11.9677933774015,-0.511310720091047,
4.18185531160186));
#82628=CARTESIAN_POINT('Ctrl Pts',(-11.9868189728695,-0.605922724232127,
4.17687222200288));
#82629=CARTESIAN_POINT('Ctrl Pts',(-12.0058480826578,-0.700552204666182,
4.17188821195057));
#82630=CARTESIAN_POINT('Ctrl Pts',(-12.0293346963251,-0.794261891087647,
4.16690420189826));
#82631=CARTESIAN_POINT('Ctrl Pts',(-12.0571566868773,-0.8866089805598,4.16192019184595));
#82632=CARTESIAN_POINT('Ctrl Pts',(-12.0850085633729,-0.979055267818368,
4.15693082804869));
#82633=CARTESIAN_POINT('Ctrl Pts',(-12.1172049870273,-1.07013561539728,
4.15194146425142));
#82634=CARTESIAN_POINT('Ctrl Pts',(-12.1535743170824,-1.15942359887452,
4.14695210045415));
#82635=CARTESIAN_POINT('Ctrl Pts',(-12.1899652045813,-1.24876450663385,
4.14195977927687));
#82636=CARTESIAN_POINT('Ctrl Pts',(-12.2305337391959,-1.33631053705219,
4.1369674580996));
#82637=CARTESIAN_POINT('Ctrl Pts',(-12.2750615074182,-1.42165834912823,
4.13197513692233));
#82638=CARTESIAN_POINT('Ctrl Pts',(-12.3196605552928,-1.50714278521692,
4.12697482408206));
#82639=CARTESIAN_POINT('Ctrl Pts',(-12.3682312708503,-1.59042159816994,
4.12197451124179));
#82640=CARTESIAN_POINT('Ctrl Pts',(-12.4205110314977,-1.67111905960488,
4.11697419840152));
#82641=CARTESIAN_POINT('Ctrl Pts',(-12.4495063995669,-1.71587543506627,
4.11420092802939));
#82642=CARTESIAN_POINT('Ctrl Pts',(-12.4796419345662,-1.75983833668275,
4.11142765765726));
#82643=CARTESIAN_POINT('Ctrl Pts',(-12.5108675909139,-1.8029481689825,4.10865438728513));
#82644=CARTESIAN_POINT('Ctrl Pts',(-12.5671750600055,-1.88068570387152,
4.10365350486901));
#82645=CARTESIAN_POINT('Ctrl Pts',(-12.6272259494741,-1.95591853358483,
4.09865262245288));
#82646=CARTESIAN_POINT('Ctrl Pts',(-12.6907696301558,-2.02826461513016,
4.09365174003675));
#82647=CARTESIAN_POINT('Ctrl Pts',(-12.7542274917857,-2.10051298952278,
4.0886576115729));
#82648=CARTESIAN_POINT('Ctrl Pts',(-12.8211684822821,-2.16988203751743,
4.08366348310905));
#82649=CARTESIAN_POINT('Ctrl Pts',(-12.8912996089411,-2.23601988156365,
4.07866935464519));
#82650=CARTESIAN_POINT('Ctrl Pts',(-12.9613571305786,-2.30208831167549,
4.07368046769035));
#82651=CARTESIAN_POINT('Ctrl Pts',(-13.0345978148429,-2.36493198020902,
4.06869158073551));
#82652=CARTESIAN_POINT('Ctrl Pts',(-13.110690134037,-2.42423399868385,4.06370269378066));
#82653=CARTESIAN_POINT('Ctrl Pts',(-13.1867284279504,-2.48349391293289,
4.05871734891811));
#82654=CARTESIAN_POINT('Ctrl Pts',(-13.2656139867963,-2.53921690713262,
4.05373200405557));
#82655=CARTESIAN_POINT('Ctrl Pts',(-13.3469810867659,-2.59112537760918,
4.04874665919302));
#82656=CARTESIAN_POINT('Ctrl Pts',(-13.4283188653751,-2.64301514240534,
4.04376311084397));
#82657=CARTESIAN_POINT('Ctrl Pts',(-13.5121360388378,-2.69109287903848,
4.03877956249492));
#82658=CARTESIAN_POINT('Ctrl Pts',(-13.5980374918523,-2.7351240146926,4.03379601414586));
#82659=CARTESIAN_POINT('Ctrl Pts',(-13.683931402068,-2.77915128407923,4.02881290339013));
#82660=CARTESIAN_POINT('Ctrl Pts',(-13.7719088374825,-2.81913245905102,
4.0238297926344));
#82661=CARTESIAN_POINT('Ctrl Pts',(-13.8615506022402,-2.85487919512199,
4.01884668187867));
#82662=CARTESIAN_POINT('Ctrl Pts',(-13.9512089273806,-2.89063253503024,
4.01386265054512));
#82663=CARTESIAN_POINT('Ctrl Pts',(-14.0425317850346,-2.92214971997824,
4.00887861921156));
#82664=CARTESIAN_POINT('Ctrl Pts',(-14.1350815603233,-2.94929115936477,
4.00389458787801));
#82665=CARTESIAN_POINT('Ctrl Pts',(-14.2277307518254,-2.97646175386402,
3.99890520273866));
#82666=CARTESIAN_POINT('Ctrl Pts',(-14.3216090704307,-2.99924709549927,
3.99391581759931));
#82667=CARTESIAN_POINT('Ctrl Pts',(-14.4162655728082,-3.0175580141086,3.98892643245996));
#82668=CARTESIAN_POINT('Ctrl Pts',(-14.5109781825905,-3.03587978646911,
3.98393408987506));
#82669=CARTESIAN_POINT('Ctrl Pts',(-14.6064694607048,-3.0497217918892,3.97894174729016));
#82670=CARTESIAN_POINT('Ctrl Pts',(-14.7022822487487,-3.059046647338,3.97394940470526));
#82671=CARTESIAN_POINT('Ctrl Pts',(-14.7982484103532,-3.06838642966986,
3.96894907056335));
#82672=CARTESIAN_POINT('Ctrl Pts',(-14.894536671744,-3.07319460225313,3.96394873642144));
#82673=CARTESIAN_POINT('Ctrl Pts',(-14.9906888535839,-3.07348589594168,
3.95894840227953));
#82674=CARTESIAN_POINT('Ctrl Pts',(-15.0440124678769,-3.07364744019369,
3.95617534103415));
#82675=CARTESIAN_POINT('Ctrl Pts',(-15.0972942896739,-3.07242073009662,
3.95340227978877));
#82676=CARTESIAN_POINT('Ctrl Pts',(-15.1504570808492,-3.06981512746653,
3.95062921854339));
#82677=CARTESIAN_POINT('Ctrl Pts',(-15.2463296764332,-3.06511624161639,
3.94562834154971));
#82678=CARTESIAN_POINT('Ctrl Pts',(-15.3421491860804,-3.05591359807456,
3.94062746455604));
#82679=CARTESIAN_POINT('Ctrl Pts',(-15.4374586967929,-3.04220843115659,
3.93562658756236));
#82680=CARTESIAN_POINT('Ctrl Pts',(-15.5326394861444,-3.02852177391017,
3.93063246456089));
#82681=CARTESIAN_POINT('Ctrl Pts',(-15.6273112149682,-3.01034474089706,
3.92563834155943));
#82682=CARTESIAN_POINT('Ctrl Pts',(-15.7210190955906,-2.98773052897909,
3.92064421855796));
#82683=CARTESIAN_POINT('Ctrl Pts',(-15.8146286258718,-2.96514005162267,
3.91565533709753));
#82684=CARTESIAN_POINT('Ctrl Pts',(-15.9072758947998,-2.93812175576487,
3.9106664556371));
#82685=CARTESIAN_POINT('Ctrl Pts',(-15.9985143717709,-2.90678022894182,
3.90567757417667));
#82686=CARTESIAN_POINT('Ctrl Pts',(-16.0896880692237,-2.87546095467138,
3.900692234833));
#82687=CARTESIAN_POINT('Ctrl Pts',(-16.1794545494874,-2.83982469366955,
3.89570689548932));
#82688=CARTESIAN_POINT('Ctrl Pts',(-16.2673815073807,-2.80002613644041,
3.89072155614564));
#82689=CARTESIAN_POINT('Ctrl Pts',(-16.3552767797466,-2.76024192109577,
3.88573801332842));
#82690=CARTESIAN_POINT('Ctrl Pts',(-16.4413334476389,-2.71629857051968,
3.8807544705112));
#82691=CARTESIAN_POINT('Ctrl Pts',(-16.5251391936413,-2.66839890009331,
3.87577092769398));
#82692=CARTESIAN_POINT('Ctrl Pts',(-16.6089375807544,-2.62050343568367,
3.8707878224761));
#82693=CARTESIAN_POINT('Ctrl Pts',(-16.6904850582122,-2.56865256000697,
3.86580471725823));
#82694=CARTESIAN_POINT('Ctrl Pts',(-16.7693948757914,-2.51309451145853,
3.86082161204035));
#82695=CARTESIAN_POINT('Ctrl Pts',(-16.8483192711681,-2.45752619911783,
3.85583758624376));
#82696=CARTESIAN_POINT('Ctrl Pts',(-16.9246046802542,-2.39824960630894,
3.85085356044718));
#82697=CARTESIAN_POINT('Ctrl Pts',(-16.9978951281539,-2.33555503187123,
3.84586953465059));
#82698=CARTESIAN_POINT('Ctrl Pts',(-17.0712643046609,-2.27279311091465,
3.84088015501293));
#82699=CARTESIAN_POINT('Ctrl Pts',(-17.1416317634431,-2.20660616412503,
3.83589077537528));
#82700=CARTESIAN_POINT('Ctrl Pts',(-17.2086764816553,-2.13732319722186,
3.83090139573762));
#82701=CARTESIAN_POINT('Ctrl Pts',(-17.2757609406612,-2.06799916280183,
3.82590905864243));
#82702=CARTESIAN_POINT('Ctrl Pts',(-17.3395184476431,-1.99557578320459,
3.82091672154724));
#82703=CARTESIAN_POINT('Ctrl Pts',(-17.3996679623523,-1.92041555931523,
3.81592438445205));
#82704=CARTESIAN_POINT('Ctrl Pts',(-17.4599137631578,-1.84513502049751,
3.81092405572713));
#82705=CARTESIAN_POINT('Ctrl Pts',(-17.5165397820994,-1.76710924441421,
3.80592372700221));
#82706=CARTESIAN_POINT('Ctrl Pts',(-17.569308072578,-1.68673005492445,3.80092339827729));
#82707=CARTESIAN_POINT('Ctrl Pts',(-17.5985726683746,-1.64215281981712,
3.79815028211875));
#82708=CARTESIAN_POINT('Ctrl Pts',(-17.6266515660431,-1.59685221102482,
3.7953771659602));
#82709=CARTESIAN_POINT('Ctrl Pts',(-17.6535104129204,-1.55089804259443,
3.79260404980166));
#82710=CARTESIAN_POINT('Ctrl Pts',(-17.7037312761393,-1.46497261111064,
3.78741885745423));
#82711=CARTESIAN_POINT('Ctrl Pts',(-17.7498481749421,-1.37648008567004,
3.78223366510681));
#82712=CARTESIAN_POINT('Ctrl Pts',(-17.7916008762206,-1.28583311432093,
3.77704847275938));
#82713=CARTESIAN_POINT('Ctrl Pts',(-17.8332824144256,-1.19534064116923,
3.77187211802516));
#82714=CARTESIAN_POINT('Ctrl Pts',(-17.8706143949755,-1.1027013849238,3.76669576329094));
#82715=CARTESIAN_POINT('Ctrl Pts',(-17.9033815283408,-1.00835408011737,
3.76151940855672));
#82716=CARTESIAN_POINT('Ctrl Pts',(-17.9360830256386,-0.914195763038406,
3.75635342261384));
#82717=CARTESIAN_POINT('Ctrl Pts',(-17.9642377647595,-0.818336583660731,
3.75118743667097));
#82718=CARTESIAN_POINT('Ctrl Pts',(-17.98767825096,-0.721235688759529,3.74602145072809));
#82719=CARTESIAN_POINT('Ctrl Pts',(-18.0110906840712,-0.624251002202372,
3.74086164733042));
#82720=CARTESIAN_POINT('Ctrl Pts',(-18.0297999980823,-0.52602793756912,
3.73570184393275));
#82721=CARTESIAN_POINT('Ctrl Pts',(-18.0436881725886,-0.42704163502405,
3.73054204053508));
#82722=CARTESIAN_POINT('Ctrl Pts',(-18.0575581431002,-0.32818507927451,
3.72538900037574));
#82723=CARTESIAN_POINT('Ctrl Pts',(-18.0666195076493,-0.228567666925236,
3.72023596021641));
#82724=CARTESIAN_POINT('Ctrl Pts',(-18.0708052822106,-0.128674662414667,
3.71508292005708));
#82725=CARTESIAN_POINT('Ctrl Pts',(-18.07260842827,-0.0856427994216626,
3.71286309576387));
#82726=CARTESIAN_POINT('Ctrl Pts',(-18.0735074520523,-0.0425599117334144,
3.71064327147067));
#82727=CARTESIAN_POINT('Ctrl Pts',(-18.0734999534721,0.000534796196229549,
3.70842344717746));
#82728=CARTESIAN_POINT('Ctrl Pts',(-18.073499953472,0.000534796702359477,
3.70842344715139));
#82729=CARTESIAN_POINT('Ctrl Pts',(-18.0734820740241,0.10328876314218,3.70313055245769));
#82730=CARTESIAN_POINT('Ctrl Pts',(-18.0683069955294,0.205917074353121,
3.69783765776399));
#82731=CARTESIAN_POINT('Ctrl Pts',(-18.0580378511336,0.307907049341914,
3.69254476307029));
#82732=CARTESIAN_POINT('Ctrl Pts',(-18.0477346931935,0.410234836361457,
3.68723433720743));
#82733=CARTESIAN_POINT('Ctrl Pts',(-18.0323037584543,0.511919708943151,
3.68192391134456));
#82734=CARTESIAN_POINT('Ctrl Pts',(-18.0118597534527,0.612456590732762,
3.67661348548169));
#82735=CARTESIAN_POINT('Ctrl Pts',(-17.9913808082723,0.713165296811276,
3.67129398374407));
#82736=CARTESIAN_POINT('Ctrl Pts',(-17.9658717804935,0.812721758175001,
3.66597448200644));
#82737=CARTESIAN_POINT('Ctrl Pts',(-17.9354972645245,0.910636074383762,
3.66065498026882));
#82738=CARTESIAN_POINT('Ctrl Pts',(-17.9050354164564,1.00883191154829,3.655320184024));
#82739=CARTESIAN_POINT('Ctrl Pts',(-17.8696802228789,1.10537583161873,3.64998538777918));
#82740=CARTESIAN_POINT('Ctrl Pts',(-17.8296450073608,1.19979639202571,3.64465059153437));
#82741=CARTESIAN_POINT('Ctrl Pts',(-17.8044504744005,1.25921612763904,3.64129335470955));
#82742=CARTESIAN_POINT('Ctrl Pts',(-17.7774034483836,1.31779541931844,3.63793611788474));
#82743=CARTESIAN_POINT('Ctrl Pts',(-17.7485661821547,1.37542218693584,3.63457888105992));
#82744=CARTESIAN_POINT('Ctrl Pts',(-17.7056107277124,1.46126194620451,3.62957800364192));
#82745=CARTESIAN_POINT('Ctrl Pts',(-17.6585552263764,1.5452372290436,3.62457712622393));
#82746=CARTESIAN_POINT('Ctrl Pts',(-17.6075850331202,1.62693040571727,3.61957624880593));
#82747=CARTESIAN_POINT('Ctrl Pts',(-17.5566836783714,1.70851325052866,3.61458212539287));
#82748=CARTESIAN_POINT('Ctrl Pts',(-17.5018783698048,1.78781974580175,3.60958800197981));
#82749=CARTESIAN_POINT('Ctrl Pts',(-17.4434011571114,1.86445515779451,3.60459387856674));
#82750=CARTESIAN_POINT('Ctrl Pts',(-17.3849853188495,1.94101013751939,3.59960499670797));
#82751=CARTESIAN_POINT('Ctrl Pts',(-17.3229055025035,2.01489926020094,3.59461611484919));
#82752=CARTESIAN_POINT('Ctrl Pts',(-17.2574374568609,2.08575606875809,3.58962723299042));
#82753=CARTESIAN_POINT('Ctrl Pts',(-17.1920158939542,2.15656256852296,3.58464189327002));
#82754=CARTESIAN_POINT('Ctrl Pts',(-17.1232111810246,2.2243407129309,3.57965655354963));
#82755=CARTESIAN_POINT('Ctrl Pts',(-17.051339181143,2.28875726408626,3.57467121382924));
#82756=CARTESIAN_POINT('Ctrl Pts',(-16.9794930813869,2.35315060179599,3.56968767064887));
#82757=CARTESIAN_POINT('Ctrl Pts',(-16.904582217274,2.41418446075199,3.5647041274685));
#82758=CARTESIAN_POINT('Ctrl Pts',(-16.8269584326305,2.47156329788257,3.55972058428813));
#82759=CARTESIAN_POINT('Ctrl Pts',(-16.7493414642639,2.52893709647962,3.55473747872119));
#82760=CARTESIAN_POINT('Ctrl Pts',(-16.669012401906,2.58265625080491,3.54975437315425));
#82761=CARTESIAN_POINT('Ctrl Pts',(-16.5863543480257,2.63246692904201,3.54477126758731));
#82762=CARTESIAN_POINT('Ctrl Pts',(-16.5036810241425,2.68228680915558,3.53978724145627));
#82763=CARTESIAN_POINT('Ctrl Pts',(-16.4186782299777,2.72819655280745,3.53480321532523));
#82764=CARTESIAN_POINT('Ctrl Pts',(-16.3317551496124,2.76998744969738,3.52981918919419));
#82765=CARTESIAN_POINT('Ctrl Pts',(-16.2447386968974,2.81182323816522,3.52482980924656));
#82766=CARTESIAN_POINT('Ctrl Pts',(-16.1557982359609,2.84953115671571,3.51984042929892));
#82767=CARTESIAN_POINT('Ctrl Pts',(-16.0653642795656,2.88295008659979,3.51485104935129));
#82768=CARTESIAN_POINT('Ctrl Pts',(-15.9748767186394,2.91638882548182,3.50985871195955));
#82769=CARTESIAN_POINT('Ctrl Pts',(-15.8828943174917,2.9455333811086,3.50486637456781));
#82770=CARTESIAN_POINT('Ctrl Pts',(-15.7898621199645,2.970272728462,3.49987403717607));
#82771=CARTESIAN_POINT('Ctrl Pts',(-15.6966809988829,2.99505167792781,3.49487370817874));
#82772=CARTESIAN_POINT('Ctrl Pts',(-15.6024471544208,3.01541124633234,3.48987337918141));
#82773=CARTESIAN_POINT('Ctrl Pts',(-15.5076150891051,3.03129166714667,3.48487305018409));
#82774=CARTESIAN_POINT('Ctrl Pts',(-15.4550225502073,3.04009872672732,3.48209993756212));
#82775=CARTESIAN_POINT('Ctrl Pts',(-15.4022461111601,3.04752907982357,3.47932682494016));
#82776=CARTESIAN_POINT('Ctrl Pts',(-15.349363510309,3.05357943857117,3.47655371231819));
#82777=CARTESIAN_POINT('Ctrl Pts',(-15.252196107347,3.06469647209504,3.47145834735391));
#82778=CARTESIAN_POINT('Ctrl Pts',(-15.1543248192937,3.07119073472823,3.46636298238962));
#82779=CARTESIAN_POINT('Ctrl Pts',(-15.0562268722244,3.07298564735338,3.46126761742533));
#82780=CARTESIAN_POINT('Ctrl Pts',(-14.9600958654314,3.0747445705818,3.45627441849887));
#82781=CARTESIAN_POINT('Ctrl Pts',(-14.863747667448,3.07199079205801,3.45128121957241));
#82782=CARTESIAN_POINT('Ctrl Pts',(-14.7676395103559,3.06470404000979,3.44628802064595));
#82783=CARTESIAN_POINT('Ctrl Pts',(-14.6716232941742,3.05742425876029,3.44129959841347));
#82784=CARTESIAN_POINT('Ctrl Pts',(-14.5758470974853,3.04562015302896,3.43631117618099));
#82785=CARTESIAN_POINT('Ctrl Pts',(-14.4807683425551,3.029323478255,3.43132275394852));
#82786=CARTESIAN_POINT('Ctrl Pts',(-14.3857546256464,3.01303795111846,3.42633774401475));
#82787=CARTESIAN_POINT('Ctrl Pts',(-14.2914378332587,2.99226603700626,3.42135273408098));
#82788=CARTESIAN_POINT('Ctrl Pts',(-14.198269390584,2.96709121530254,3.41636772414722));
#82789=CARTESIAN_POINT('Ctrl Pts',(-14.1015457709371,2.94095575774583,3.41119249323289));
#82790=CARTESIAN_POINT('Ctrl Pts',(-14.006060382732,2.9100747143353,3.40601726231856));
#82791=CARTESIAN_POINT('Ctrl Pts',(-13.9123050577016,2.87459944383534,3.40084203140424));
#82792=CARTESIAN_POINT('Ctrl Pts',(-13.8220234257243,2.84043855415217,3.39585854601124));
#82793=CARTESIAN_POINT('Ctrl Pts',(-13.7333463505172,2.80201804783541,3.39087506061824));
#82794=CARTESIAN_POINT('Ctrl Pts',(-13.6466946169307,2.75952292799963,3.38589157522524));
#82795=CARTESIAN_POINT('Ctrl Pts',(-13.5600346086623,2.71702375015389,3.38090761394151));
#82796=CARTESIAN_POINT('Ctrl Pts',(-13.4754007165344,2.67044938602366,3.37592365265779));
#82797=CARTESIAN_POINT('Ctrl Pts',(-13.3931897327425,2.62003110955497,3.37093969137406));
#82798=CARTESIAN_POINT('Ctrl Pts',(-13.3109254881076,2.56958016932551,3.3659525012033));
#82799=CARTESIAN_POINT('Ctrl Pts',(-13.2310876511612,2.5152805872233,3.36096531103255));
#82800=CARTESIAN_POINT('Ctrl Pts',(-13.154044028865,2.45740692654494,3.35597812086179));
#82801=CARTESIAN_POINT('Ctrl Pts',(-13.1452221846569,2.45078012989336,3.35540706496629));
#82802=CARTESIAN_POINT('Ctrl Pts',(-13.1364369407639,2.44410651610121,3.35483600907079));
#82803=CARTESIAN_POINT('Ctrl Pts',(-13.1276888212995,2.43738653071547,3.3542649531753));
#82804=CARTESIAN_POINT('',(-18.0739720314691,0.000457053523349289,3.79157660465044));
#82805=CARTESIAN_POINT('Ctrl Pts',(-18.0734999658784,0.000457979655525854,
3.79157655282255));
#82806=CARTESIAN_POINT('Ctrl Pts',(-18.0734962197828,0.0255980150809229,
3.79026691442027));
#82807=CARTESIAN_POINT('Ctrl Pts',(-18.0731840258867,0.0507354218780576,
3.78895727601798));
#82808=CARTESIAN_POINT('Ctrl Pts',(-18.0725635426613,0.0758651850894085,
3.7876476376157));
#82809=CARTESIAN_POINT('Ctrl Pts',(-18.0701942141197,0.171823726401515,
3.78264675520893));
#82810=CARTESIAN_POINT('Ctrl Pts',(-18.0633211566005,0.267838563984851,
3.77764587280217));
#82811=CARTESIAN_POINT('Ctrl Pts',(-18.0519345090764,0.363452888705755,
3.77264499039541));
#82812=CARTESIAN_POINT('Ctrl Pts',(-18.0405632398134,0.458938081296764,
3.76765086194103));
#82813=CARTESIAN_POINT('Ctrl Pts',(-18.0246905473028,0.554023404166364,
3.76265673348665));
#82814=CARTESIAN_POINT('Ctrl Pts',(-18.0043585693512,0.648252911112749,
3.75766260503227));
#82815=CARTESIAN_POINT('Ctrl Pts',(-17.9840479305078,0.742383520959695,
3.752673718087));
#82816=CARTESIAN_POINT('Ctrl Pts',(-17.9592874023539,0.835659673953074,
3.74768483114172));
#82817=CARTESIAN_POINT('Ctrl Pts',(-17.9301706987204,0.927632430632183,
3.74269594419645));
#82818=CARTESIAN_POINT('Ctrl Pts',(-17.9010746678452,1.01953988697378,3.73771059934356));
#82819=CARTESIAN_POINT('Ctrl Pts',(-17.8676287420875,1.11014536966332,3.73272525449067));
#82820=CARTESIAN_POINT('Ctrl Pts',(-17.8299770689057,1.19901294382832,3.72773990963779));
#82821=CARTESIAN_POINT('Ctrl Pts',(-17.7923389638407,1.28784849376909,3.72275636129845));
#82822=CARTESIAN_POINT('Ctrl Pts',(-17.7504982936859,1.37494697604483,3.71777281295912));
#82823=CARTESIAN_POINT('Ctrl Pts',(-17.7046478019502,1.45989126903539,3.71278926461978));
#82824=CARTESIAN_POINT('Ctrl Pts',(-17.6588013362356,1.54482810327242,3.70780615387381));
#82825=CARTESIAN_POINT('Ctrl Pts',(-17.6089459575431,1.62761073838789,3.70282304312784));
#82826=CARTESIAN_POINT('Ctrl Pts',(-17.5553204398576,1.70784650939308,3.69783993238187));
#82827=CARTESIAN_POINT('Ctrl Pts',(-17.5016850154166,1.78809710312076,3.69285590105812));
#82828=CARTESIAN_POINT('Ctrl Pts',(-17.4442783125023,1.86579953361445,3.68787186973437));
#82829=CARTESIAN_POINT('Ctrl Pts',(-17.383381900477,1.94059088075737,3.68288783841062));
#82830=CARTESIAN_POINT('Ctrl Pts',(-17.3224200740224,2.01546256815557,3.67789845328106));
#82831=CARTESIAN_POINT('Ctrl Pts',(-17.2579613322987,2.08741658875113,3.6729090681515));
#82832=CARTESIAN_POINT('Ctrl Pts',(-17.190326788901,2.15612402422093,3.66791968302194));
#82833=CARTESIAN_POINT('Ctrl Pts',(-17.122652155297,2.22487218585111,3.66292734044684));
#82834=CARTESIAN_POINT('Ctrl Pts',(-17.0517982936774,2.29036963290002,3.65793499787174));
#82835=CARTESIAN_POINT('Ctrl Pts',(-16.9781207738701,2.35232660444579,3.65294265529663));
#82836=CARTESIAN_POINT('Ctrl Pts',(-16.9043253138179,2.41438275441689,3.64794232116444));
#82837=CARTESIAN_POINT('Ctrl Pts',(-16.8276975188581,2.47288684667339,3.64294198703224));
#82838=CARTESIAN_POINT('Ctrl Pts',(-16.7486233196402,2.5275914891474,3.63794165290004));
#82839=CARTESIAN_POINT('Ctrl Pts',(-16.7047707291522,2.55792932763249,3.63516859155802));
#82840=CARTESIAN_POINT('Ctrl Pts',(-16.6601662150027,2.58709942991981,3.63239553021599));
#82841=CARTESIAN_POINT('Ctrl Pts',(-16.6148787322104,2.6150657602161,3.62962246887397));
#82842=CARTESIAN_POINT('Ctrl Pts',(-16.5332082955066,2.66549961671397,3.62462159188003));
#82843=CARTESIAN_POINT('Ctrl Pts',(-16.4490304917344,2.71219184764961,3.6196207148861));
#82844=CARTESIAN_POINT('Ctrl Pts',(-16.3627225629527,2.75488465573779,3.61461983789216));
#82845=CARTESIAN_POINT('Ctrl Pts',(-16.2765311983419,2.79751980456053,3.60962571489045));
#82846=CARTESIAN_POINT('Ctrl Pts',(-16.1882158162888,2.83616607295716,3.60463159188875));
#82847=CARTESIAN_POINT('Ctrl Pts',(-16.0981813411113,2.87060968995003,3.59963746888704));
#82848=CARTESIAN_POINT('Ctrl Pts',(-16.0082413608828,2.90501715692566,3.59464858742639));
#82849=CARTESIAN_POINT('Ctrl Pts',(-15.9165862819263,2.93523058528095,3.58965970596574));
#82850=CARTESIAN_POINT('Ctrl Pts',(-15.8236433337036,2.96108323234008,3.58467082450508));
#82851=CARTESIAN_POINT('Ctrl Pts',(-15.7307663751782,2.98691752396303,3.57968548516122));
#82852=CARTESIAN_POINT('Ctrl Pts',(-15.6366037866106,3.00839707218904,3.57470014581736));
#82853=CARTESIAN_POINT('Ctrl Pts',(-15.5415994546647,3.02540448216546,3.5697148064735));
#82854=CARTESIAN_POINT('Ctrl Pts',(-15.4466293586627,3.04240576331889,3.56473126365612));
#82855=CARTESIAN_POINT('Ctrl Pts',(-15.3508185533612,3.05493803114046,3.55974772083874));
#82856=CARTESIAN_POINT('Ctrl Pts',(-15.2546217133959,3.06293487248217,3.55476417802136));
#82857=CARTESIAN_POINT('Ctrl Pts',(-15.1584333203684,3.07093101163011,3.54978107280335));
#82858=CARTESIAN_POINT('Ctrl Pts',(-15.0618593972539,3.07439247999359,3.54479796758533));
#82859=CARTESIAN_POINT('Ctrl Pts',(-14.9653592781951,3.0733047799385,3.53981486236732));
#82860=CARTESIAN_POINT('Ctrl Pts',(-14.8688413317076,3.07221687894174,3.53483083657062));
#82861=CARTESIAN_POINT('Ctrl Pts',(-14.7723976549859,3.06657814541914,3.52984681077392));
#82862=CARTESIAN_POINT('Ctrl Pts',(-14.6764860449469,3.05642617625322,3.52486278497722));
#82863=CARTESIAN_POINT('Ctrl Pts',(-14.580471406646,3.04626330184093,3.51987340533946));
#82864=CARTESIAN_POINT('Ctrl Pts',(-14.4849904129745,3.0315775594591,3.51488402570171));
#82865=CARTESIAN_POINT('Ctrl Pts',(-14.3904939819799,3.01245824269769,3.50989464606396));
#82866=CARTESIAN_POINT('Ctrl Pts',(-14.2959415381741,2.99332759295082,3.5049023089687));
#82867=CARTESIAN_POINT('Ctrl Pts',(-14.2023752442585,2.96975824309058,3.49990997187344));
#82868=CARTESIAN_POINT('Ctrl Pts',(-14.1102320415969,2.94188973794042,3.49491763477818));
#82869=CARTESIAN_POINT('Ctrl Pts',(-14.0179413380071,2.9139766214651,3.48991730605321));
#82870=CARTESIAN_POINT('Ctrl Pts',(-13.9270786873677,2.88175075492031,3.48491697732825));
#82871=CARTESIAN_POINT('Ctrl Pts',(-13.8380621272317,2.84540025828118,3.47991664860329));
#82872=CARTESIAN_POINT('Ctrl Pts',(-13.7886947206603,2.82524075375853,3.47714353244627));
#82873=CARTESIAN_POINT('Ctrl Pts',(-13.7398947013448,2.80381348694063,3.47437041628924));
#82874=CARTESIAN_POINT('Ctrl Pts',(-13.6917299249556,2.78115653294512,3.47159730013222));
#82875=CARTESIAN_POINT('Ctrl Pts',(-13.6048646115275,2.74029465092907,3.46659597712793));
#82876=CARTESIAN_POINT('Ctrl Pts',(-13.5197639714094,2.6952879144502,3.46159465412364));
#82877=CARTESIAN_POINT('Ctrl Pts',(-13.4368501248134,2.64631153073559,3.45659333111934));
#82878=CARTESIAN_POINT('Ctrl Pts',(-13.3540585553577,2.59740737491035,3.45159938381283));
#82879=CARTESIAN_POINT('Ctrl Pts',(-13.2734477413335,2.54454543399417,3.44660543650632));
#82880=CARTESIAN_POINT('Ctrl Pts',(-13.1954178916597,2.48794808311147,3.4416114891998));
#82881=CARTESIAN_POINT('Ctrl Pts',(-13.1726181386746,2.47141074996104,3.44015229421884));
#82882=CARTESIAN_POINT('Ctrl Pts',(-13.1500385872511,2.45455480341457,3.43869309923789));
#82883=CARTESIAN_POINT('Ctrl Pts',(-13.1276888212995,2.43738653071547,3.43723390425693));
#82884=CARTESIAN_POINT('Ctrl Pts',(-13.1255958151414,2.44015351965519,4.43742368090164));
#82885=CARTESIAN_POINT('Ctrl Pts',(-13.0351160055007,2.37176328111156,4.43153189146197));
#82886=CARTESIAN_POINT('Ctrl Pts',(-12.1759702308937,1.6408111827257,4.37296504577506));
#82887=CARTESIAN_POINT('Ctrl Pts',(-11.436582832353,-0.676361228608103,
4.26172314384091));
#82888=CARTESIAN_POINT('Ctrl Pts',(-13.6199704166047,-3.35423250130061,
4.10369797509917));
#82889=CARTESIAN_POINT('Ctrl Pts',(-17.0272186911122,-2.99125965920794,
3.94698262309378));
#82890=CARTESIAN_POINT('Ctrl Pts',(-18.0762959775521,-0.987130875700585,
3.84294232733563));
#82891=CARTESIAN_POINT('Ctrl Pts',(-18.0783729425329,0.000448419499977877,
3.79157708782474));
#82892=CARTESIAN_POINT('Origin',(-15.,0.,8.20842344717746));
#82893=CARTESIAN_POINT('',(-13.1276888212995,2.43738653071547,5.43736138633702));
#82894=CARTESIAN_POINT('',(-13.1256826865589,2.43995710119903,5.35407232013781));
#82895=CARTESIAN_POINT('',(-13.1276888212995,2.43738653071547,8.20842344717746));
#82896=CARTESIAN_POINT('',(-18.0730476819807,-0.00351971310571451,5.79157674198311));
#82897=CARTESIAN_POINT('Ctrl Pts',(-18.0734979882452,-0.00351656827781883,
5.79157655282255));
#82898=CARTESIAN_POINT('Ctrl Pts',(-18.0736072822651,0.0920069431531279,
5.78664473933955));
#82899=CARTESIAN_POINT('Ctrl Pts',(-18.0692590445082,0.187606130278477,
5.78171292585655));
#82900=CARTESIAN_POINT('Ctrl Pts',(-18.0604590887115,0.282829305984153,
5.77678111237354));
#82901=CARTESIAN_POINT('Ctrl Pts',(-18.0516617025475,0.378024676028252,
5.77185073900568));
#82902=CARTESIAN_POINT('Ctrl Pts',(-18.038415221166,0.472843806578188,5.76692036563781));
#82903=CARTESIAN_POINT('Ctrl Pts',(-18.0207774649557,0.566838387210871,
5.76198999226995));
#82904=CARTESIAN_POINT('Ctrl Pts',(-18.0031398133705,0.660832410278753,
5.75705964814848));
#82905=CARTESIAN_POINT('Ctrl Pts',(-17.9811110222353,0.754001452603219,
5.75212930402701));
#82906=CARTESIAN_POINT('Ctrl Pts',(-17.9548001333951,0.845906863483294,
5.74719895990554));
#82907=CARTESIAN_POINT('Ctrl Pts',(-17.9284818733408,0.937838022427872,
5.7422672345072));
#82908=CARTESIAN_POINT('Ctrl Pts',(-17.8978792574336,1.02850441626493,5.73733550910886));
#82909=CARTESIAN_POINT('Ctrl Pts',(-17.8631509863536,1.11748318973598,5.73240378371051));
#82910=CARTESIAN_POINT('Ctrl Pts',(-17.8283818661184,1.20656662455667,5.72746625736644));
#82911=CARTESIAN_POINT('Ctrl Pts',(-17.7894775723116,1.29395806073367,5.72252873102237));
#82912=CARTESIAN_POINT('Ctrl Pts',(-17.7466445403766,1.37925560314957,5.71759120467829));
#82913=CARTESIAN_POINT('Ctrl Pts',(-17.7037815187446,1.46461286693794,5.71265022130789));
#82914=CARTESIAN_POINT('Ctrl Pts',(-17.6569845067983,1.54787293116407,5.70770923793749));
#82915=CARTESIAN_POINT('Ctrl Pts',(-17.6065042419745,1.62866137873061,5.70276825456709));
#82916=CARTESIAN_POINT('Ctrl Pts',(-17.5559431874896,1.70957912180153,5.69781936354458));
#82917=CARTESIAN_POINT('Ctrl Pts',(-17.5016873762857,1.78801699128002,5.69287047252208));
#82918=CARTESIAN_POINT('Ctrl Pts',(-17.4440286458054,1.8636325357974,5.68792158149958));
#82919=CARTESIAN_POINT('Ctrl Pts',(-17.4286032501567,1.88386190404153,5.68659760850523));
#82920=CARTESIAN_POINT('Ctrl Pts',(-17.4129345076039,1.90388947532135,5.68527363551087));
#82921=CARTESIAN_POINT('Ctrl Pts',(-17.3970284450544,1.92370914735055,5.68394966251652));
#82922=CARTESIAN_POINT('Ctrl Pts',(-17.3368771896634,1.99866032714632,5.67894285222227));
#82923=CARTESIAN_POINT('Ctrl Pts',(-17.2731035294659,2.07091670579144,5.67393604192802));
#82924=CARTESIAN_POINT('Ctrl Pts',(-17.2059776324753,2.14010862692026,5.66892923163378));
#82925=CARTESIAN_POINT('Ctrl Pts',(-17.1389423799006,2.209207113748,5.66392918235747));
#82926=CARTESIAN_POINT('Ctrl Pts',(-17.0685641899493,2.27524905664967,5.65892913308117));
#82927=CARTESIAN_POINT('Ctrl Pts',(-16.9951540132018,2.33789707078918,5.65392908380487));
#82928=CARTESIAN_POINT('Ctrl Pts',(-16.9218210229,2.40047921425854,5.64893429178374));
#82929=CARTESIAN_POINT('Ctrl Pts',(-16.8454627148059,2.45967424103802,5.64393949976261));
#82930=CARTESIAN_POINT('Ctrl Pts',(-16.7664267653277,2.51518165004718,5.63894470774148));
#82931=CARTESIAN_POINT('Ctrl Pts',(-16.6874476518167,2.57064914282447,5.63395350755215));
#82932=CARTESIAN_POINT('Ctrl Pts',(-16.6057950822321,2.62243403946385,5.62896230736282));
#82933=CARTESIAN_POINT('Ctrl Pts',(-16.5218489159773,2.67027678845072,5.62397110717348));
#82934=CARTESIAN_POINT('Ctrl Pts',(-16.4379335277937,2.71810199634431,5.61898173696069));
#82935=CARTESIAN_POINT('Ctrl Pts',(-16.3517265936208,2.76198771227858,5.61399236674789));
#82936=CARTESIAN_POINT('Ctrl Pts',(-16.2636351889554,2.80171882230064,5.60900299653509));
#82937=CARTESIAN_POINT('Ctrl Pts',(-16.1755522383816,2.84144611934632,5.60401410514986));
#82938=CARTESIAN_POINT('Ctrl Pts',(-16.0855855757646,2.87701942363017,5.59902521376464));
#82939=CARTESIAN_POINT('Ctrl Pts',(-15.9941640445155,2.90827098163024,5.59403632237941));
#82940=CARTESIAN_POINT('Ctrl Pts',(-15.9027265423428,2.93952799913467,5.58904655945765));
#82941=CARTESIAN_POINT('Ctrl Pts',(-15.8098340807032,2.9664616294552,5.5840567965359));
#82942=CARTESIAN_POINT('Ctrl Pts',(-15.7159315074474,2.98895371771529,5.57906703361414));
#82943=CARTESIAN_POINT('Ctrl Pts',(-15.6219302684125,3.01146943897431,5.57407202782385));
#82944=CARTESIAN_POINT('Ctrl Pts',(-15.5269172249754,3.02953419920992,5.56907702203356));
#82945=CARTESIAN_POINT('Ctrl Pts',(-15.4313480654783,3.04308085604181,5.56408201624327));
#82946=CARTESIAN_POINT('Ctrl Pts',(-15.3357233712283,3.05663538476712,5.55908410788051));
#82947=CARTESIAN_POINT('Ctrl Pts',(-15.2395423527312,3.06566654080875,5.55408619951775));
#82948=CARTESIAN_POINT('Ctrl Pts',(-15.1432644002756,3.070159207861,5.54908829115498));
#82949=CARTESIAN_POINT('Ctrl Pts',(-15.0468352254713,3.0746589314786,5.54408253265185));
#82950=CARTESIAN_POINT('Ctrl Pts',(-14.9503092498453,3.07460593233485,5.53907677414872));
#82951=CARTESIAN_POINT('Ctrl Pts',(-14.8541443578981,3.07003719548592,5.53407101564558));
#82952=CARTESIAN_POINT('Ctrl Pts',(-14.8019771458789,3.06755876225491,5.53135550835532));
#82953=CARTESIAN_POINT('Ctrl Pts',(-14.7499160909764,3.06375233419271,5.52864000106506));
#82954=CARTESIAN_POINT('Ctrl Pts',(-14.6980331473027,3.05863012962864,5.5259244937748));
#82955=CARTESIAN_POINT('Ctrl Pts',(-14.6023361309739,3.04918232927076,5.52091579675229));
#82956=CARTESIAN_POINT('Ctrl Pts',(-14.5069222957617,3.03522319463142,5.51590709972977));
#82957=CARTESIAN_POINT('Ctrl Pts',(-14.4122491793749,3.01677828533264,5.51089840270726));
#82958=CARTESIAN_POINT('Ctrl Pts',(-14.3176949370156,2.99835653594174,5.50589599473501));
#82959=CARTESIAN_POINT('Ctrl Pts',(-14.2238799907018,2.9754602871356,5.50089358676275));
#82960=CARTESIAN_POINT('Ctrl Pts',(-14.1312570510269,2.94816687767323,5.4958911787905));
#82961=CARTESIAN_POINT('Ctrl Pts',(-14.0387345507126,2.92090306490263,5.49089419537786));
#82962=CARTESIAN_POINT('Ctrl Pts',(-13.9474019031945,2.88925169788506,5.48589721196523));
#82963=CARTESIAN_POINT('Ctrl Pts',(-13.8577007516974,2.85334096759,5.4809002285526));
#82964=CARTESIAN_POINT('Ctrl Pts',(-13.7680578858049,2.81745357120527,5.47590649205702));
#82965=CARTESIAN_POINT('Ctrl Pts',(-13.6800448133697,2.77731247431519,5.47091275556145));
#82966=CARTESIAN_POINT('Ctrl Pts',(-13.5940863736698,2.73309515481974,5.46591901906588));
#82967=CARTESIAN_POINT('Ctrl Pts',(-13.5081446764819,2.68888644773051,5.46092625522282));
#82968=CARTESIAN_POINT('Ctrl Pts',(-13.4242572092542,2.64060328715728,5.45593349137977));
#82969=CARTESIAN_POINT('Ctrl Pts',(-13.342826504894,2.58847025424634,5.45094072753672));
#82970=CARTESIAN_POINT('Ctrl Pts',(-13.269001308176,2.54120636969085,5.44641428047015));
#82971=CARTESIAN_POINT('Ctrl Pts',(-13.1971953162039,2.49077887770757,5.44188783340359));
#82972=CARTESIAN_POINT('Ctrl Pts',(-13.1276888212995,2.43738653071547,5.43736138633702));
#82973=CARTESIAN_POINT('',(-15.7937992825329,-2.96922295374568,6.));
#82974=CARTESIAN_POINT('Ctrl Pts',(-15.7937992825329,-2.96922295374568,
6.));
#82975=CARTESIAN_POINT('Ctrl Pts',(-16.7765145099755,-2.70650147589437,
5.94732494375275));
#82976=CARTESIAN_POINT('Ctrl Pts',(-17.8761971489951,-1.66915693147179,
5.87785090484933));
#82977=CARTESIAN_POINT('Ctrl Pts',(-18.0726938053019,-0.328583276450114,
5.80837686594592));
#82978=CARTESIAN_POINT('Ctrl Pts',(-18.0703307438941,-0.00353868753125157,
5.79157788328974));
#82979=CARTESIAN_POINT('',(-14.2057854622994,-2.96911190730578,5.99999996471849));
#82980=CARTESIAN_POINT('Origin',(-15.,0.,6.));
#82981=CARTESIAN_POINT('',(-18.0736575411657,0.00192524165061634,5.70842344717746));
#82982=CARTESIAN_POINT('Ctrl Pts',(-14.2057854622994,-2.96911190730578,
5.99999996471849));
#82983=CARTESIAN_POINT('Ctrl Pts',(-14.2981329538255,-2.99381414911409,
5.99502017228295));
#82984=CARTESIAN_POINT('Ctrl Pts',(-14.3918009260944,-3.0142484885268,5.99004037984741));
#82985=CARTESIAN_POINT('Ctrl Pts',(-14.4863574076049,-3.03027614868309,
5.98506058741186));
#82986=CARTESIAN_POINT('Ctrl Pts',(-14.5807866776791,-3.04628224604818,
5.98008749453343));
#82987=CARTESIAN_POINT('Ctrl Pts',(-14.6761016489036,-3.05789337130818,
5.975114401655));
#82988=CARTESIAN_POINT('Ctrl Pts',(-14.7718563427238,-3.06502083543402,
5.97014130877657));
#82989=CARTESIAN_POINT('Ctrl Pts',(-14.8707044704539,-3.0723785581335,5.96500755605439));
#82990=CARTESIAN_POINT('Ctrl Pts',(-14.9700207596084,-3.07495783903088,
5.95987380333221));
#82991=CARTESIAN_POINT('Ctrl Pts',(-15.0693042032246,-3.07271853208448,
5.95474005061003));
#82992=CARTESIAN_POINT('Ctrl Pts',(-15.1653131834789,-3.0705530796327,5.94977561398513));
#82993=CARTESIAN_POINT('Ctrl Pts',(-15.2612909701088,-3.06388190765667,
5.94481117736023));
#82994=CARTESIAN_POINT('Ctrl Pts',(-15.3567818694496,-3.05272156405265,
5.93984674073533));
#82995=CARTESIAN_POINT('Ctrl Pts',(-15.4522414511916,-3.04156488064207,
5.93488393226804));
#82996=CARTESIAN_POINT('Ctrl Pts',(-15.5472140234408,-3.02592200199951,
5.92992112380074));
#82997=CARTESIAN_POINT('Ctrl Pts',(-15.6412484396551,-3.00586138879355,
5.92495831533345));
#82998=CARTESIAN_POINT('Ctrl Pts',(-15.7352782205293,-2.98580176445709,
5.91999575150324));
#82999=CARTESIAN_POINT('Ctrl Pts',(-15.8283695043764,-2.96132493159438,
5.91503318767304));
#83000=CARTESIAN_POINT('Ctrl Pts',(-15.9200818807813,-2.93255035466708,
5.91007062384283));
#83001=CARTESIAN_POINT('Ctrl Pts',(-16.0118152939033,-2.90376917751133,
5.90510692171422));
#83002=CARTESIAN_POINT('Ctrl Pts',(-16.1021687491958,-2.87068843159189,
5.90014321958561));
#83003=CARTESIAN_POINT('Ctrl Pts',(-16.1907186020685,-2.8334769207968,5.895179517457));
#83004=CARTESIAN_POINT('Ctrl Pts',(-16.279363489585,-2.79622547337207,5.89021048811835));
#83005=CARTESIAN_POINT('Ctrl Pts',(-16.3662005037129,-2.75483458692342,
5.88524145877971));
#83006=CARTESIAN_POINT('Ctrl Pts',(-16.4508278702327,-2.70952038947046,
5.88027242944107));
#83007=CARTESIAN_POINT('Ctrl Pts',(-16.5355097997349,-2.6641769759629,5.87530019635083));
#83008=CARTESIAN_POINT('Ctrl Pts',(-16.6179788668853,-2.61490544397536,
5.87032796326059));
#83009=CARTESIAN_POINT('Ctrl Pts',(-16.6978614993426,-2.56196576461322,
5.86535573017034));
#83010=CARTESIAN_POINT('Ctrl Pts',(-16.777862735832,-2.50894748419303,5.86037611466324));
#83011=CARTESIAN_POINT('Ctrl Pts',(-16.8552695203958,-2.45225045177839,
5.85539649915613));
#83012=CARTESIAN_POINT('Ctrl Pts',(-16.929740909553,-2.39217521766225,5.85041688364903));
#83013=CARTESIAN_POINT('Ctrl Pts',(-16.9471171151244,-2.37815802757672,
5.84925500358076));
#83014=CARTESIAN_POINT('Ctrl Pts',(-16.9643336718353,-2.36395708041279,
5.84809312351249));
#83015=CARTESIAN_POINT('Ctrl Pts',(-16.9813865454886,-2.34957647403879,
5.84693124344423));
#83016=CARTESIAN_POINT('Ctrl Pts',(-17.0538726013641,-2.28844933157971,
5.84199248032074));
#83017=CARTESIAN_POINT('Ctrl Pts',(-17.1236662966299,-2.22384719863751,
5.83705371719726));
#83018=CARTESIAN_POINT('Ctrl Pts',(-17.1904101659715,-2.15603932125758,
5.83211495407377));
#83019=CARTESIAN_POINT('Ctrl Pts',(-17.2600602784974,-2.08527887035407,
5.82696114128643));
#83020=CARTESIAN_POINT('Ctrl Pts',(-17.3263884968989,-2.01102738546575,
5.82180732849908));
#83021=CARTESIAN_POINT('Ctrl Pts',(-17.3890253810344,-1.93363905079863,
5.81665351571173));
#83022=CARTESIAN_POINT('Ctrl Pts',(-17.4489019566701,-1.85966109774477,
5.81172682330944));
#83023=CARTESIAN_POINT('Ctrl Pts',(-17.5054053086427,-1.78281729323004,
5.80680013090714));
#83024=CARTESIAN_POINT('Ctrl Pts',(-17.5582502566199,-1.70345468812772,
5.80187343850485));
#83025=CARTESIAN_POINT('Ctrl Pts',(-17.6110650497904,-1.62413736954947,
5.79694955741115));
#83026=CARTESIAN_POINT('Ctrl Pts',(-17.660225334983,-1.54230447853674,5.79202567631746));
#83027=CARTESIAN_POINT('Ctrl Pts',(-17.7054876831221,-1.45833420260055,
5.78710179522376));
#83028=CARTESIAN_POINT('Ctrl Pts',(-17.750737289915,-1.37438756428807,5.78217930020206));
#83029=CARTESIAN_POINT('Ctrl Pts',(-17.7920909261204,-1.28830513300759,
5.77725680518037));
#83030=CARTESIAN_POINT('Ctrl Pts',(-17.8293504193898,-1.20049092220581,
5.77233431015867));
#83031=CARTESIAN_POINT('Ctrl Pts',(-17.866610196384,-1.11267604271373,5.76741177765302));
#83032=CARTESIAN_POINT('Ctrl Pts',(-17.8997755947692,-1.02312977334097,
5.76248924514736));
#83033=CARTESIAN_POINT('Ctrl Pts',(-17.9286965110889,-0.932276244433962,
5.7575667126417));
#83034=CARTESIAN_POINT('Ctrl Pts',(-17.9576404750251,-0.841350312658586,
5.75264025727826));
#83035=CARTESIAN_POINT('Ctrl Pts',(-17.9823330691332,-0.749115472153399,
5.74771380191482));
#83036=CARTESIAN_POINT('Ctrl Pts',(-18.0026741953112,-0.656010614862657,
5.74278734655138));
#83037=CARTESIAN_POINT('Ctrl Pts',(-18.0230248956179,-0.562861935125983,
5.73785857241177));
#83038=CARTESIAN_POINT('Ctrl Pts',(-18.0390199757596,-0.468842867573405,
5.73292979827217));
#83039=CARTESIAN_POINT('Ctrl Pts',(-18.0506108997062,-0.374400038186194,
5.72800102413256));
#83040=CARTESIAN_POINT('Ctrl Pts',(-18.0622170327952,-0.279833284731336,
5.72306578265453));
#83041=CARTESIAN_POINT('Ctrl Pts',(-18.0694074453535,-0.184842108475051,
5.71813054117649));
#83042=CARTESIAN_POINT('Ctrl Pts',(-18.0721856531716,-0.08987526047971,
5.71319529969846));
#83043=CARTESIAN_POINT('Ctrl Pts',(-18.0730810634597,-0.0592676536020603,
5.71160468219146));
#83044=CARTESIAN_POINT('Ctrl Pts',(-18.0735185562359,-0.0286625483501631,
5.71001406468446));
#83045=CARTESIAN_POINT('Ctrl Pts',(-18.0734993970759,0.00192514259417154,
5.70842344717746));
#83046=CARTESIAN_POINT('Ctrl Pts',(-18.0766836350382,0.00192713709989245,
5.70842344717746));
#83047=CARTESIAN_POINT('Ctrl Pts',(-18.0776349419369,0.127164229732423,
5.70191765635247));
#83048=CARTESIAN_POINT('Ctrl Pts',(-18.0140094212094,1.26546671125655,5.64273680928023));
#83049=CARTESIAN_POINT('Ctrl Pts',(-16.5948036893957,3.25791148079165,5.53088090596076));
#83050=CARTESIAN_POINT('Ctrl Pts',(-14.156529652945,3.15709983619958,5.41926965443919));
#83051=CARTESIAN_POINT('Ctrl Pts',(-13.2206851146332,2.51416173457833,5.36033345916488));
#83052=CARTESIAN_POINT('Ctrl Pts',(-13.1256826865589,2.43995710119902,5.35407232013781));
#83053=CARTESIAN_POINT('Origin',(-15.,0.,3.));
#83054=CARTESIAN_POINT('',(-17.3614291533995,0.872615954171733,0.32975881722873));
#83055=CARTESIAN_POINT('',(-17.3614291890562,0.872615857679407,0.0533213468502638));
#83056=CARTESIAN_POINT('',(-17.3614291890287,0.872615857753799,3.));
#83057=CARTESIAN_POINT('',(-16.913465996665,1.63598720337497,0.));
#83058=CARTESIAN_POINT('Ctrl Pts',(-17.3614291890837,0.872615857605008,
0.0533213468502644));
#83059=CARTESIAN_POINT('Ctrl Pts',(-17.3052161900689,1.02473665110477,0.0434939346638048));
#83060=CARTESIAN_POINT('Ctrl Pts',(-17.2344350464082,1.17107267661228,0.0340532122102998));
#83061=CARTESIAN_POINT('Ctrl Pts',(-17.1011568765138,1.38988700371282,0.0189269413933175));
#83062=CARTESIAN_POINT('Ctrl Pts',(-17.0477914117863,1.46737654487933,0.0133363778978164));
#83063=CARTESIAN_POINT('Ctrl Pts',(-16.9764158275753,1.55951755727942,0.00618525948857481));
#83064=CARTESIAN_POINT('Ctrl Pts',(-16.9623709791679,1.57715396022876,0.00479206767144312));
#83065=CARTESIAN_POINT('Ctrl Pts',(-16.9366976029821,1.60851864428275,0.00226581726433723));
#83066=CARTESIAN_POINT('Ctrl Pts',(-16.9251550674062,1.62231555646376,0.00113715644275298));
#83067=CARTESIAN_POINT('Ctrl Pts',(-16.9134659966651,1.63598720337494,-1.35308431126191E-14));
#83068=CARTESIAN_POINT('',(-13.1119440673944,1.66524804319138,0.));
#83069=CARTESIAN_POINT('Origin',(-15.,0.,0.));
#83070=CARTESIAN_POINT('Ctrl Pts',(-13.1119440673944,1.66524804319138,2.16064552317416E-15));
#83071=CARTESIAN_POINT('Ctrl Pts',(-13.1135335123553,1.66705015369397,0.000157689880063195));
#83072=CARTESIAN_POINT('Ctrl Pts',(-13.1151255349311,1.66884998572192,0.000315530651660374));
#83073=CARTESIAN_POINT('Ctrl Pts',(-13.1324724607268,1.68840474846791,0.00203422419148989));
#83074=CARTESIAN_POINT('Ctrl Pts',(-13.1484745908993,1.7059376549406,0.00360924412967116));
#83075=CARTESIAN_POINT('Ctrl Pts',(-13.2534887681128,1.81777937908589,0.0138647376047754));
#83076=CARTESIAN_POINT('Ctrl Pts',(-13.3494226709774,1.90531206599647,0.0228556276482404));
#83077=CARTESIAN_POINT('Ctrl Pts',(-13.5355877911107,2.05051970210863,0.0391499519066325));
#83078=CARTESIAN_POINT('Ctrl Pts',(-13.623582970446,2.11059555403921,0.0464530866945166));
#83079=CARTESIAN_POINT('Ctrl Pts',(-13.7788341957787,2.202736759696,0.0585670985125662));
#83080=CARTESIAN_POINT('Ctrl Pts',(-13.8441880865476,2.23772110470361,0.0634565361499455));
#83081=CARTESIAN_POINT('Ctrl Pts',(-13.9474036428933,2.28724240695303,0.0708607840807191));
#83082=CARTESIAN_POINT('Ctrl Pts',(-13.9842281774554,2.30383263886003,0.0734430106906672));
#83083=CARTESIAN_POINT('Ctrl Pts',(-14.0552558746739,2.33379776538124,0.0783160517901265));
#83084=CARTESIAN_POINT('Ctrl Pts',(-14.0893833186159,2.34732421127126,0.0806113988119353));
#83085=CARTESIAN_POINT('Ctrl Pts',(-14.1714383348913,2.37778772791051,0.0860287056502805));
#83086=CARTESIAN_POINT('Ctrl Pts',(-14.2196076831033,2.39402950428948,0.0891277408921832));
#83087=CARTESIAN_POINT('Ctrl Pts',(-14.405553329791,2.45051727712314,0.100829173395792));
#83088=CARTESIAN_POINT('Ctrl Pts',(-14.5461873762118,2.48041537783897,0.109121425604108));
#83089=CARTESIAN_POINT('Ctrl Pts',(-14.7850155934075,2.51018443359966,0.123024089519485));
#83090=CARTESIAN_POINT('Ctrl Pts',(-14.882028683596,2.51660984285428,0.128629015144472));
#83091=CARTESIAN_POINT('Ctrl Pts',(-15.0364294410421,2.51788772643851,0.137783619794858));
#83092=CARTESIAN_POINT('Ctrl Pts',(-15.0936893712441,2.51640756498048,0.141230510496763));
#83093=CARTESIAN_POINT('Ctrl Pts',(-15.1761668073964,2.51145675548247,0.146332446298021));
#83094=CARTESIAN_POINT('Ctrl Pts',(-15.2014635092165,2.50955416643222,0.147915963725465));
#83095=CARTESIAN_POINT('Ctrl Pts',(-15.247739526031,2.50536954522139,0.150854040337095));
#83096=CARTESIAN_POINT('Ctrl Pts',(-15.2687261830582,2.50320545547813,0.152202679230776));
#83097=CARTESIAN_POINT('Ctrl Pts',(-15.321716423073,2.49706722557264,0.155647203925214));
#83098=CARTESIAN_POINT('Ctrl Pts',(-15.3536742692965,2.49274155642832,0.157760245281535));
#83099=CARTESIAN_POINT('Ctrl Pts',(-15.5316576101007,2.46515922978768,0.169696690307591));
#83100=CARTESIAN_POINT('Ctrl Pts',(-15.6754877712572,2.42968734194731,0.179959744111941));
#83101=CARTESIAN_POINT('Ctrl Pts',(-15.9109727885108,2.34907369416207,0.197107441612617));
#83102=CARTESIAN_POINT('Ctrl Pts',(-16.0045310908566,2.31061438230456,0.204022654996152));
#83103=CARTESIAN_POINT('Ctrl Pts',(-16.1599282872409,2.23550632759541,0.215582544968285));
#83104=CARTESIAN_POINT('Ctrl Pts',(-16.2229752173846,2.20164833410109,0.220296203449823));
#83105=CARTESIAN_POINT('Ctrl Pts',(-16.3186507052275,2.14488772362933,0.227485132641972));
#83106=CARTESIAN_POINT('Ctrl Pts',(-16.3523190521331,2.12382120287335,0.23002251074712));
#83107=CARTESIAN_POINT('Ctrl Pts',(-16.4158738302987,2.08193010866575,0.234831074233356));
#83108=CARTESIAN_POINT('Ctrl Pts',(-16.4458340838878,2.06123644956739,0.237106273146607));
#83109=CARTESIAN_POINT('Ctrl Pts',(-16.5164631128415,2.01015473018781,0.242497126511684));
#83110=CARTESIAN_POINT('Ctrl Pts',(-16.5566829838664,1.97917180465407,0.24558925166422));
#83111=CARTESIAN_POINT('Ctrl Pts',(-16.7442991373719,1.82538369300179,0.260176814510257));
#83112=CARTESIAN_POINT('Ctrl Pts',(-16.8782700861455,1.68721986885628,0.271036910978185));
#83113=CARTESIAN_POINT('Ctrl Pts',(-17.0392174994968,1.4780377503028,0.286288042746235));
#83114=CARTESIAN_POINT('Ctrl Pts',(-17.0807027192118,1.41904144931832,0.290485770188388));
#83115=CARTESIAN_POINT('Ctrl Pts',(-17.1455044627881,1.31792350532712,0.297648848234922));
#83116=CARTESIAN_POINT('Ctrl Pts',(-17.1702483661582,1.27676668014217,0.300556367568883));
#83117=CARTESIAN_POINT('Ctrl Pts',(-17.2053952931272,1.21432974395098,0.304993664207599));
#83118=CARTESIAN_POINT('Ctrl Pts',(-17.2167006205197,1.19356750296359,0.306473444302919));
#83119=CARTESIAN_POINT('Ctrl Pts',(-17.2373822371722,1.15427814178871,0.309287409043184));
#83120=CARTESIAN_POINT('Ctrl Pts',(-17.2468245989627,1.13578888961816,0.310617695718588));
#83121=CARTESIAN_POINT('Ctrl Pts',(-17.270915964066,1.08713897474704,0.314130599103508));
#83122=CARTESIAN_POINT('Ctrl Pts',(-17.285192619967,1.05679936520077,0.316333500626808));
#83123=CARTESIAN_POINT('Ctrl Pts',(-17.3214038409402,0.975679075861538,
0.32223831725814));
#83124=CARTESIAN_POINT('Ctrl Pts',(-17.3422709041098,0.924461039268354,
0.325981378466721));
#83125=CARTESIAN_POINT('Ctrl Pts',(-17.3614291533995,0.872615954171733,
0.32975881722873));
#83126=CARTESIAN_POINT('Origin',(-15.,0.,3.));
#83127=CARTESIAN_POINT('',(-17.361429188522,0.872615859124936,1.33336838650867));
#83128=CARTESIAN_POINT('',(-17.3614291890287,0.872615857753796,1.05617159787625));
#83129=CARTESIAN_POINT('',(-17.3614291890287,0.872615857753799,3.));
#83130=CARTESIAN_POINT('',(-17.5174978061968,-0.00332352138350004,0.1125849952481));
#83131=CARTESIAN_POINT('Ctrl Pts',(-17.3614291890287,0.872615857753796,
1.05617159787625));
#83132=CARTESIAN_POINT('Ctrl Pts',(-17.3326448870889,0.950510489374704,
1.05093100125945));
#83133=CARTESIAN_POINT('Ctrl Pts',(-17.2999832020769,1.02703116401984,1.04569040464266));
#83134=CARTESIAN_POINT('Ctrl Pts',(-17.2636046805941,1.10177134651095,1.04044980802587));
#83135=CARTESIAN_POINT('Ctrl Pts',(-17.2272362206276,1.17649085747555,1.03521066084535));
#83136=CARTESIAN_POINT('Ctrl Pts',(-17.1871531677912,1.2494304402801,1.02997151366483));
#83137=CARTESIAN_POINT('Ctrl Pts',(-17.1435634096145,1.32020534727064,1.02473236648432));
#83138=CARTESIAN_POINT('Ctrl Pts',(-17.0999725941995,1.39098197085576,1.01949309223205));
#83139=CARTESIAN_POINT('Ctrl Pts',(-17.0528751474684,1.45959342265606,1.01425381797978));
#83140=CARTESIAN_POINT('Ctrl Pts',(-17.0025232141706,1.52568247899355,1.00901454372751));
#83141=CARTESIAN_POINT('Ctrl Pts',(-16.952120986379,1.59183754899549,1.00377003617776));
#83142=CARTESIAN_POINT('Ctrl Pts',(-16.8984580591094,1.65546482379302,0.998525528628003));
#83143=CARTESIAN_POINT('Ctrl Pts',(-16.841827645515,1.71623925319773,0.993281021078248));
#83144=CARTESIAN_POINT('Ctrl Pts',(-16.7851691135384,1.77704385858963,0.988033909502522));
#83145=CARTESIAN_POINT('Ctrl Pts',(-16.7255404910154,1.83499247532486,0.982786797926795));
#83146=CARTESIAN_POINT('Ctrl Pts',(-16.6632709798934,1.88979784565554,0.977539686351068));
#83147=CARTESIAN_POINT('Ctrl Pts',(-16.6008925738527,1.94469905785563,0.972283398795334));
#83148=CARTESIAN_POINT('Ctrl Pts',(-16.5358644134693,1.99644575379372,0.9670271112396));
#83149=CARTESIAN_POINT('Ctrl Pts',(-16.4685476759482,2.04479191446642,0.961770823683865));
#83150=CARTESIAN_POINT('Ctrl Pts',(-16.4104051657852,2.08654924320464,0.957230886606063));
#83151=CARTESIAN_POINT('Ctrl Pts',(-16.350556005376,2.12577036497012,0.95269094952826));
#83152=CARTESIAN_POINT('Ctrl Pts',(-16.2892476054404,2.16232441180002,0.948151012450456));
#83153=CARTESIAN_POINT('Ctrl Pts',(-16.2182438678792,2.2046591318487,0.942893127704567));
#83154=CARTESIAN_POINT('Ctrl Pts',(-16.1450230554184,2.24357016117157,0.937635242958676));
#83155=CARTESIAN_POINT('Ctrl Pts',(-16.0699488301934,2.27881893768853,0.932377358212785));
#83156=CARTESIAN_POINT('Ctrl Pts',(-15.9949803266762,2.31401807585302,0.927126877773143));
#83157=CARTESIAN_POINT('Ctrl Pts',(-15.918164008624,2.34556501121923,0.921876397333499));
#83158=CARTESIAN_POINT('Ctrl Pts',(-15.8398902335713,2.37326581856131,0.916625916893855));
#83159=CARTESIAN_POINT('Ctrl Pts',(-15.7613129936211,2.4010740210387,0.911355080511142));
#83160=CARTESIAN_POINT('Ctrl Pts',(-15.6812673759639,2.42500596976104,0.906084244128428));
#83161=CARTESIAN_POINT('Ctrl Pts',(-15.6001709003809,2.4449133195956,0.900813407745713));
#83162=CARTESIAN_POINT('Ctrl Pts',(-15.5195303896874,2.46470874036663,0.895572206637671));
#83163=CARTESIAN_POINT('Ctrl Pts',(-15.4378512585436,2.48052458758556,0.890331005529628));
#83164=CARTESIAN_POINT('Ctrl Pts',(-15.3555598645567,2.49226471963081,0.885089804421585));
#83165=CARTESIAN_POINT('Ctrl Pts',(-15.2732951560398,2.50400104458363,0.87985030293131));
#83166=CARTESIAN_POINT('Ctrl Pts',(-15.1904190349098,2.51166421436965,0.874610801441035));
#83167=CARTESIAN_POINT('Ctrl Pts',(-15.1073665468774,2.51520946933086,0.86937129995076));
#83168=CARTESIAN_POINT('Ctrl Pts',(-15.024316013629,2.51875464084836,0.864131921781214));
#83169=CARTESIAN_POINT('Ctrl Pts',(-14.9410895822175,2.5181820716874,0.858892543611667));
#83170=CARTESIAN_POINT('Ctrl Pts',(-14.858124511103,2.51349907412958,0.85365316544212));
#83171=CARTESIAN_POINT('Ctrl Pts',(-14.7742954033543,2.50876730566861,0.848359221964331));
#83172=CARTESIAN_POINT('Ctrl Pts',(-14.6907336115004,2.49983900301017,0.843065278486542));
#83173=CARTESIAN_POINT('Ctrl Pts',(-14.6078853482802,2.4867754924614,0.837771335008753));
#83174=CARTESIAN_POINT('Ctrl Pts',(-14.5257736899565,2.47382812974075,0.832524460045574));
#83175=CARTESIAN_POINT('Ctrl Pts',(-14.4443633662088,2.4568189551323,0.827277585082395));
#83176=CARTESIAN_POINT('Ctrl Pts',(-14.3640771794608,2.4358588662559,0.822030710119216));
#83177=CARTESIAN_POINT('Ctrl Pts',(-14.2827106491997,2.41461673513823,0.816713232384122));
#83178=CARTESIAN_POINT('Ctrl Pts',(-14.2024992013692,2.38931671685081,0.811395754649029));
#83179=CARTESIAN_POINT('Ctrl Pts',(-14.1238638879225,2.36012537021103,0.806078276913937));
#83180=CARTESIAN_POINT('Ctrl Pts',(-14.0452285744758,2.33093402357125,0.800760799178844));
#83181=CARTESIAN_POINT('Ctrl Pts',(-13.9681698167597,2.29785159865797,0.795443321443751));
#83182=CARTESIAN_POINT('Ctrl Pts',(-13.893082930489,2.26109284445046,0.79012584370866));
#83183=CARTESIAN_POINT('Ctrl Pts',(-13.8189474965226,2.22479987332616,0.784875745601297));
#83184=CARTESIAN_POINT('Ctrl Pts',(-13.7464608376546,2.18478938452908,0.779625647493936));
#83185=CARTESIAN_POINT('Ctrl Pts',(-13.6760207366242,2.14123449443323,0.774375549386575));
#83186=CARTESIAN_POINT('Ctrl Pts',(-13.605680399304,2.09774129075429,0.769132886948089));
#83187=CARTESIAN_POINT('Ctrl Pts',(-13.5373812527803,2.05071389740047,0.763890224509603));
#83188=CARTESIAN_POINT('Ctrl Pts',(-13.4714983702567,2.00037221983111,0.758647562071117));
#83189=CARTESIAN_POINT('Ctrl Pts',(-13.405236922355,1.94974127719816,0.753374775108442));
#83190=CARTESIAN_POINT('Ctrl Pts',(-13.3414200243656,1.89575804321547,0.748101988145768));
#83191=CARTESIAN_POINT('Ctrl Pts',(-13.2804014184089,1.83869164576061,0.742829201183094));
#83192=CARTESIAN_POINT('Ctrl Pts',(-13.219839031771,1.78205191804966,0.73759583739699));
#83193=CARTESIAN_POINT('Ctrl Pts',(-13.1620335767745,1.72237529581021,0.732362473610887));
#83194=CARTESIAN_POINT('Ctrl Pts',(-13.1072979450464,1.65996541565613,0.727129109824783));
#83195=CARTESIAN_POINT('Ctrl Pts',(-13.0525799854307,1.59757568534566,0.721897435698419));
#83196=CARTESIAN_POINT('Ctrl Pts',(-13.0009301854049,1.53245479702817,0.716665761572055));
#83197=CARTESIAN_POINT('Ctrl Pts',(-12.9526231667737,1.4649417574663,0.711434087445692));
#83198=CARTESIAN_POINT('Ctrl Pts',(-12.9043170984839,1.39743004608469,0.706202516241761));
#83199=CARTESIAN_POINT('Ctrl Pts',(-12.8593539490163,1.32752665371892,0.700970945037832));
#83200=CARTESIAN_POINT('Ctrl Pts',(-12.8179659397959,1.25560089602911,0.695739373833902));
#83201=CARTESIAN_POINT('Ctrl Pts',(-12.7760110637684,1.18269001425678,0.690436148928323));
#83202=CARTESIAN_POINT('Ctrl Pts',(-12.7377302625247,1.107701362593,0.685132924022745));
#83203=CARTESIAN_POINT('Ctrl Pts',(-12.7033171764188,1.03104522590768,0.679829699117166));
#83204=CARTESIAN_POINT('Ctrl Pts',(-12.6693195724963,0.955314587707073,
0.67459050204845));
#83205=CARTESIAN_POINT('Ctrl Pts',(-12.6390969079577,0.877956970031112,
0.669351304979735));
#83206=CARTESIAN_POINT('Ctrl Pts',(-12.6127865685549,0.799386191229341,
0.664112107911019));
#83207=CARTESIAN_POINT('Ctrl Pts',(-12.585993924107,0.719375100980596,0.658776869087008));
#83208=CARTESIAN_POINT('Ctrl Pts',(-12.5632586093974,0.638106412233824,
0.653441630262997));
#83209=CARTESIAN_POINT('Ctrl Pts',(-12.5446715529995,0.556029196490907,
0.648106391438986));
#83210=CARTESIAN_POINT('Ctrl Pts',(-12.5260844966017,0.473951980747991,
0.642771152614975));
#83211=CARTESIAN_POINT('Ctrl Pts',(-12.5116457181982,0.391066741099775,
0.637435913790963));
#83212=CARTESIAN_POINT('Ctrl Pts',(-12.5013906609342,0.307827257943743,
0.632100674966951));
#83213=CARTESIAN_POINT('Ctrl Pts',(-12.4912682527072,0.225664476457947,
0.626834447390188));
#83214=CARTESIAN_POINT('Ctrl Pts',(-12.485184536481,0.142853551862634,0.621568219813424));
#83215=CARTESIAN_POINT('Ctrl Pts',(-12.4832109210679,0.0598245950088185,
0.61630199223666));
#83216=CARTESIAN_POINT('Ctrl Pts',(-12.4812400963258,-0.0230869597886339,
0.611043211049327));
#83217=CARTESIAN_POINT('Ctrl Pts',(-12.4833678382513,-0.106215478942918,
0.605784429861994));
#83218=CARTESIAN_POINT('Ctrl Pts',(-12.4896139375275,-0.189124475793081,
0.60052564867466));
#83219=CARTESIAN_POINT('Ctrl Pts',(-12.4958718842765,-0.272190732724241,
0.595256892739267));
#83220=CARTESIAN_POINT('Ctrl Pts',(-12.5062638709878,-0.355036171088218,
0.589988136803874));
#83221=CARTESIAN_POINT('Ctrl Pts',(-12.5207572668831,-0.437220448157504,
0.584719380868481));
#83222=CARTESIAN_POINT('Ctrl Pts',(-12.5351972505915,-0.519101853352908,
0.579470041761221));
#83223=CARTESIAN_POINT('Ctrl Pts',(-12.5537083992556,-0.600326505241181,
0.574220702653961));
#83224=CARTESIAN_POINT('Ctrl Pts',(-12.5762066114153,-0.680464443929934,
0.568971363546702));
#83225=CARTESIAN_POINT('Ctrl Pts',(-12.5986971988316,-0.760575223518061,
0.563723803463601));
#83226=CARTESIAN_POINT('Ctrl Pts',(-12.6251720416696,-0.839599579622999,
0.558476243380501));
#83227=CARTESIAN_POINT('Ctrl Pts',(-12.6554965123832,-0.917120301025145,
0.5532286832974));
#83228=CARTESIAN_POINT('Ctrl Pts',(-12.6858197490691,-0.994637867789994,
0.547981336759123));
#83229=CARTESIAN_POINT('Ctrl Pts',(-12.7199921338847,-1.07065149415662,
0.542733990220846));
#83230=CARTESIAN_POINT('Ctrl Pts',(-12.7578304822127,-1.14476290274696,
0.537486643682569));
#83231=CARTESIAN_POINT('Ctrl Pts',(-12.7959350221214,-1.21939568274665,
0.532202382227788));
#83232=CARTESIAN_POINT('Ctrl Pts',(-12.8377571101419,-1.29209894713812,
0.526918120773007));
#83233=CARTESIAN_POINT('Ctrl Pts',(-12.8830629103333,-1.36249169112816,
0.521633859318227));
#83234=CARTESIAN_POINT('Ctrl Pts',(-12.9281139033789,-1.4324885349443,0.516379317404273));
#83235=CARTESIAN_POINT('Ctrl Pts',(-12.9766092089694,-1.50020043601646,
0.51112477549032));
#83236=CARTESIAN_POINT('Ctrl Pts',(-13.028276749544,-1.5652838955318,0.505870233576366));
#83237=CARTESIAN_POINT('Ctrl Pts',(-13.0803826353464,-1.63091952036352,
0.500571112351172));
#83238=CARTESIAN_POINT('Ctrl Pts',(-13.1357145248397,-1.69388153391925,
0.495271991125978));
#83239=CARTESIAN_POINT('Ctrl Pts',(-13.1939548016703,-1.75385489467925,
0.489972869900785));
#83240=CARTESIAN_POINT('Ctrl Pts',(-13.2521950785009,-1.81382825543925,
0.484673748675591));
#83241=CARTESIAN_POINT('Ctrl Pts',(-13.3133433562412,-1.87081268452723,
0.479374627450397));
#83242=CARTESIAN_POINT('Ctrl Pts',(-13.3770487753447,-1.92453515748345,
0.474075506225204));
#83243=CARTESIAN_POINT('Ctrl Pts',(-13.4403122453009,-1.97788493685339,
0.468813147054786));
#83244=CARTESIAN_POINT('Ctrl Pts',(-13.5063221429355,-2.02820737021692,
0.463550787884368));
#83245=CARTESIAN_POINT('Ctrl Pts',(-13.5747571460486,-2.07520819612405,
0.458288428713951));
#83246=CARTESIAN_POINT('Ctrl Pts',(-13.6430971283048,-2.12214376217075,
0.453033376241201));
#83247=CARTESIAN_POINT('Ctrl Pts',(-13.7138551510125,-2.16576662421337,
0.447778323768452));
#83248=CARTESIAN_POINT('Ctrl Pts',(-13.7866764018457,-2.2058223174503,0.442523271295703));
#83249=CARTESIAN_POINT('Ctrl Pts',(-13.8597007062691,-2.24598970133012,
0.437253565720193));
#83250=CARTESIAN_POINT('Ctrl Pts',(-13.934799399838,-2.28256969880127,0.431983860144683));
#83251=CARTESIAN_POINT('Ctrl Pts',(-14.0115848495443,-2.31534916164921,
0.426714154569173));
#83252=CARTESIAN_POINT('Ctrl Pts',(-14.0880244836537,-2.34798099692506,
0.421468181958519));
#83253=CARTESIAN_POINT('Ctrl Pts',(-14.166135289611,-2.37684627000409,0.416222209347864));
#83254=CARTESIAN_POINT('Ctrl Pts',(-14.2455112625665,-2.40178121299297,
0.41097623673721));
#83255=CARTESIAN_POINT('Ctrl Pts',(-14.3248624773042,-2.42670837850555,
0.405731900401708));
#83256=CARTESIAN_POINT('Ctrl Pts',(-14.4054776368251,-2.44770751123073,
0.400487564066206));
#83257=CARTESIAN_POINT('Ctrl Pts',(-14.486933900383,-2.46466416118379,0.395243227730705));
#83258=CARTESIAN_POINT('Ctrl Pts',(-14.5683891181309,-2.48162059343187,
0.389998958726788));
#83259=CARTESIAN_POINT('Ctrl Pts',(-14.6506849680177,-2.4945345535338,0.384754689722871));
#83260=CARTESIAN_POINT('Ctrl Pts',(-14.7333880403175,-2.50334262795852,
0.379510420718955));
#83261=CARTESIAN_POINT('Ctrl Pts',(-14.816786124462,-2.51222472280211,0.374222080449331));
#83262=CARTESIAN_POINT('Ctrl Pts',(-14.9005978372215,-2.51693152990207,
0.368933740179708));
#83263=CARTESIAN_POINT('Ctrl Pts',(-14.9843748973317,-2.51745151019173,
0.363645399910085));
#83264=CARTESIAN_POINT('Ctrl Pts',(-15.0675738836329,-2.51796790254232,
0.358393549951753));
#83265=CARTESIAN_POINT('Ctrl Pts',(-15.1507382326642,-2.51435514771791,
0.353141699993422));
#83266=CARTESIAN_POINT('Ctrl Pts',(-15.2334320679974,-2.50665428801629,
0.34788985003509));
#83267=CARTESIAN_POINT('Ctrl Pts',(-15.3169877492946,-2.49887316894799,
0.342583264609821));
#83268=CARTESIAN_POINT('Ctrl Pts',(-15.4000625758693,-2.48691830414295,
0.337276679184551));
#83269=CARTESIAN_POINT('Ctrl Pts',(-15.4822173048577,-2.47088500762294,
0.331970093759281));
#83270=CARTESIAN_POINT('Ctrl Pts',(-15.564372033846,-2.45485171110292,0.326663508334012));
#83271=CARTESIAN_POINT('Ctrl Pts',(-15.6456062166517,-2.43474015815058,
0.321356922908741));
#83272=CARTESIAN_POINT('Ctrl Pts',(-15.7254979597234,-2.41069677903239,
0.316050337483472));
#83273=CARTESIAN_POINT('Ctrl Pts',(-15.8038427307388,-2.38711896036145,
0.310846505347241));
#83274=CARTESIAN_POINT('Ctrl Pts',(-15.8811971867098,-2.35966961191086,
0.305642673211009));
#83275=CARTESIAN_POINT('Ctrl Pts',(-15.9571460064262,-2.32844964995647,
0.300438841074778));
#83276=CARTESIAN_POINT('Ctrl Pts',(-16.0329861558088,-2.29727435865922,
0.295242454770849));
#83277=CARTESIAN_POINT('Ctrl Pts',(-16.1074242298212,-2.26233934147627,
0.29004606846692));
#83278=CARTESIAN_POINT('Ctrl Pts',(-16.1800592325574,-2.22379550715799,
0.28484968216299));
#83279=CARTESIAN_POINT('Ctrl Pts',(-16.2539238564564,-2.18459917318267,
0.279565327437105));
#83280=CARTESIAN_POINT('Ctrl Pts',(-16.325923316285,-2.14167083002662,0.27428097271122));
#83281=CARTESIAN_POINT('Ctrl Pts',(-16.3956564509007,-2.09522059007142,
0.268996617985334));
#83282=CARTESIAN_POINT('Ctrl Pts',(-16.4641097169547,-2.04962288890042,
0.263809251291323));
#83283=CARTESIAN_POINT('Ctrl Pts',(-16.5303787408325,-2.00063175712121,
0.258621884597311));
#83284=CARTESIAN_POINT('Ctrl Pts',(-16.5941099988484,-1.94849161188122,
0.253434517903299));
#83285=CARTESIAN_POINT('Ctrl Pts',(-16.6578228501835,-1.89636652560982,
0.248248649409796));
#83286=CARTESIAN_POINT('Ctrl Pts',(-16.7189990257932,-1.84109452913811,
0.243062780916293));
#83287=CARTESIAN_POINT('Ctrl Pts',(-16.7773169667484,-1.7829612025247,0.237876912422789));
#83288=CARTESIAN_POINT('Ctrl Pts',(-16.835636496752,-1.72482629189317,0.23269090262463));
#83289=CARTESIAN_POINT('Ctrl Pts',(-16.8910973045054,-1.66383022991061,
0.22750489282647));
#83290=CARTESIAN_POINT('Ctrl Pts',(-16.9434147849419,-1.60029535513585,
0.222318883028311));
#83291=CARTESIAN_POINT('Ctrl Pts',(-16.9974654145893,-1.53465572651663,
0.21696107350443));
#83292=CARTESIAN_POINT('Ctrl Pts',(-17.0481604449311,-1.46630652813774,
0.211603263980548));
#83293=CARTESIAN_POINT('Ctrl Pts',(-17.0952326766386,-1.39563830584638,
0.206245454456667));
#83294=CARTESIAN_POINT('Ctrl Pts',(-17.1408716867421,-1.32712173898402,
0.201050775680607));
#83295=CARTESIAN_POINT('Ctrl Pts',(-17.1831051609906,-1.25642578881495,
0.195856096904547));
#83296=CARTESIAN_POINT('Ctrl Pts',(-17.2217359743982,-1.18393222359437,
0.190661418128487));
#83297=CARTESIAN_POINT('Ctrl Pts',(-17.2621864980569,-1.10802383812701,
0.185222043230696));
#83298=CARTESIAN_POINT('Ctrl Pts',(-17.2986863508818,-1.03014485341659,
0.179782668332903));
#83299=CARTESIAN_POINT('Ctrl Pts',(-17.3310662766949,-0.950755627727631,
0.174343293435112));
#83300=CARTESIAN_POINT('Ctrl Pts',(-17.363446202508,-0.871366402038671,
0.16890391853732));
#83301=CARTESIAN_POINT('Ctrl Pts',(-17.3917060957219,-0.790467515069941,
0.163464543639529));
#83302=CARTESIAN_POINT('Ctrl Pts',(-17.415737281965,-0.708533439242165,
0.158025168741737));
#83303=CARTESIAN_POINT('Ctrl Pts',(-17.4466522592493,-0.603129150523376,
0.151027671834813));
#83304=CARTESIAN_POINT('Ctrl Pts',(-17.4706689005917,-0.495685522224355,
0.144030174927888));
#83305=CARTESIAN_POINT('Ctrl Pts',(-17.4875795798172,-0.386980728301084,
0.137032678020964));
#83306=CARTESIAN_POINT('Ctrl Pts',(-17.5040746181104,-0.280947746745211,
0.130207169837831));
#83307=CARTESIAN_POINT('Ctrl Pts',(-17.5138087928967,-0.173714442495203,
0.123381661654697));
#83308=CARTESIAN_POINT('Ctrl Pts',(-17.5166340645248,-0.0660245050990958,
0.116556153471564));
#83309=CARTESIAN_POINT('Ctrl Pts',(-17.5171819895709,-0.0451394286573785,
0.115232434063742));
#83310=CARTESIAN_POINT('Ctrl Pts',(-17.5174701965452,-0.0242372539493491,
0.113908714655921));
#83311=CARTESIAN_POINT('Ctrl Pts',(-17.5174978061968,-0.00332352138350004,
0.1125849952481));
#83312=CARTESIAN_POINT('Ctrl Pts',(-17.5174977222504,-0.00338651208338963,
0.111633905503722));
#83313=CARTESIAN_POINT('Ctrl Pts',(-17.5176325157458,0.0968175649154425,
0.104703074197213));
#83314=CARTESIAN_POINT('Ctrl Pts',(-17.5117846136227,0.196948044376628,
0.0978488253944215));
#83315=CARTESIAN_POINT('Ctrl Pts',(-17.4930720434123,0.354740893766269,
0.0872175436775509));
#83316=CARTESIAN_POINT('Ctrl Pts',(-17.4841264447284,0.412754141523008,
0.0833447591150981));
#83317=CARTESIAN_POINT('Ctrl Pts',(-17.4647998011908,0.514364129027663,
0.0766202001912281));
#83318=CARTESIAN_POINT('Ctrl Pts',(-17.4552678085838,0.558093984067512,
0.0737454561072239));
#83319=CARTESIAN_POINT('Ctrl Pts',(-17.4351215394682,0.63996442595149,0.0683922448439606));
#83320=CARTESIAN_POINT('Ctrl Pts',(-17.4247638172419,0.678153421756895,
0.0659072083612793));
#83321=CARTESIAN_POINT('Ctrl Pts',(-17.3981285586884,0.767925649809322,
0.0600836889126596));
#83322=CARTESIAN_POINT('Ctrl Pts',(-17.3810802704562,0.819260452293542,
0.0567682006828312));
#83323=CARTESIAN_POINT('Ctrl Pts',(-17.3620708144642,0.870878048526862,
0.053433613536233));
#83324=CARTESIAN_POINT('Ctrl Pts',(-17.3617502393738,0.87174704744106,0.0533774743223632));
#83325=CARTESIAN_POINT('Ctrl Pts',(-17.3614291890837,0.87261585760501,0.0533213468502636));
#83326=CARTESIAN_POINT('Ctrl Pts',(-17.3614291533995,0.872615954171733,
0.32975881722873));
#83327=CARTESIAN_POINT('Ctrl Pts',(-17.3835552367282,0.81273946672832,0.334121424873797));
#83328=CARTESIAN_POINT('Ctrl Pts',(-17.4034020623706,0.752026587676025,
0.338529625453672));
#83329=CARTESIAN_POINT('Ctrl Pts',(-17.4531844221817,0.577514795597414,
0.351064346283168));
#83330=CARTESIAN_POINT('Ctrl Pts',(-17.4774840866728,0.462291736318107,
0.359172488206155));
#83331=CARTESIAN_POINT('Ctrl Pts',(-17.5043312932454,0.268682296977471,
0.372328516818489));
#83332=CARTESIAN_POINT('Ctrl Pts',(-17.5114419898486,0.191119310229726,
0.377479436103626));
#83333=CARTESIAN_POINT('Ctrl Pts',(-17.516765524736,0.0729979165311001,
0.385137648848412));
#83334=CARTESIAN_POINT('Ctrl Pts',(-17.5176127964505,0.0326116499114517,
0.387723534903136));
#83335=CARTESIAN_POINT('Ctrl Pts',(-17.5173777526979,-0.0434495297615438,
0.392536475026815));
#83336=CARTESIAN_POINT('Ctrl Pts',(-17.5165094300388,-0.0791145299421246,
0.394769609835801));
#83337=CARTESIAN_POINT('Ctrl Pts',(-17.512756247774,-0.161369606599533,
0.399871355794675));
#83338=CARTESIAN_POINT('Ctrl Pts',(-17.5093331267655,-0.207922573269812,
0.402722574830289));
#83339=CARTESIAN_POINT('Ctrl Pts',(-17.4851893986466,-0.44566352085408,
0.417141889270126));
#83340=CARTESIAN_POINT('Ctrl Pts',(-17.4439084327773,-0.634113327432651,
0.428041337479941));
#83341=CARTESIAN_POINT('Ctrl Pts',(-17.3567675779103,-0.888430637067505,
0.44353417009997));
#83342=CARTESIAN_POINT('Ctrl Pts',(-17.328675493853,-0.959651781800779,
0.447973517484615));
#83343=CARTESIAN_POINT('Ctrl Pts',(-17.2770363992305,-1.07488963855831,
0.455485754108116));
#83344=CARTESIAN_POINT('Ctrl Pts',(-17.2553467882276,-1.11968417693967,
0.458492215238968));
#83345=CARTESIAN_POINT('Ctrl Pts',(-17.22134321923,-1.1849080213295,0.463041553373214));
#83346=CARTESIAN_POINT('Ctrl Pts',(-17.2100423362815,-1.20585467002197,
0.464529576566361));
#83347=CARTESIAN_POINT('Ctrl Pts',(-17.1883793902625,-1.24468020096113,
0.467344452902078));
#83348=CARTESIAN_POINT('Ctrl Pts',(-17.178091180958,-1.26259726143376,0.468666972891903));
#83349=CARTESIAN_POINT('Ctrl Pts',(-17.1509413459817,-1.30855966361013,
0.472117585430802));
#83350=CARTESIAN_POINT('Ctrl Pts',(-17.1337516128707,-1.33640595664184,
0.474264573196645));
#83351=CARTESIAN_POINT('Ctrl Pts',(-17.039450929768,-1.48270809215482,0.485816722063119));
#83352=CARTESIAN_POINT('Ctrl Pts',(-16.9530134946302,-1.59484054879456,
0.495621793098598));
#83353=CARTESIAN_POINT('Ctrl Pts',(-16.7867718132438,-1.7765910223426,0.512615649130391));
#83354=CARTESIAN_POINT('Ctrl Pts',(-16.7111297343397,-1.84955869676579,
0.519816267343447));
#83355=CARTESIAN_POINT('Ctrl Pts',(-16.5753940732101,-1.96501836852654,
0.531769505265099));
#83356=CARTESIAN_POINT('Ctrl Pts',(-16.5175957902642,-2.00999214156221,
0.536598870876882));
#83357=CARTESIAN_POINT('Ctrl Pts',(-16.4253816490581,-2.0754965339777,0.543913253657244));
#83358=CARTESIAN_POINT('Ctrl Pts',(-16.3923023927518,-2.09783055844111,
0.546464668245145));
#83359=CARTESIAN_POINT('Ctrl Pts',(-16.3282267632005,-2.13890873584394,
0.55127513820568));
#83360=CARTESIAN_POINT('Ctrl Pts',(-16.2973299084303,-2.15778873827146,
0.553538786079863));
#83361=CARTESIAN_POINT('Ctrl Pts',(-16.2229613386796,-2.20105775470535,
0.558862953888334));
#83362=CARTESIAN_POINT('Ctrl Pts',(-16.1791508181441,-2.22483561864094,
0.561901341018575));
#83363=CARTESIAN_POINT('Ctrl Pts',(-16.031732719489,-2.29926701070143,0.571841499385341));
#83364=CARTESIAN_POINT('Ctrl Pts',(-15.9253512859313,-2.34410529944111,
0.578556408502827));
#83365=CARTESIAN_POINT('Ctrl Pts',(-15.7198547933984,-2.41453963987603,
0.591090054750961));
#83366=CARTESIAN_POINT('Ctrl Pts',(-15.621532021519,-2.44169809770156,0.596912617368568));
#83367=CARTESIAN_POINT('Ctrl Pts',(-15.4662160344018,-2.4746073215871,0.606164010612973));
#83368=CARTESIAN_POINT('Ctrl Pts',(-15.4102151392395,-2.48450430093974,
0.609511242558185));
#83369=CARTESIAN_POINT('Ctrl Pts',(-15.31329076579,-2.49826740769255,0.615394868078066));
#83370=CARTESIAN_POINT('Ctrl Pts',(-15.2725184440567,-2.50304303151205,
0.617897181194153));
#83371=CARTESIAN_POINT('Ctrl Pts',(-15.2093224815791,-2.50888284619231,
0.621842671508584));
#83372=CARTESIAN_POINT('Ctrl Pts',(-15.1869691012376,-2.51064762646456,
0.623251156667712));
#83373=CARTESIAN_POINT('Ctrl Pts',(-15.1426703040893,-2.51355012673629,
0.626073189435645));
#83374=CARTESIAN_POINT('Ctrl Pts',(-15.1207277961168,-2.51469953492058,
0.627486072094262));
#83375=CARTESIAN_POINT('Ctrl Pts',(-15.0599929579003,-2.51708430562984,
0.631433278272996));
#83376=CARTESIAN_POINT('Ctrl Pts',(-15.0211840009243,-2.51770995525376,
0.633996569152672));
#83377=CARTESIAN_POINT('Ctrl Pts',(-14.8108185964556,-2.51623745568275,
0.648060437220967));
#83378=CARTESIAN_POINT('Ctrl Pts',(-14.6398367497722,-2.49750295198875,
0.660066422047367));
#83379=CARTESIAN_POINT('Ctrl Pts',(-14.35541507125,-2.43650493710748,0.679999278915355));
#83380=CARTESIAN_POINT('Ctrl Pts',(-14.2406522768677,-2.40321527523799,
0.688039210490641));
#83381=CARTESIAN_POINT('Ctrl Pts',(-14.0863649710764,-2.34629722665468,
0.698772555634754));
#83382=CARTESIAN_POINT('Ctrl Pts',(-14.0444837528991,-2.32955548769909,
0.701679465851918));
#83383=CARTESIAN_POINT('Ctrl Pts',(-13.9702810714025,-2.29755531859551,
0.706821705188407));
#83384=CARTESIAN_POINT('Ctrl Pts',(-13.9377929040945,-2.28271719880701,
0.709070337008699));
#83385=CARTESIAN_POINT('Ctrl Pts',(-13.8673524649943,-2.24871571480265,
0.713944720421659));
#83386=CARTESIAN_POINT('Ctrl Pts',(-13.8295473321898,-2.22927200851229,
0.716560034462634));
#83387=CARTESIAN_POINT('Ctrl Pts',(-13.7113806484636,-2.16466200265832,
0.724750958268619));
#83388=CARTESIAN_POINT('Ctrl Pts',(-13.6329951294246,-2.11603438860291,
0.730206023229071));
#83389=CARTESIAN_POINT('Ctrl Pts',(-13.4196449813503,-1.96686468615854,
0.745380059179249));
#83390=CARTESIAN_POINT('Ctrl Pts',(-13.2918501599983,-1.85695934035244,
0.754848757100814));
#83391=CARTESIAN_POINT('Ctrl Pts',(-13.1317932005299,-1.68870299272427,
0.768507028295722));
#83392=CARTESIAN_POINT('Ctrl Pts',(-13.0894098215822,-1.64059692989384,
0.772336417259867));
#83393=CARTESIAN_POINT('Ctrl Pts',(-13.0322553293579,-1.57050369135047,
0.777898153398103));
#83394=CARTESIAN_POINT('Ctrl Pts',(-13.0159217702844,-1.54981753055592,
0.779537513498898));
#83395=CARTESIAN_POINT('Ctrl Pts',(-12.9874979582772,-1.51263344933187,
0.782488384671607));
#83396=CARTESIAN_POINT('Ctrl Pts',(-12.9752789007632,-1.49623821614062,
0.783791345813231));
#83397=CARTESIAN_POINT('Ctrl Pts',(-12.9463398442183,-1.45640482452355,
0.786961001506182));
#83398=CARTESIAN_POINT('Ctrl Pts',(-12.9298204131927,-1.43282635194578,
0.788839760972054));
#83399=CARTESIAN_POINT('Ctrl Pts',(-12.859914929169,-1.32931597502486,0.797080747082635));
#83400=CARTESIAN_POINT('Ctrl Pts',(-12.810730703438,-1.24665219944856,0.803641852284902));
#83401=CARTESIAN_POINT('Ctrl Pts',(-12.6708138783061,-0.977561493700402,
0.824522576820951));
#83402=CARTESIAN_POINT('Ctrl Pts',(-12.5982717066286,-0.782600715743599,
0.838889060123552));
#83403=CARTESIAN_POINT('Ctrl Pts',(-12.5404867268985,-0.538946144549989,
0.855297518861489));
#83404=CARTESIAN_POINT('Ctrl Pts',(-12.5316094548605,-0.496706126852236,
0.858092548642426));
#83405=CARTESIAN_POINT('Ctrl Pts',(-12.5172701717136,-0.41854189053908,
0.863176754644976));
#83406=CARTESIAN_POINT('Ctrl Pts',(-12.5114914821592,-0.382688246636222,
0.865475263860691));
#83407=CARTESIAN_POINT('Ctrl Pts',(-12.5011014050085,-0.307965941793777,
0.870200535121905));
#83408=CARTESIAN_POINT('Ctrl Pts',(-12.4966166167801,-0.269089410729553,
0.8726227556154));
#83409=CARTESIAN_POINT('Ctrl Pts',(-12.4867492458804,-0.161593964858977,
0.879232219953701));
#83410=CARTESIAN_POINT('Ctrl Pts',(-12.4832709270209,-0.0928327669313311,
0.883360757948777));
#83411=CARTESIAN_POINT('Ctrl Pts',(-12.4817107107369,0.0707466317847089,
0.893028132897282));
#83412=CARTESIAN_POINT('Ctrl Pts',(-12.486157761215,0.165483170982915,0.898502500759125));
#83413=CARTESIAN_POINT('Ctrl Pts',(-12.5127570854783,0.421911468866452,
0.913335932456505));
#83414=CARTESIAN_POINT('Ctrl Pts',(-12.5452893646556,0.582039038458692,
0.92260511854225));
#83415=CARTESIAN_POINT('Ctrl Pts',(-12.6020148425295,0.767076418174483,
0.934408471148048));
#83416=CARTESIAN_POINT('Ctrl Pts',(-12.6114967506365,0.796109965945524,
0.936294311449801));
#83417=CARTESIAN_POINT('Ctrl Pts',(-12.6282544910687,0.844425168184754,
0.939500706381289));
#83418=CARTESIAN_POINT('Ctrl Pts',(-12.6352429454685,0.863802444978699,
0.940805549043224));
#83419=CARTESIAN_POINT('Ctrl Pts',(-12.6513024419976,0.906675349002907,
0.943737317989772));
#83420=CARTESIAN_POINT('Ctrl Pts',(-12.6604889263279,0.930122692365925,
0.945370142445873));
#83421=CARTESIAN_POINT('Ctrl Pts',(-12.6920802357719,1.00732519022705,0.950835216511538));
#83422=CARTESIAN_POINT('Ctrl Pts',(-12.7159972599234,1.06043769478327,0.954739033353897));
#83423=CARTESIAN_POINT('Ctrl Pts',(-12.7858793703816,1.20227013016722,0.965474745974864));
#83424=CARTESIAN_POINT('Ctrl Pts',(-12.8353188496068,1.2891617342377,0.972391216390137));
#83425=CARTESIAN_POINT('Ctrl Pts',(-12.9696476981395,1.49563399758236,0.989385977156253));
#83426=CARTESIAN_POINT('Ctrl Pts',(-13.0600756031843,1.61119692168597,0.999389481879473));
#83427=CARTESIAN_POINT('Ctrl Pts',(-13.1949281767611,1.7556005442937,1.01238688813328));
#83428=CARTESIAN_POINT('Ctrl Pts',(-13.2309367079026,1.79187980681812,1.01570340736094));
#83429=CARTESIAN_POINT('Ctrl Pts',(-13.2943801234735,1.85202205188942,1.02129517969685));
#83430=CARTESIAN_POINT('Ctrl Pts',(-13.3212718329469,1.87643193530091,1.02359336432171));
#83431=CARTESIAN_POINT('Ctrl Pts',(-13.3783380026123,1.92602235013558,1.0283279114817));
#83432=CARTESIAN_POINT('Ctrl Pts',(-13.4085929465998,1.95109548331557,1.0307595055537));
#83433=CARTESIAN_POINT('Ctrl Pts',(-13.4940547484666,2.0186089966816,1.0374265119159));
#83434=CARTESIAN_POINT('Ctrl Pts',(-13.5504554580865,2.05948421306682,1.04160153626649));
#83435=CARTESIAN_POINT('Ctrl Pts',(-13.6889747025622,2.15135963635004,1.05142000406807));
#83436=CARTESIAN_POINT('Ctrl Pts',(-13.7724762227648,2.20007328514741,1.0569959252357));
#83437=CARTESIAN_POINT('Ctrl Pts',(-13.9999715471583,2.31579713311458,1.07168128872143));
#83438=CARTESIAN_POINT('Ctrl Pts',(-14.1478353813586,2.3741897242527,1.08071679832936));
#83439=CARTESIAN_POINT('Ctrl Pts',(-14.3299749299033,2.42689806436197,1.0922727402276));
#83440=CARTESIAN_POINT('Ctrl Pts',(-14.3599169434052,2.43496638285326,1.09418625867067));
#83441=CARTESIAN_POINT('Ctrl Pts',(-14.4100528989628,2.44748767584125,1.09742490045056));
#83442=CARTESIAN_POINT('Ctrl Pts',(-14.4301659690668,2.45224848932349,1.09873355378819));
#83443=CARTESIAN_POINT('Ctrl Pts',(-14.4746919515494,2.46221050552374,1.10165420826288));
#83444=CARTESIAN_POINT('Ctrl Pts',(-14.4991257142135,2.46729689157235,1.10327166891477));
#83445=CARTESIAN_POINT('Ctrl Pts',(-14.5792526385346,2.48273774149783,1.10861511016226));
#83446=CARTESIAN_POINT('Ctrl Pts',(-14.6352172406197,2.49157532250733,1.11240858962044));
#83447=CARTESIAN_POINT('Ctrl Pts',(-14.7857773839676,2.51016983045862,1.12269915252817));
#83448=CARTESIAN_POINT('Ctrl Pts',(-14.8807081588065,2.51646818946665,1.12927404051608));
#83449=CARTESIAN_POINT('Ctrl Pts',(-15.1294620771118,2.51886306153653,1.1464446892016));
#83450=CARTESIAN_POINT('Ctrl Pts',(-15.2829923890487,2.50626395564869,1.15696427808092));
#83451=CARTESIAN_POINT('Ctrl Pts',(-15.484634773469,2.47093771492628,1.17042905232434));
#83452=CARTESIAN_POINT('Ctrl Pts',(-15.5345628333025,2.46061928034601,1.17373658441706));
#83453=CARTESIAN_POINT('Ctrl Pts',(-15.6194404852995,2.44037216436577,1.17931759947465));
#83454=CARTESIAN_POINT('Ctrl Pts',(-15.6545499493115,2.43119053174039,1.18161381551733));
#83455=CARTESIAN_POINT('Ctrl Pts',(-15.7272600474732,2.41048637662271,1.18634782926339));
#83456=CARTESIAN_POINT('Ctrl Pts',(-15.7648140403433,2.39883544671789,1.18878078244725));
#83457=CARTESIAN_POINT('Ctrl Pts',(-15.8682717451064,2.36406145098872,1.19546137755397));
#83458=CARTESIAN_POINT('Ctrl Pts',(-15.9335113184679,2.33906823684261,1.19964812237518));
#83459=CARTESIAN_POINT('Ctrl Pts',(-16.0867423289768,2.27293144358567,1.20950448362295));
#83460=CARTESIAN_POINT('Ctrl Pts',(-16.1735575998852,2.22934749926156,1.21510571054418));
#83461=CARTESIAN_POINT('Ctrl Pts',(-16.3943467622135,2.10202431611659,1.22976762849102));
#83462=CARTESIAN_POINT('Ctrl Pts',(-16.5233200012927,2.01052072242488,1.23875740209731));
#83463=CARTESIAN_POINT('Ctrl Pts',(-16.666434569669,1.88726511987068,1.25026600172275));
#83464=CARTESIAN_POINT('Ctrl Pts',(-16.6896244614534,1.86653228762496,1.25218513990339));
#83465=CARTESIAN_POINT('Ctrl Pts',(-16.7275772563391,1.831313865884,1.25542963989552));
#83466=CARTESIAN_POINT('Ctrl Pts',(-16.7425561710251,1.8170667610702,1.25673834793639));
#83467=CARTESIAN_POINT('Ctrl Pts',(-16.7751757085839,1.78526653022033,1.2596540881484));
#83468=CARTESIAN_POINT('Ctrl Pts',(-16.7927331828004,1.76763486006384,1.26126646309826));
#83469=CARTESIAN_POINT('Ctrl Pts',(-16.8490524592795,1.70937538113403,1.26657177865021));
#83470=CARTESIAN_POINT('Ctrl Pts',(-16.8867148416647,1.6677126047612,1.27033099157672));
#83471=CARTESIAN_POINT('Ctrl Pts',(-16.9833698683707,1.55332348173811,1.28048653997405));
#83472=CARTESIAN_POINT('Ctrl Pts',(-17.0397521464408,1.47850594623718,1.28695867289338));
#83473=CARTESIAN_POINT('Ctrl Pts',(-17.1786906859522,1.27101598920294,1.30419664743113));
#83474=CARTESIAN_POINT('Ctrl Pts',(-17.253304957287,1.13349204240167,1.31488676720222));
#83475=CARTESIAN_POINT('Ctrl Pts',(-17.3312570993131,0.951219606211523,
1.32792444222788));
#83476=CARTESIAN_POINT('Ctrl Pts',(-17.3468371067832,0.912104217466158,
1.33066246219695));
#83477=CARTESIAN_POINT('Ctrl Pts',(-17.361429188522,0.872615859124936,1.33336838650867));
#83478=CARTESIAN_POINT('Origin',(-15.,0.,3.));
#83479=CARTESIAN_POINT('',(-17.3614291132577,0.87261606280125,2.3307189689843));
#83480=CARTESIAN_POINT('',(-17.3614291890287,0.872615857753798,2.05625951847909));
#83481=CARTESIAN_POINT('',(-17.3614291890287,0.872615857753799,3.));
#83482=CARTESIAN_POINT('',(-17.5174999225306,0.000624546553775974,1.11258330254393));
#83483=CARTESIAN_POINT('Ctrl Pts',(-17.3614291890287,0.872615857753798,
2.0562595184791));
#83484=CARTESIAN_POINT('Ctrl Pts',(-17.3579183588427,0.88211668999871,2.05561541020025));
#83485=CARTESIAN_POINT('Ctrl Pts',(-17.3543505691999,0.891595309335236,
2.05497130192141));
#83486=CARTESIAN_POINT('Ctrl Pts',(-17.3507261017234,0.901051077728782,
2.05432719364256));
#83487=CARTESIAN_POINT('Ctrl Pts',(-17.3211460982113,0.978221493550537,
2.04907049723843));
#83488=CARTESIAN_POINT('Ctrl Pts',(-17.2877077514437,1.05407531900084,2.0438138008343));
#83489=CARTESIAN_POINT('Ctrl Pts',(-17.2505489208352,1.12820025036668,2.03855710443017));
#83490=CARTESIAN_POINT('Ctrl Pts',(-17.2134425427188,1.2022205488011,2.03330782824949));
#83491=CARTESIAN_POINT('Ctrl Pts',(-17.1726263174307,1.27451639191413,2.02805855206882));
#83492=CARTESIAN_POINT('Ctrl Pts',(-17.1282867028638,1.34469400251988,2.02280927588814));
#83493=CARTESIAN_POINT('Ctrl Pts',(-17.0837624472362,1.41516384995711,2.01753814043034));
#83494=CARTESIAN_POINT('Ctrl Pts',(-17.0356855587209,1.48349734301016,2.01226700497253));
#83495=CARTESIAN_POINT('Ctrl Pts',(-16.9842922536276,1.54931936739762,2.00699586951473));
#83496=CARTESIAN_POINT('Ctrl Pts',(-16.9332028355715,1.61475218817319,2.00175590211925));
#83497=CARTESIAN_POINT('Ctrl Pts',(-16.8788363990628,1.67770279135969,1.99651593472378));
#83498=CARTESIAN_POINT('Ctrl Pts',(-16.821468216685,1.73783192098843,1.99127596732831));
#83499=CARTESIAN_POINT('Ctrl Pts',(-16.7641187321055,1.79794145295363,1.98603770777592));
#83500=CARTESIAN_POINT('Ctrl Pts',(-16.7037697628315,1.85523100441582,1.98079944822352));
#83501=CARTESIAN_POINT('Ctrl Pts',(-16.6407352069614,1.9093963000481,1.97556118867113));
#83502=CARTESIAN_POINT('Ctrl Pts',(-16.5777022129079,1.9635602536187,1.97032305890788));
#83503=CARTESIAN_POINT('Ctrl Pts',(-16.5119841149943,2.0145998055727,1.96508492914463));
#83504=CARTESIAN_POINT('Ctrl Pts',(-16.443928775299,2.06225021320485,1.95984679938138));
#83505=CARTESIAN_POINT('Ctrl Pts',(-16.3751293912855,2.11042157944539,1.954551401508));
#83506=CARTESIAN_POINT('Ctrl Pts',(-16.303941731054,2.15512895127721,1.94925600363462));
#83507=CARTESIAN_POINT('Ctrl Pts',(-16.2307547169103,2.1961441384397,1.94396060576124));
#83508=CARTESIAN_POINT('Ctrl Pts',(-16.1582556254288,2.23677380260915,1.93871498207588));
#83509=CARTESIAN_POINT('Ctrl Pts',(-16.0837950534331,2.27378024822346,1.93346935839053));
#83510=CARTESIAN_POINT('Ctrl Pts',(-16.0077736161152,2.30698907423987,1.92822373470517));
#83511=CARTESIAN_POINT('Ctrl Pts',(-15.9306701610406,2.34067056350356,1.92290344973778));
#83512=CARTESIAN_POINT('Ctrl Pts',(-15.8519615197173,2.37044530624312,1.91758316477039));
#83513=CARTESIAN_POINT('Ctrl Pts',(-15.7720823641435,2.39618343892504,1.912262879803));
#83514=CARTESIAN_POINT('Ctrl Pts',(-15.6922032085696,2.42192157160695,1.90694259483561));
#83515=CARTESIAN_POINT('Ctrl Pts',(-15.6111540266284,2.44362302983869,1.90162230986822));
#83516=CARTESIAN_POINT('Ctrl Pts',(-15.5293791044952,2.46121189939506,1.89630202490083));
#83517=CARTESIAN_POINT('Ctrl Pts',(-15.4485811111899,2.47859064250592,1.89104529902492));
#83518=CARTESIAN_POINT('Ctrl Pts',(-15.3667782505564,2.4920183248603,1.88578857314902));
#83519=CARTESIAN_POINT('Ctrl Pts',(-15.2843911870634,2.5013851967901,1.88053184727311));
#83520=CARTESIAN_POINT('Ctrl Pts',(-15.202120412429,2.51073884743493,1.87528254123506));
#83521=CARTESIAN_POINT('Ctrl Pts',(-15.1192675272454,2.51604302130111,1.87003323519701));
#83522=CARTESIAN_POINT('Ctrl Pts',(-15.0362642248042,2.51723879598248,1.86478392915895));
#83523=CARTESIAN_POINT('Ctrl Pts',(-14.9529158675402,2.51843954164464,1.85951280111729));
#83524=CARTESIAN_POINT('Ctrl Pts',(-14.8694162997541,2.51549755241802,1.85424167307563));
#83525=CARTESIAN_POINT('Ctrl Pts',(-14.7862087535634,2.50840577916474,1.84897054503397));
#83526=CARTESIAN_POINT('Ctrl Pts',(-14.7034926121531,2.50135588830601,1.8437305470717));
#83527=CARTESIAN_POINT('Ctrl Pts',(-14.6210655169452,2.4902051330005,1.83849054910942));
#83528=CARTESIAN_POINT('Ctrl Pts',(-14.5393620086488,2.47499876584291,1.83325055114714));
#83529=CARTESIAN_POINT('Ctrl Pts',(-14.4576851264548,2.45979735424106,1.82801226083152));
#83530=CARTESIAN_POINT('Ctrl Pts',(-14.3767318157995,2.44054304008941,1.82277397051589));
#83531=CARTESIAN_POINT('Ctrl Pts',(-14.2969284164376,2.41733253781665,1.81753568020027));
#83532=CARTESIAN_POINT('Ctrl Pts',(-14.2171269920321,2.3941226099521,1.81229751952065));
#83533=CARTESIAN_POINT('Ctrl Pts',(-14.138475864793,2.36695681844558,1.80705935884104));
#83534=CARTESIAN_POINT('Ctrl Pts',(-14.0613868143877,2.33598192154707,1.80182119816143));
#83535=CARTESIAN_POINT('Ctrl Pts',(-13.983455945087,2.30466877617673,1.7965258363279));
#83536=CARTESIAN_POINT('Ctrl Pts',(-13.9071219299059,2.26946298869584,1.79123047449437));
#83537=CARTESIAN_POINT('Ctrl Pts',(-13.8327883460253,2.23056566924753,1.78593511266085));
#83538=CARTESIAN_POINT('Ctrl Pts',(-13.7591525261008,2.19203347611339,1.78068945800447));
#83539=CARTESIAN_POINT('Ctrl Pts',(-13.6874801096723,2.14987905464921,1.77544380334809));
#83540=CARTESIAN_POINT('Ctrl Pts',(-13.6181360221196,2.10434269942812,1.77019814869171));
#83541=CARTESIAN_POINT('Ctrl Pts',(-13.5478062905234,2.05815909887048,1.76487793326961));
#83542=CARTESIAN_POINT('Ctrl Pts',(-13.4798719930558,2.00849695994764,1.7595577178475));
#83543=CARTESIAN_POINT('Ctrl Pts',(-13.4146793346692,1.95564941594221,1.7542375024254));
#83544=CARTESIAN_POINT('Ctrl Pts',(-13.3494866762826,1.90280187193678,1.7489172870033));
#83545=CARTESIAN_POINT('Ctrl Pts',(-13.2870359773928,1.84676929628926,1.7435970715812));
#83546=CARTESIAN_POINT('Ctrl Pts',(-13.2276335093517,1.78788234311626,1.7382768561591));
#83547=CARTESIAN_POINT('Ctrl Pts',(-13.1689417340556,1.7296999150544,1.73302029193916));
#83548=CARTESIAN_POINT('Ctrl Pts',(-13.1130102909223,1.66851762084859,1.72776372771923));
#83549=CARTESIAN_POINT('Ctrl Pts',(-13.0601608943265,1.60462783663376,1.72250716349929));
#83550=CARTESIAN_POINT('Ctrl Pts',(-13.0073861005807,1.54082824001408,1.71725801950924));
#83551=CARTESIAN_POINT('Ctrl Pts',(-12.9576850030239,1.47432909740031,1.71200887551918));
#83552=CARTESIAN_POINT('Ctrl Pts',(-12.9113427684534,1.40545978921783,1.70675973152913));
#83553=CARTESIAN_POINT('Ctrl Pts',(-12.8648060897557,1.33630151714207,1.70148856302447));
#83554=CARTESIAN_POINT('Ctrl Pts',(-12.8216568603807,1.26475347508018,1.69621739451981));
#83555=CARTESIAN_POINT('Ctrl Pts',(-12.7821431293703,1.19118308895007,1.69094622601516));
#83556=CARTESIAN_POINT('Ctrl Pts',(-12.7428642719539,1.11805001259977,1.68570638986662));
#83557=CARTESIAN_POINT('Ctrl Pts',(-12.7071780338311,1.04291897808977,1.68046655371808));
#83558=CARTESIAN_POINT('Ctrl Pts',(-12.6752838786094,0.966178660987118,
1.67522671756955));
#83559=CARTESIAN_POINT('Ctrl Pts',(-12.6434001148738,0.889463346770761,
1.66998858862046));
#83560=CARTESIAN_POINT('Ctrl Pts',(-12.6153061570237,0.811140216822043,
1.66475045967138));
#83561=CARTESIAN_POINT('Ctrl Pts',(-12.5911538838185,0.731619189577037,
1.6595123307223));
#83562=CARTESIAN_POINT('Ctrl Pts',(-12.5670022052839,0.652100120276801,
1.65427433074498));
#83563=CARTESIAN_POINT('Ctrl Pts',(-12.5467921514062,0.5713836538708,1.64903633076766));
#83564=CARTESIAN_POINT('Ctrl Pts',(-12.5306257299106,0.489894850167558,
1.64379833079034));
#83565=CARTESIAN_POINT('Ctrl Pts',(-12.5142816764258,0.407510670928604,
1.63850277717592));
#83566=CARTESIAN_POINT('Ctrl Pts',(-12.5020707728335,0.324337546161918,
1.63320722356151));
#83567=CARTESIAN_POINT('Ctrl Pts',(-12.4940450286002,0.240823444283986,
1.62791166994709));
#83568=CARTESIAN_POINT('Ctrl Pts',(-12.4860951479878,0.158098762300121,
1.62266617273368));
#83569=CARTESIAN_POINT('Ctrl Pts',(-12.48225159958,0.0750399909802926,1.61742067552027));
#83570=CARTESIAN_POINT('Ctrl Pts',(-12.4825124454019,-0.00791596132666538,
1.61217517830687));
#83571=CARTESIAN_POINT('Ctrl Pts',(-12.4827770249985,-0.0920593539025686,
1.60685459649195));
#83572=CARTESIAN_POINT('Ctrl Pts',(-12.4872644023026,-0.176096469374805,
1.60153401467703));
#83573=CARTESIAN_POINT('Ctrl Pts',(-12.4959181350515,-0.259577086115441,
1.59621343286211));
#83574=CARTESIAN_POINT('Ctrl Pts',(-12.5045718678004,-0.343057702856078,
1.59089285104719));
#83575=CARTESIAN_POINT('Ctrl Pts',(-12.5173918181152,-0.425981348228918,
1.58557226923227));
#83576=CARTESIAN_POINT('Ctrl Pts',(-12.5342682813868,-0.507910761674344,
1.58025168741735));
#83577=CARTESIAN_POINT('Ctrl Pts',(-12.5509424231166,-0.588857973756139,
1.57499489078646));
#83578=CARTESIAN_POINT('Ctrl Pts',(-12.5716374750143,-0.669131681034995,
1.56973809415557));
#83579=CARTESIAN_POINT('Ctrl Pts',(-12.5962842586559,-0.748302669255232,
1.56448129752468));
#83580=CARTESIAN_POINT('Ctrl Pts',(-12.6208962491726,-0.82736189416728,
1.55923192175584));
#83581=CARTESIAN_POINT('Ctrl Pts',(-12.6494487546389,-0.905321055478407,
1.553982545987));
#83582=CARTESIAN_POINT('Ctrl Pts',(-12.6818216371413,-0.981761339620741,
1.54873317021816));
#83583=CARTESIAN_POINT('Ctrl Pts',(-12.7143285575393,-1.05851811997933,
1.54346205973722));
#83584=CARTESIAN_POINT('Ctrl Pts',(-12.7506874683974,-1.13374295575044,
1.53819094925628));
#83585=CARTESIAN_POINT('Ctrl Pts',(-12.7907261182731,-1.20702740876898,
1.53291983877534));
#83586=CARTESIAN_POINT('Ctrl Pts',(-12.8305289487565,-1.27988023146951,
1.5276797740483));
#83587=CARTESIAN_POINT('Ctrl Pts',(-12.8739680684985,-1.35081505642381,
1.52243970932127));
#83588=CARTESIAN_POINT('Ctrl Pts',(-12.9208268601991,-1.41945246652737,
1.51719964459423));
#83589=CARTESIAN_POINT('Ctrl Pts',(-12.9676703702129,-1.48806749245554,
1.51196128876803));
#83590=CARTESIAN_POINT('Ctrl Pts',(-13.0179310774233,-1.55438621109506,
1.50672293294184));
#83591=CARTESIAN_POINT('Ctrl Pts',(-13.0713485773765,-1.61805745881054,
1.50148457711564));
#83592=CARTESIAN_POINT('Ctrl Pts',(-13.1247647417676,-1.6817271145962,1.49624635226057));
#83593=CARTESIAN_POINT('Ctrl Pts',(-13.18133724479,-1.74274907852124,1.4910081274055));
#83594=CARTESIAN_POINT('Ctrl Pts',(-13.2407657562769,-1.80080568793864,
1.48576990255042));
#83595=CARTESIAN_POINT('Ctrl Pts',(-13.3008415902188,-1.85949467642785,
1.48047462056086));
#83596=CARTESIAN_POINT('Ctrl Pts',(-13.3638356979858,-1.91515296809219,
1.47517933857129));
#83597=CARTESIAN_POINT('Ctrl Pts',(-13.4294013462705,-1.96749234278134,
1.46988405658172));
#83598=CARTESIAN_POINT('Ctrl Pts',(-13.4943532602625,-2.01934178913228,
1.46463834164795));
#83599=CARTESIAN_POINT('Ctrl Pts',(-13.5618283590093,-2.06793397067668,
1.45939262671418));
#83600=CARTESIAN_POINT('Ctrl Pts',(-13.6314596067478,-2.11303181283129,
1.45414691178041));
#83601=CARTESIAN_POINT('Ctrl Pts',(-13.7020777788575,-2.15876885306085,
1.44882684626295));
#83602=CARTESIAN_POINT('Ctrl Pts',(-13.7749132735029,-2.2009114778222,1.44350678074548));
#83603=CARTESIAN_POINT('Ctrl Pts',(-13.8495582965948,-2.23926106943028,
1.43818671522802));
#83604=CARTESIAN_POINT('Ctrl Pts',(-13.9242033196866,-2.27761066103836,
1.43286664971055));
#83605=CARTESIAN_POINT('Ctrl Pts',(-14.0006574004068,-2.31216707685132,
1.42754658419309));
#83606=CARTESIAN_POINT('Ctrl Pts',(-14.0784945104588,-2.34278336231618,
1.42222651867563));
#83607=CARTESIAN_POINT('Ctrl Pts',(-14.1554076983103,-2.37303623416223,
1.41696960204225));
#83608=CARTESIAN_POINT('Ctrl Pts',(-14.2339532309517,-2.399552974658,1.41171268540887));
#83609=CARTESIAN_POINT('Ctrl Pts',(-14.3137337737756,-2.42215707928773,
1.40645576877549));
#83610=CARTESIAN_POINT('Ctrl Pts',(-14.3934017384898,-2.44472928732614,
1.40120627016305));
#83611=CARTESIAN_POINT('Ctrl Pts',(-14.4743008117969,-2.46339970165732,
1.39595677155062));
#83612=CARTESIAN_POINT('Ctrl Pts',(-14.5560145367786,-2.4780401849946,1.39070727293818));
#83613=CARTESIAN_POINT('Ctrl Pts',(-14.6380641997092,-2.49274085765681,
1.385436192813));
#83614=CARTESIAN_POINT('Ctrl Pts',(-14.720934789805,-2.50337821665985,1.38016511268782));
#83615=CARTESIAN_POINT('Ctrl Pts',(-14.8041901146933,-2.50987345075726,
1.37489403256264));
#83616=CARTESIAN_POINT('Ctrl Pts',(-14.886957593483,-2.51633062513155,1.36965383906096));
#83617=CARTESIAN_POINT('Ctrl Pts',(-14.9701048461394,-2.51869404784475,
1.36441364555928));
#83618=CARTESIAN_POINT('Ctrl Pts',(-15.0531957172911,-2.51693791454257,
1.3591734520576));
#83619=CARTESIAN_POINT('Ctrl Pts',(-15.1362595218497,-2.51518235329535,
1.35393496553267));
#83620=CARTESIAN_POINT('Ctrl Pts',(-15.2192665207753,-2.50930991101445,
1.34869647900775));
#83621=CARTESIAN_POINT('Ctrl Pts',(-15.301780307132,-2.49934689393595,1.34345799248282));
#83622=CARTESIAN_POINT('Ctrl Pts',(-15.3842920577936,-2.48938412265476,
1.33821963519645));
#83623=CARTESIAN_POINT('Ctrl Pts',(-15.4663101624699,-2.47533103357443,
1.33298127791007));
#83624=CARTESIAN_POINT('Ctrl Pts',(-15.5474044670369,-2.45726567539369,
1.3277429206237));
#83625=CARTESIAN_POINT('Ctrl Pts',(-15.629377676138,-2.43900452386718,1.32244778973288));
#83626=CARTESIAN_POINT('Ctrl Pts',(-15.7104064662015,-2.41664369278313,
1.31715265884206));
#83627=CARTESIAN_POINT('Ctrl Pts',(-15.790060066662,-2.3903161592279,1.31185752795124));
#83628=CARTESIAN_POINT('Ctrl Pts',(-15.8689723476672,-2.36423365053935,
1.30661167773983));
#83629=CARTESIAN_POINT('Ctrl Pts',(-15.946534517254,-2.33425819292832,1.30136582752842));
#83630=CARTESIAN_POINT('Ctrl Pts',(-16.0223474854582,-2.30056772753537,
1.296119977317));
#83631=CARTESIAN_POINT('Ctrl Pts',(-16.0992287593984,-2.2664025185955,1.29080020608648));
#83632=CARTESIAN_POINT('Ctrl Pts',(-16.1743107126428,-2.22841701001766,
1.28548043485596));
#83633=CARTESIAN_POINT('Ctrl Pts',(-16.2472042958861,-2.18684423183801,
1.28016066362544));
#83634=CARTESIAN_POINT('Ctrl Pts',(-16.3200978791295,-2.14527145365836,
1.27484089239492));
#83635=CARTESIAN_POINT('Ctrl Pts',(-16.3908027158774,-2.10011172217429,
1.2695211211644));
#83636=CARTESIAN_POINT('Ctrl Pts',(-16.458963058855,-2.05164154834528,1.26420134993388));
#83637=CARTESIAN_POINT('Ctrl Pts',(-16.5258768594739,-2.00405781554877,
1.25897886870935));
#83638=CARTESIAN_POINT('Ctrl Pts',(-16.5905910504883,-1.9531040037354,1.25375638748483));
#83639=CARTESIAN_POINT('Ctrl Pts',(-16.6527433969628,-1.89901172028921,
1.2485339062603));
#83640=CARTESIAN_POINT('Ctrl Pts',(-16.7148077447634,-1.84499602364115,
1.24331881930885));
#83641=CARTESIAN_POINT('Ctrl Pts',(-16.7743171005252,-1.78785098331981,
1.2381037323574));
#83642=CARTESIAN_POINT('Ctrl Pts',(-16.8309390359885,-1.72785083166735,
1.23288864540595));
#83643=CARTESIAN_POINT('Ctrl Pts',(-16.8874968861012,-1.66791858886896,
1.22767946094923));
#83644=CARTESIAN_POINT('Ctrl Pts',(-16.9411734901439,-1.6051379942373,1.22247027649251));
#83645=CARTESIAN_POINT('Ctrl Pts',(-16.99167143653,-1.53982178803601,1.21726109203579));
#83646=CARTESIAN_POINT('Ctrl Pts',(-17.0421384923936,-1.47454553695928,
1.212055094133));
#83647=CARTESIAN_POINT('Ctrl Pts',(-17.0894304642487,-1.40673712186122,
1.20684909623022));
#83648=CARTESIAN_POINT('Ctrl Pts',(-17.1332894007877,-1.33674327471159,
1.20164309832743));
#83649=CARTESIAN_POINT('Ctrl Pts',(-17.1771351667822,-1.26677044624498,
1.19643866375091));
#83650=CARTESIAN_POINT('Ctrl Pts',(-17.2175496963465,-1.19461388511103,
1.19123422917439));
#83651=CARTESIAN_POINT('Ctrl Pts',(-17.2543185061784,-1.12064906313328,
1.18602979459787));
#83652=CARTESIAN_POINT('Ctrl Pts',(-17.2910877251957,-1.04668341803063,
1.18082530210328));
#83653=CARTESIAN_POINT('Ctrl Pts',(-17.3242109373603,-0.970909891917941,
1.17562080960869));
#83654=CARTESIAN_POINT('Ctrl Pts',(-17.3535204181281,-0.893726966950397,
1.1704163171141));
#83655=CARTESIAN_POINT('Ctrl Pts',(-17.3828581303628,-0.816469697875104,
1.16520681155022));
#83656=CARTESIAN_POINT('Ctrl Pts',(-17.4083746099405,-0.737800757540424,
1.15999730598634));
#83657=CARTESIAN_POINT('Ctrl Pts',(-17.4299511964776,-0.65813633294112,
1.15478780042246));
#83658=CARTESIAN_POINT('Ctrl Pts',(-17.4515386754913,-0.578431691466635,
1.14957566495149));
#83659=CARTESIAN_POINT('Ctrl Pts',(-17.4691822018905,-0.497731022518042,
1.14436352948052));
#83660=CARTESIAN_POINT('Ctrl Pts',(-17.4828142452473,-0.416460890837208,
1.13915139400955));
#83661=CARTESIAN_POINT('Ctrl Pts',(-17.4964690143288,-0.335055275239358,
1.13393056948499));
#83662=CARTESIAN_POINT('Ctrl Pts',(-17.5060988917234,-0.25307876606046,
1.12870974496043));
#83663=CARTESIAN_POINT('Ctrl Pts',(-17.5116882685441,-0.170962837066912,
1.12348892043587));
#83664=CARTESIAN_POINT('Ctrl Pts',(-17.5155800936491,-0.113786367447792,
1.11985371447189));
#83665=CARTESIAN_POINT('Ctrl Pts',(-17.517514104616,-0.0565423669010007,
1.11621850850791));
#83666=CARTESIAN_POINT('Ctrl Pts',(-17.5174999225306,0.000624546553782374,
1.11258330254393));
#83667=CARTESIAN_POINT('Ctrl Pts',(-17.5174999225304,0.000624547370669188,
1.11258330249198));
#83668=CARTESIAN_POINT('Ctrl Pts',(-17.5174915904523,0.0342104800950757,
1.11044759539204));
#83669=CARTESIAN_POINT('Ctrl Pts',(-17.5168111821614,0.0677873313081131,
1.10831188829209));
#83670=CARTESIAN_POINT('Ctrl Pts',(-17.5154596174,0.10133687990857,1.10617618119214));
#83671=CARTESIAN_POINT('Ctrl Pts',(-17.5121328106533,0.183917358347414,
1.10091924864084));
#83672=CARTESIAN_POINT('Ctrl Pts',(-17.5047290348594,0.266485049122924,
1.09566231608955));
#83673=CARTESIAN_POINT('Ctrl Pts',(-17.4932470011056,0.348605280335514,
1.09040538353826));
#83674=CARTESIAN_POINT('Ctrl Pts',(-17.4817792084923,0.430623658011649,
1.08515497114849));
#83675=CARTESIAN_POINT('Ctrl Pts',(-17.4662432595015,0.512195225028043,
1.07990455875871));
#83676=CARTESIAN_POINT('Ctrl Pts',(-17.4466898348291,0.592887090552553,
1.07465414636895));
#83677=CARTESIAN_POINT('Ctrl Pts',(-17.4271585183416,0.673487721384712,
1.06940967038622));
#83678=CARTESIAN_POINT('Ctrl Pts',(-17.4036188623419,0.753210181893953,
1.0641651944035));
#83679=CARTESIAN_POINT('Ctrl Pts',(-17.376172897285,0.831630093375674,1.05892071842078));
#83680=CARTESIAN_POINT('Ctrl Pts',(-17.371377231226,0.845332497611128,1.05800434490594));
#83681=CARTESIAN_POINT('Ctrl Pts',(-17.3664624273925,0.858995160992436,
1.05708797139109));
#83682=CARTESIAN_POINT('Ctrl Pts',(-17.3614291890287,0.872615857753796,
1.05617159787625));
#83683=CARTESIAN_POINT('',(-17.5174990715549,-0.00216211011121049,1.38677810957484));
#83684=CARTESIAN_POINT('Ctrl Pts',(-17.361429188522,0.872615859124936,1.33336838650867));
#83685=CARTESIAN_POINT('Ctrl Pts',(-17.3644697119384,0.864387747443512,
1.33393221464368));
#83686=CARTESIAN_POINT('Ctrl Pts',(-17.3674673419817,0.856143442814553,
1.3344946565356));
#83687=CARTESIAN_POINT('Ctrl Pts',(-17.3826366100634,0.813734815422654,
1.33737516686039));
#83688=CARTESIAN_POINT('Ctrl Pts',(-17.3941124149619,0.779325048998579,
1.33967013449361));
#83689=CARTESIAN_POINT('Ctrl Pts',(-17.4164783306267,0.707097202009639,
1.34440453398241));
#83690=CARTESIAN_POINT('Ctrl Pts',(-17.4272334213277,0.669247459917327,
1.3468390565592));
#83691=CARTESIAN_POINT('Ctrl Pts',(-17.4546538286454,0.563368980426638,
1.35353294537761));
#83692=CARTESIAN_POINT('Ctrl Pts',(-17.4693750492632,0.494871834409698,
1.3577309577425));
#83693=CARTESIAN_POINT('Ctrl Pts',(-17.5054861443727,0.284467611793582,
1.37033664236042));
#83694=CARTESIAN_POINT('Ctrl Pts',(-17.5176222639292,0.141279561221942,
1.37850634702139));
#83695=CARTESIAN_POINT('Ctrl Pts',(-17.5174990715549,-0.00216211011121049,
1.38677810957484));
#83696=CARTESIAN_POINT('Ctrl Pts',(-17.5174990700656,-0.00216384354887156,
1.38677820953593));
#83697=CARTESIAN_POINT('Ctrl Pts',(-17.51741074099,-0.104929297953376,1.39270432233761));
#83698=CARTESIAN_POINT('Ctrl Pts',(-17.5110300750471,-0.207586802734071,
1.3986753730216));
#83699=CARTESIAN_POINT('Ctrl Pts',(-17.4951445603227,-0.335795742753872,
1.40649579315783));
#83700=CARTESIAN_POINT('Ctrl Pts',(-17.4914808689594,-0.361978067002406,
1.4081122615719));
#83701=CARTESIAN_POINT('Ctrl Pts',(-17.4837484833002,-0.411536795135612,
1.41121705589603));
#83702=CARTESIAN_POINT('Ctrl Pts',(-17.4797602707,-0.434922935711898,1.41270135868087));
#83703=CARTESIAN_POINT('Ctrl Pts',(-17.4716560460498,-0.478701706731114,
1.41552195544408));
#83704=CARTESIAN_POINT('Ctrl Pts',(-17.4676167067343,-0.499105799734577,
1.41685425623413));
#83705=CARTESIAN_POINT('Ctrl Pts',(-17.4564238192827,-0.552183836688912,
1.42036299168395));
#83706=CARTESIAN_POINT('Ctrl Pts',(-17.4488712189477,-0.584768729881325,
1.42255945597878));
#83707=CARTESIAN_POINT('Ctrl Pts',(-17.4102116686093,-0.737647178732982,
1.43303559146702));
#83708=CARTESIAN_POINT('Ctrl Pts',(-17.3708778124791,-0.855673738076037,
1.44161771255737));
#83709=CARTESIAN_POINT('Ctrl Pts',(-17.2788507738176,-1.07599470455397,
1.4581025758057));
#83710=CARTESIAN_POINT('Ctrl Pts',(-17.2275401150562,-1.17855597735989,
1.46598750706981));
#83711=CARTESIAN_POINT('Ctrl Pts',(-17.1304437310446,-1.34347210301674,
1.47885632062811));
#83712=CARTESIAN_POINT('Ctrl Pts',(-17.0884552579023,-1.40785808502855,
1.48393584376869));
#83713=CARTESIAN_POINT('Ctrl Pts',(-17.0199887772231,-1.50302492600982,
1.49152602486034));
#83714=CARTESIAN_POINT('Ctrl Pts',(-16.9956066370565,-1.53525015779285,
1.49411198496748));
#83715=CARTESIAN_POINT('Ctrl Pts',(-16.9480725587814,-1.59502764224625,
1.49894337157539));
#83716=CARTESIAN_POINT('Ctrl Pts',(-16.9250853592536,-1.62269727486359,
1.5011944533973));
#83717=CARTESIAN_POINT('Ctrl Pts',(-16.8697954236546,-1.68642031891409,
1.50642021843077));
#83718=CARTESIAN_POINT('Ctrl Pts',(-16.8370297964,-1.72205412664812,1.5093749748587));
#83719=CARTESIAN_POINT('Ctrl Pts',(-16.6757701912873,-1.88758520926889,
1.5233064672854));
#83720=CARTESIAN_POINT('Ctrl Pts',(-16.5344199516149,-2.0041818450257,1.53370215386311));
#83721=CARTESIAN_POINT('Ctrl Pts',(-16.3147676298489,-2.14839492329636,
1.5488468285158));
#83722=CARTESIAN_POINT('Ctrl Pts',(-16.2457951060086,-2.18911119093644,
1.55348594542009));
#83723=CARTESIAN_POINT('Ctrl Pts',(-16.1297280120013,-2.25036481123439,
1.56128820626082));
#83724=CARTESIAN_POINT('Ctrl Pts',(-16.0837362709733,-2.27287089488973,
1.56437912776286));
#83725=CARTESIAN_POINT('Ctrl Pts',(-16.0151056212476,-2.30389868207061,
1.56903615911648));
#83726=CARTESIAN_POINT('Ctrl Pts',(-15.9929764674198,-2.31352246331369,
1.57054442940889));
#83727=CARTESIAN_POINT('Ctrl Pts',(-15.9516568138439,-2.33079002381752,
1.57337910231776));
#83728=CARTESIAN_POINT('Ctrl Pts',(-15.932504673425,-2.33851827849744,1.57470072485983));
#83729=CARTESIAN_POINT('Ctrl Pts',(-15.8830141027774,-2.35778409374209,
1.57813284331709));
#83730=CARTESIAN_POINT('Ctrl Pts',(-15.8525443724825,-2.36897184358824,
1.5802617180655));
#83731=CARTESIAN_POINT('Ctrl Pts',(-15.6851471818416,-2.42678846124556,
1.59201154403098));
#83732=CARTESIAN_POINT('Ctrl Pts',(-15.5446197952672,-2.46213581091885,
1.60205391088852));
#83733=CARTESIAN_POINT('Ctrl Pts',(-15.3000216729287,-2.50168594680716,
1.61914428558574));
#83734=CARTESIAN_POINT('Ctrl Pts',(-15.1972744133894,-2.51187807177734,
1.62621330117869));
#83735=CARTESIAN_POINT('Ctrl Pts',(-15.0218425278818,-2.51844592440845,
1.63798321193597));
#83736=CARTESIAN_POINT('Ctrl Pts',(-14.9494121099834,-2.51803286362245,
1.64275764569538));
#83737=CARTESIAN_POINT('Ctrl Pts',(-14.8374217325841,-2.51255889790163,
1.65000628215555));
#83738=CARTESIAN_POINT('Ctrl Pts',(-14.7977990828646,-2.50968105360116,
1.65254522002841));
#83739=CARTESIAN_POINT('Ctrl Pts',(-14.7222821257896,-2.50239593756581,
1.65733920875892));
#83740=CARTESIAN_POINT('Ctrl Pts',(-14.6863825826926,-2.49815071133972,
1.65959867450862));
#83741=CARTESIAN_POINT('Ctrl Pts',(-14.6011634235553,-2.48620717972852,
1.66492234893989));
#83742=CARTESIAN_POINT('Ctrl Pts',(-14.5519560815547,-2.47781232388039,
1.66796416099419));
#83743=CARTESIAN_POINT('Ctrl Pts',(-14.3887109287107,-2.44493972746542,
1.67798371300989));
#83744=CARTESIAN_POINT('Ctrl Pts',(-14.2761261381144,-2.41400389357336,
1.68476868986902));
#83745=CARTESIAN_POINT('Ctrl Pts',(-14.0497333614593,-2.33452464324547,
1.69860126208235));
#83746=CARTESIAN_POINT('Ctrl Pts',(-13.9365473921558,-2.28518661595405,
1.70562348887135));
#83747=CARTESIAN_POINT('Ctrl Pts',(-13.7699258323203,-2.19748667984402,
1.71669718811635));
#83748=CARTESIAN_POINT('Ctrl Pts',(-13.7136125135431,-2.16500254353319,
1.72058055858812));
#83749=CARTESIAN_POINT('Ctrl Pts',(-13.6365675149431,-2.11649177913667,
1.7261830698941));
#83750=CARTESIAN_POINT('Ctrl Pts',(-13.6147293085288,-2.10226320281731,
1.72780516773122));
#83751=CARTESIAN_POINT('Ctrl Pts',(-13.5761280782184,-2.07625015261861,
1.73074128529458));
#83752=CARTESIAN_POINT('Ctrl Pts',(-13.5592813794292,-2.06459577281768,
1.73204728911199));
#83753=CARTESIAN_POINT('Ctrl Pts',(-13.5187576025879,-2.03582433159446,
1.73524821981792));
#83754=CARTESIAN_POINT('Ctrl Pts',(-13.4952337354723,-2.0184989619937,1.7371559007093));
#83755=CARTESIAN_POINT('Ctrl Pts',(-13.3932583319858,-1.9406206173743,1.74562723661071));
#83756=CARTESIAN_POINT('Ctrl Pts',(-13.3181257297811,-1.87587915831881,
1.75240065805066));
#83757=CARTESIAN_POINT('Ctrl Pts',(-13.1485513295577,-1.71136289228862,
1.7686757924878));
#83758=CARTESIAN_POINT('Ctrl Pts',(-13.0580568401493,-1.60794485962692,
1.77818910802633));
#83759=CARTESIAN_POINT('Ctrl Pts',(-12.92628381013,-1.42990023747465,1.79315092028478));
#83760=CARTESIAN_POINT('Ctrl Pts',(-12.8795623454426,-1.35965445253963,
1.79874748437558));
#83761=CARTESIAN_POINT('Ctrl Pts',(-12.8152444318241,-1.25154681982423,
1.80690886825791));
#83762=CARTESIAN_POINT('Ctrl Pts',(-12.7949220216378,-1.2153837985722,1.80956844024252));
#83763=CARTESIAN_POINT('Ctrl Pts',(-12.7587470892079,-1.14711467822045,
1.81446383365772));
#83764=CARTESIAN_POINT('Ctrl Pts',(-12.7426681718462,-1.11514121202083,
1.81670716260732));
#83765=CARTESIAN_POINT('Ctrl Pts',(-12.7076214894262,-1.04158292537489,
1.82176278251821));
#83766=CARTESIAN_POINT('Ctrl Pts',(-12.6890931827839,-0.999802135017713,
1.82455957570571));
#83767=CARTESIAN_POINT('Ctrl Pts',(-12.5957800124775,-0.772907773260703,
1.83939378298238));
#83768=CARTESIAN_POINT('Ctrl Pts',(-12.5420789946517,-0.579905236458507,
1.85069849313828));
#83769=CARTESIAN_POINT('Ctrl Pts',(-12.5006395735616,-0.310384398969156,
1.86644851325316));
#83770=CARTESIAN_POINT('Ctrl Pts',(-12.4926875744485,-0.23774824482131,
1.87069821484972));
#83771=CARTESIAN_POINT('Ctrl Pts',(-12.4847373231454,-0.116614366871532,
1.87793454077127));
#83772=CARTESIAN_POINT('Ctrl Pts',(-12.4829614961188,-0.0682770984409923,
1.88086159378687));
#83773=CARTESIAN_POINT('Ctrl Pts',(-12.4823915276552,0.00374558707273863,
1.88532066291344));
#83774=CARTESIAN_POINT('Ctrl Pts',(-12.4825380175491,0.027413775255064,
1.88680173826362));
#83775=CARTESIAN_POINT('Ctrl Pts',(-12.4834406661178,0.0718961410599484,
1.88962072421106));
#83776=CARTESIAN_POINT('Ctrl Pts',(-12.4841214615025,0.0927091808764392,
1.89095475279585));
#83777=CARTESIAN_POINT('Ctrl Pts',(-12.4865752790908,0.14707614294081,1.89447540692934));
#83778=CARTESIAN_POINT('Ctrl Pts',(-12.4887620110582,0.180606545600921,
1.89668231750773));
#83779=CARTESIAN_POINT('Ctrl Pts',(-12.5018894485058,0.334420250930173,
1.90694011608563));
#83780=CARTESIAN_POINT('Ctrl Pts',(-12.5208057433837,0.453855449612457,
1.91527511630195));
#83781=CARTESIAN_POINT('Ctrl Pts',(-12.5746765633848,0.684981153922177,
1.93166030484436));
#83782=CARTESIAN_POINT('Ctrl Pts',(-12.6089896275729,0.796533844033761,
1.93969037957492));
#83783=CARTESIAN_POINT('Ctrl Pts',(-12.6788026686794,0.977683206159806,
1.95275092826776));
#83784=CARTESIAN_POINT('Ctrl Pts',(-12.7100246190622,1.04873079468747,1.95788126928044));
#83785=CARTESIAN_POINT('Ctrl Pts',(-12.7624746842335,1.15452495130637,1.9655279382062));
#83786=CARTESIAN_POINT('Ctrl Pts',(-12.7813432755363,1.19038231334867,1.96812139822791));
#83787=CARTESIAN_POINT('Ctrl Pts',(-12.8185698656697,1.25716371334219,1.97295889718402));
#83788=CARTESIAN_POINT('Ctrl Pts',(-12.836740667003,1.28817984125442,1.97520878757044));
#83789=CARTESIAN_POINT('Ctrl Pts',(-12.8808052193339,1.35983097479106,1.98042007034532));
#83790=CARTESIAN_POINT('Ctrl Pts',(-12.9072139489706,1.40013349607472,1.98336189575687));
#83791=CARTESIAN_POINT('Ctrl Pts',(-13.0402730523914,1.59101138787177,1.99739280564575));
#83792=CARTESIAN_POINT('Ctrl Pts',(-13.1620991728174,1.73031017383203,2.00788578632071));
#83793=CARTESIAN_POINT('Ctrl Pts',(-13.3564731192859,1.90864067087109,2.02309228407537));
#83794=CARTESIAN_POINT('Ctrl Pts',(-13.4173788092537,1.95943833674866,2.02768791156971));
#83795=CARTESIAN_POINT('Ctrl Pts',(-13.521149642625,2.03798857909398,2.03542747270723));
#83796=CARTESIAN_POINT('Ctrl Pts',(-13.5626430888984,2.06746225958091,2.03850063859477));
#83797=CARTESIAN_POINT('Ctrl Pts',(-13.6250440309144,2.1090002945182,2.04313621795057));
#83798=CARTESIAN_POINT('Ctrl Pts',(-13.6452796817278,2.12205535097268,2.04464155400268));
#83799=CARTESIAN_POINT('Ctrl Pts',(-13.6832257670378,2.14577237408993,2.0474743278546));
#83800=CARTESIAN_POINT('Ctrl Pts',(-13.700885631735,2.15650995782518,2.04879707906495));
#83801=CARTESIAN_POINT('Ctrl Pts',(-13.7467085747113,2.18360424707422,2.05223766802096));
#83802=CARTESIAN_POINT('Ctrl Pts',(-13.7750598594629,2.19963367834657,2.05437406875671));
#83803=CARTESIAN_POINT('Ctrl Pts',(-13.9298220662405,2.28321430957237,2.06604533588087));
#83804=CARTESIAN_POINT('Ctrl Pts',(-14.0615086621974,2.34042240477489,2.07599291910889));
#83805=CARTESIAN_POINT('Ctrl Pts',(-14.3432295227119,2.43519038608521,2.09649672266226));
#83806=CARTESIAN_POINT('Ctrl Pts',(-14.4933357030283,2.47079013715364,2.10699315412295));
#83807=CARTESIAN_POINT('Ctrl Pts',(-14.6924010604153,2.49908128460314,2.12015392998989));
#83808=CARTESIAN_POINT('Ctrl Pts',(-14.7392086029188,2.50439867176429,2.12319754377254));
#83809=CARTESIAN_POINT('Ctrl Pts',(-14.8218461732262,2.5114441320951,2.12848549235195));
#83810=CARTESIAN_POINT('Ctrl Pts',(-14.8576141947806,2.51372570310347,2.13074631920287));
#83811=CARTESIAN_POINT('Ctrl Pts',(-14.9344821854733,2.51698287105086,2.13554992572323));
#83812=CARTESIAN_POINT('Ctrl Pts',(-14.975582230692,2.51771710722279,2.13808460016937));
#83813=CARTESIAN_POINT('Ctrl Pts',(-15.0982874490642,2.51690390813561,2.14556671967149));
#83814=CARTESIAN_POINT('Ctrl Pts',(-15.1798211683558,2.5123956434932,2.15042415253401));
#83815=CARTESIAN_POINT('Ctrl Pts',(-15.3062221260613,2.4992202191508,2.15787237779834));
#83816=CARTESIAN_POINT('Ctrl Pts',(-15.3513112372926,2.4932818327974,2.16051331582906));
#83817=CARTESIAN_POINT('Ctrl Pts',(-15.5284859290761,2.46504536084989,2.17088356622319));
#83818=CARTESIAN_POINT('Ctrl Pts',(-15.6588566633258,2.43344427486408,2.17848822351278));
#83819=CARTESIAN_POINT('Ctrl Pts',(-15.8503054310333,2.37051812648493,2.19032009531502));
#83820=CARTESIAN_POINT('Ctrl Pts',(-15.9136405727218,2.34683507862466,2.19435203607397));
#83821=CARTESIAN_POINT('Ctrl Pts',(-16.0002522883677,2.31041061455897,2.20012982753585));
#83822=CARTESIAN_POINT('Ctrl Pts',(-16.0244007212841,2.29980539971069,2.20177019813175));
#83823=CARTESIAN_POINT('Ctrl Pts',(-16.0669780447957,2.28030320266165,2.2047227136022));
#83824=CARTESIAN_POINT('Ctrl Pts',(-16.0854725850685,2.27155761974723,2.20602629616552));
#83825=CARTESIAN_POINT('Ctrl Pts',(-16.1297459239671,2.24995779261166,2.20919749154462));
#83826=CARTESIAN_POINT('Ctrl Pts',(-16.1554133750856,2.23688526346347,2.21107717725398));
#83827=CARTESIAN_POINT('Ctrl Pts',(-16.2604189583063,2.18111611071466,2.21892147788057));
#83828=CARTESIAN_POINT('Ctrl Pts',(-16.3376557556887,2.13461885474172,2.22505880398839));
#83829=CARTESIAN_POINT('Ctrl Pts',(-16.514387399488,2.01486129009422,2.23973937716109));
#83830=CARTESIAN_POINT('Ctrl Pts',(-16.6113240810356,1.93821364535464,2.24830757315026));
#83831=CARTESIAN_POINT('Ctrl Pts',(-16.7769960424481,1.78616469138696,2.26362274608836));
#83832=CARTESIAN_POINT('Ctrl Pts',(-16.8475341111643,1.71310279774354,2.27041108134033));
#83833=CARTESIAN_POINT('Ctrl Pts',(-16.9417663073569,1.60288644711555,2.27985280603844));
#83834=CARTESIAN_POINT('Ctrl Pts',(-16.969194033204,1.56906870448489,2.28265325612637));
#83835=CARTESIAN_POINT('Ctrl Pts',(-17.0174709722588,1.50628316749648,2.28768464482899));
#83836=CARTESIAN_POINT('Ctrl Pts',(-17.0386072114135,1.47755167462609,2.28992644383609));
#83837=CARTESIAN_POINT('Ctrl Pts',(-17.0843707274607,1.41249077309344,2.29487517146996));
#83838=CARTESIAN_POINT('Ctrl Pts',(-17.1086732255476,1.37594662036801,2.29756940987837));
#83839=CARTESIAN_POINT('Ctrl Pts',(-17.1825020268267,1.25837449706739,2.30599320188743));
#83840=CARTESIAN_POINT('Ctrl Pts',(-17.2284082296537,1.17516840427878,2.31159607240119));
#83841=CARTESIAN_POINT('Ctrl Pts',(-17.3035351786815,1.01868229294143,2.321691433626));
#83842=CARTESIAN_POINT('Ctrl Pts',(-17.3342056011023,0.946286943855907,
2.32620193476533));
#83843=CARTESIAN_POINT('Ctrl Pts',(-17.3614291132577,0.872616062801249,
2.3307189689843));
#83844=CARTESIAN_POINT('Origin',(-15.,0.,3.));
#83845=CARTESIAN_POINT('',(-17.3614291865442,0.872615864477069,3.32953388487208));
#83846=CARTESIAN_POINT('',(-17.3591485432458,0.871797030805385,3.05636277808387));
#83847=CARTESIAN_POINT('',(-17.3614291890287,0.872615857753799,3.));
#83848=CARTESIAN_POINT('',(-17.5150210530422,0.00159552408394636,2.11258330249198));
#83849=CARTESIAN_POINT('Ctrl Pts',(-17.3591485432458,0.871797030805393,
3.05636277808387));
#83850=CARTESIAN_POINT('Ctrl Pts',(-17.2624742437046,1.13962407251414,3.03840125408691));
#83851=CARTESIAN_POINT('Ctrl Pts',(-16.7111054856786,2.12729618132246,2.96776467384271));
#83852=CARTESIAN_POINT('Ctrl Pts',(-14.6622990804118,2.95164362565941,2.84445303735124));
#83853=CARTESIAN_POINT('Ctrl Pts',(-12.3431875092431,1.32950737222075,2.6864278686095));
#83854=CARTESIAN_POINT('Ctrl Pts',(-12.435070079852,-1.49912548760771,2.52840269986778));
#83855=CARTESIAN_POINT('Ctrl Pts',(-14.8545655401893,-2.96733705322818,
2.37037753112603));
#83856=CARTESIAN_POINT('Ctrl Pts',(-17.0925050104093,-1.89324215569749,
2.2317710653341));
#83857=CARTESIAN_POINT('Ctrl Pts',(-17.5114957050982,-0.525856969687278,
2.14583965578942));
#83858=CARTESIAN_POINT('Ctrl Pts',(-17.514587964214,0.00159524933330165,
2.11258330249198));
#83859=CARTESIAN_POINT('Ctrl Pts',(-17.5174994934027,0.00159709640131535,
2.11258330249198));
#83860=CARTESIAN_POINT('Ctrl Pts',(-17.5174399084259,0.0955207624432348,
2.10666815241494));
#83861=CARTESIAN_POINT('Ctrl Pts',(-17.5121200573974,0.189246299150487,
2.1007530023379));
#83862=CARTESIAN_POINT('Ctrl Pts',(-17.5016305128836,0.282225135325527,
2.09483785226086));
#83863=CARTESIAN_POINT('Ctrl Pts',(-17.4910921020488,0.375637120304911,
2.08889514601847));
#83864=CARTESIAN_POINT('Ctrl Pts',(-17.4753358468603,0.468295220825688,
2.08295243977609));
#83865=CARTESIAN_POINT('Ctrl Pts',(-17.4545031557752,0.559661065547269,
2.0770097335337));
#83866=CARTESIAN_POINT('Ctrl Pts',(-17.4335578999204,0.651520585100958,
2.07103491721215));
#83867=CARTESIAN_POINT('Ctrl Pts',(-17.4074813199554,0.742073642382098,
2.0650601008906));
#83868=CARTESIAN_POINT('Ctrl Pts',(-17.3764652582008,0.830794274513616,
2.05908528456905));
#83869=CARTESIAN_POINT('Ctrl Pts',(-17.3715756163645,0.844780966894033,
2.05814336253907));
#83870=CARTESIAN_POINT('Ctrl Pts',(-17.36656330763,0.858722163962524,2.05720144050908));
#83871=CARTESIAN_POINT('Ctrl Pts',(-17.3614291890287,0.872615857753798,
2.0562595184791));
#83872=CARTESIAN_POINT('Ctrl Pts',(-17.3614291132577,0.872616062801249,
2.3307189689843));
#83873=CARTESIAN_POINT('Ctrl Pts',(-17.3869176511553,0.803640280654235,
2.33494812932253));
#83874=CARTESIAN_POINT('Ctrl Pts',(-17.4093845944515,0.733546376936331,
2.33918337490291));
#83875=CARTESIAN_POINT('Ctrl Pts',(-17.4475770545046,0.593537990326144,
2.34768363991974));
#83876=CARTESIAN_POINT('Ctrl Pts',(-17.4634478885576,0.523778120690173,
2.35193855498513));
#83877=CARTESIAN_POINT('Ctrl Pts',(-17.4811557921531,0.42707253811359,2.35797832605816));
#83878=CARTESIAN_POINT('Ctrl Pts',(-17.485562893351,0.400626985064299,2.35964437732084));
#83879=CARTESIAN_POINT('Ctrl Pts',(-17.4925832577244,0.353910301453609,
2.36262075381162));
#83880=CARTESIAN_POINT('Ctrl Pts',(-17.4953734322925,0.333669219728799,
2.36392175561438));
#83881=CARTESIAN_POINT('Ctrl Pts',(-17.5014365699172,0.285343125753982,
2.36705506296288));
#83882=CARTESIAN_POINT('Ctrl Pts',(-17.5044831872879,0.257234160904541,
2.36889855783631));
#83883=CARTESIAN_POINT('Ctrl Pts',(-17.5139636711795,0.153480180741025,
2.37576605195838));
#83884=CARTESIAN_POINT('Ctrl Pts',(-17.5174479275044,0.0776112731086758,
2.38090973185285));
#83885=CARTESIAN_POINT('Ctrl Pts',(-17.5176287541216,-0.188935286467546,
2.39917147469878));
#83886=CARTESIAN_POINT('Ctrl Pts',(-17.4961013173271,-0.379005005466573,
2.4124777376111));
#83887=CARTESIAN_POINT('Ctrl Pts',(-17.4383781101692,-0.629724805593542,
2.42965284337106));
#83888=CARTESIAN_POINT('Ctrl Pts',(-17.4208666769519,-0.694007916179942,
2.43402885887995));
#83889=CARTESIAN_POINT('Ctrl Pts',(-17.3891540940823,-0.79451452594344,
2.44082725258749));
#83890=CARTESIAN_POINT('Ctrl Pts',(-17.3766294435179,-0.831230039400335,
2.44330154751165));
#83891=CARTESIAN_POINT('Ctrl Pts',(-17.3506779834146,-0.90191585483675,
2.44805130092728));
#83892=CARTESIAN_POINT('Ctrl Pts',(-17.3373506479433,-0.935912047144666,
2.4503293330029));
#83893=CARTESIAN_POINT('Ctrl Pts',(-17.3030431418918,-1.01811664327379,
2.45582941542707));
#83894=CARTESIAN_POINT('Ctrl Pts',(-17.2812830733585,-1.06598186561352,
2.45902460782333));
#83895=CARTESIAN_POINT('Ctrl Pts',(-17.2302624345133,-1.16947943238262,
2.46594597607649));
#83896=CARTESIAN_POINT('Ctrl Pts',(-17.2003853960593,-1.22476835188526,
2.46965145327467));
#83897=CARTESIAN_POINT('Ctrl Pts',(-17.0884854260482,-1.41450535764004,
2.48250615460954));
#83898=CARTESIAN_POINT('Ctrl Pts',(-16.9959582236296,-1.54231808056167,
2.49139888008759));
#83899=CARTESIAN_POINT('Ctrl Pts',(-16.8430807155802,-1.71650301940684,
2.50494194940342));
#83900=CARTESIAN_POINT('Ctrl Pts',(-16.7916135705348,-1.77015480798999,
2.50935076384188));
#83901=CARTESIAN_POINT('Ctrl Pts',(-16.7196785540355,-1.83878845814315,
2.51544589712765));
#83902=CARTESIAN_POINT('Ctrl Pts',(-16.7012452905341,-1.8558560483638,2.51700234238244));
#83903=CARTESIAN_POINT('Ctrl Pts',(-16.6672745382308,-1.88637858348403,
2.51986776946221));
#83904=CARTESIAN_POINT('Ctrl Pts',(-16.6518225725973,-1.89992386613791,
2.52117035535816));
#83905=CARTESIAN_POINT('Ctrl Pts',(-16.6167841688128,-1.92988814335971,
2.52412462446931));
#83906=CARTESIAN_POINT('Ctrl Pts',(-16.5971119346455,-1.94619953681524,
2.52578285106987));
#83907=CARTESIAN_POINT('Ctrl Pts',(-16.5296616708102,-2.00041513491911,
2.53145715195341));
#83908=CARTESIAN_POINT('Ctrl Pts',(-16.4807585070886,-2.03687962349371,
2.5355520773628));
#83909=CARTESIAN_POINT('Ctrl Pts',(-16.341054817694,-2.13335802089972,2.54709805472074));
#83910=CARTESIAN_POINT('Ctrl Pts',(-16.2476137687162,-2.18931573646796,
2.55464623928563));
#83911=CARTESIAN_POINT('Ctrl Pts',(-16.031226118663,-2.30053662382151,2.57141026218501));
#83912=CARTESIAN_POINT('Ctrl Pts',(-15.9068558602498,-2.3523428817155,2.58056541460202));
#83913=CARTESIAN_POINT('Ctrl Pts',(-15.7306682603886,-2.40966919262813,
2.59274881752035));
#83914=CARTESIAN_POINT('Ctrl Pts',(-15.6819430288102,-2.42390924611142,
2.59604138677518));
#83915=CARTESIAN_POINT('Ctrl Pts',(-15.5977273827775,-2.44578057055992,
2.60160552763582));
#83916=CARTESIAN_POINT('Ctrl Pts',(-15.5624430135173,-2.4541350210893,2.60389947277222));
#83917=CARTESIAN_POINT('Ctrl Pts',(-15.4884699675048,-2.46997065715485,
2.60863583515606));
#83918=CARTESIAN_POINT('Ctrl Pts',(-15.4497612082208,-2.47731166420063,
2.61107325210743));
#83919=CARTESIAN_POINT('Ctrl Pts',(-15.341511634753,-2.49521978280486,2.61778781615758));
#83920=CARTESIAN_POINT('Ctrl Pts',(-15.2716746789872,-2.50378634934609,
2.62200294065662));
#83921=CARTESIAN_POINT('Ctrl Pts',(-15.1036660455121,-2.51728143140701,
2.63195348661318));
#83922=CARTESIAN_POINT('Ctrl Pts',(-15.0053862713122,-2.51940963883767,
2.63761846333319));
#83923=CARTESIAN_POINT('Ctrl Pts',(-14.7521420585386,-2.5100712673857,2.65219511752568));
#83924=CARTESIAN_POINT('Ctrl Pts',(-14.5979327152573,-2.4900245068108,2.6610443197688));
#83925=CARTESIAN_POINT('Ctrl Pts',(-14.4159570548383,-2.44901712298245,
2.67240531685714));
#83926=CARTESIAN_POINT('Ctrl Pts',(-14.385476799177,-2.44154706182681,2.67434067751713));
#83927=CARTESIAN_POINT('Ctrl Pts',(-14.3351271545209,-2.42820494099491,
2.67760374666496));
#83928=CARTESIAN_POINT('Ctrl Pts',(-14.3151767245409,-2.42265395595961,
2.67891433348294));
#83929=CARTESIAN_POINT('Ctrl Pts',(-14.2715416262838,-2.40993088612659,
2.6818227040949));
#83930=CARTESIAN_POINT('Ctrl Pts',(-14.2478920542708,-2.40265519806397,
2.68342557336208));
#83931=CARTESIAN_POINT('Ctrl Pts',(-14.1718478476851,-2.37802783629761,
2.6886572462396));
#83932=CARTESIAN_POINT('Ctrl Pts',(-14.1199182211979,-2.35930233665988,
2.69234993039285));
#83933=CARTESIAN_POINT('Ctrl Pts',(-13.9842510961954,-2.3052793935945,2.70224648429402));
#83934=CARTESIAN_POINT('Ctrl Pts',(-13.9017362945269,-2.26712913761037,
2.70852228853673));
#83935=CARTESIAN_POINT('Ctrl Pts',(-13.6793151093378,-2.14929667704887,
2.72589983870378));
#83936=CARTESIAN_POINT('Ctrl Pts',(-13.5446892707445,-2.06052645496528,
2.73692813818312));
#83937=CARTESIAN_POINT('Ctrl Pts',(-13.380064154688,-1.9277380070008,2.7508334931422));
#83938=CARTESIAN_POINT('Ctrl Pts',(-13.3416488487547,-1.89479234315044,
2.7541154614739));
#83939=CARTESIAN_POINT('Ctrl Pts',(-13.2774696440001,-1.83630288694201,
2.75966768746456));
#83940=CARTESIAN_POINT('Ctrl Pts',(-13.2512180440227,-1.81132023996692,
2.76196006325521));
#83941=CARTESIAN_POINT('Ctrl Pts',(-13.1975302524656,-1.75797193951023,
2.76669825813417));
#83942=CARTESIAN_POINT('Ctrl Pts',(-13.1702030867015,-1.72951035200085,
2.76913896422233));
#83943=CARTESIAN_POINT('Ctrl Pts',(-13.0958090604157,-1.64829002239326,
2.77587837790422));
#83944=CARTESIAN_POINT('Ctrl Pts',(-13.0502772942259,-1.5941724413033,2.78011423432863));
#83945=CARTESIAN_POINT('Ctrl Pts',(-12.9465514001448,-1.45978387913291,
2.79013376201575));
#83946=CARTESIAN_POINT('Ctrl Pts',(-12.8907015728942,-1.37785404332529,
2.79584546032297));
#83947=CARTESIAN_POINT('Ctrl Pts',(-12.7610826846142,-1.16127742400947,
2.81036259986223));
#83948=CARTESIAN_POINT('Ctrl Pts',(-12.6945349330085,-1.02280790805782,
2.81911120884958));
#83949=CARTESIAN_POINT('Ctrl Pts',(-12.6299729532501,-0.849573634692896,
2.8303670547454));
#83950=CARTESIAN_POINT('Ctrl Pts',(-12.6195028212696,-0.819778342378454,
2.83231412650748));
#83951=CARTESIAN_POINT('Ctrl Pts',(-12.6030913109298,-0.770107097637757,
2.83559060136096));
#83952=CARTESIAN_POINT('Ctrl Pts',(-12.596830275966,-0.750340893720218,
2.83690254208553));
#83953=CARTESIAN_POINT('Ctrl Pts',(-12.5836631794991,-0.706915754798818,
2.83980559072895));
#83954=CARTESIAN_POINT('Ctrl Pts',(-12.5768596178438,-0.683230626323396,
2.84140160002731));
#83955=CARTESIAN_POINT('Ctrl Pts',(-12.5561247863127,-0.606837882382302,
2.84658127016461));
#83956=CARTESIAN_POINT('Ctrl Pts',(-12.5435582261136,-0.553779008773233,
2.8502271556168));
#83957=CARTESIAN_POINT('Ctrl Pts',(-12.5150477716154,-0.413193494008731,
2.85994458156858));
#83958=CARTESIAN_POINT('Ctrl Pts',(-12.5020031031935,-0.325156460661742,
2.86608542144575));
#83959=CARTESIAN_POINT('Ctrl Pts',(-12.4781983189133,-0.0730060907433333,
2.88357178997894));
#83960=CARTESIAN_POINT('Ctrl Pts',(-12.4788076964045,0.0917477238429772,
2.89484652088946));
#83961=CARTESIAN_POINT('Ctrl Pts',(-12.5005808669617,0.305358351967433,
2.90895873790014));
#83962=CARTESIAN_POINT('Ctrl Pts',(-12.5071857424341,0.355270871363622,
2.91222298124398));
#83963=CARTESIAN_POINT('Ctrl Pts',(-12.5211060233838,0.440682757340842,
2.9177553079748));
#83964=CARTESIAN_POINT('Ctrl Pts',(-12.5276990472702,0.476282331932242,
2.92004508361057));
#83965=CARTESIAN_POINT('Ctrl Pts',(-12.5430969509735,0.550452351395346,
2.92478650809586));
#83966=CARTESIAN_POINT('Ctrl Pts',(-12.5520477533316,0.588982558360689,
2.92723285236229));
#83967=CARTESIAN_POINT('Ctrl Pts',(-12.5796722141068,0.696351346534435,
2.93401499948102));
#83968=CARTESIAN_POINT('Ctrl Pts',(-12.6003687714435,0.764632627008571,
2.93828651460151));
#83969=CARTESIAN_POINT('Ctrl Pts',(-12.6571642681183,0.926841873644022,
2.94842560670099));
#83970=CARTESIAN_POINT('Ctrl Pts',(-12.6960464175674,1.01966392427488,2.95421851629432));
#83971=CARTESIAN_POINT('Ctrl Pts',(-12.806563482134,1.24466043223553,2.96863469749068));
#83972=CARTESIAN_POINT('Ctrl Pts',(-12.8846626119122,1.37320096601879,2.97721004938609));
#83973=CARTESIAN_POINT('Ctrl Pts',(-12.9926754001392,1.51969505002037,2.98828525906537));
#83974=CARTESIAN_POINT('Ctrl Pts',(-13.0121037247994,1.54502209456754,2.99025227605026));
#83975=CARTESIAN_POINT('Ctrl Pts',(-13.0449666736673,1.58621650140448,2.99355169319552));
#83976=CARTESIAN_POINT('Ctrl Pts',(-13.0581255019231,1.60229881892036,2.99486604922211));
#83977=CARTESIAN_POINT('Ctrl Pts',(-13.0872170304606,1.63696876509306,2.99776057623168));
#83978=CARTESIAN_POINT('Ctrl Pts',(-13.1032231558638,1.65548872478016,2.99934534512335));
#83979=CARTESIAN_POINT('Ctrl Pts',(-13.1550175808511,1.71368043431677,3.00444101542798));
#83980=CARTESIAN_POINT('Ctrl Pts',(-13.1917980664131,1.75244562621497,3.00801151178949));
#83981=CARTESIAN_POINT('Ctrl Pts',(-13.2908870688405,1.85043915937773,3.01744525799798));
#83982=CARTESIAN_POINT('Ctrl Pts',(-13.3550451955013,1.90769876580335,3.0233736901728));
#83983=CARTESIAN_POINT('Ctrl Pts',(-13.5545629362486,2.06820265521756,3.04105265507564));
#83984=CARTESIAN_POINT('Ctrl Pts',(-13.6976113851656,2.16114567730894,3.05273857469013));
#83985=CARTESIAN_POINT('Ctrl Pts',(-13.893258716429,2.2617274372317,3.06718804843629));
#83986=CARTESIAN_POINT('Ctrl Pts',(-13.9382258410366,2.28318275130165,3.07041658358145));
#83987=CARTESIAN_POINT('Ctrl Pts',(-14.0168604523089,2.31787584077405,3.07590891744927));
#83988=CARTESIAN_POINT('Ctrl Pts',(-14.0502296614099,2.33174790806057,3.07819355462035));
#83989=CARTESIAN_POINT('Ctrl Pts',(-14.1209204821693,2.35936564147681,3.08294215743068));
#83990=CARTESIAN_POINT('Ctrl Pts',(-14.1582926148763,2.37295511612319,3.08540041986946));
#83991=CARTESIAN_POINT('Ctrl Pts',(-14.2648110442874,2.4088545878647,3.09227349976952));
#83992=CARTESIAN_POINT('Ctrl Pts',(-14.3346250801505,2.42906582920409,3.09662092320177));
#83993=CARTESIAN_POINT('Ctrl Pts',(-14.5060424418368,2.47074445920202,3.10701856413908));
#83994=CARTESIAN_POINT('Ctrl Pts',(-14.6082871056264,2.48900276700779,3.11298808776827));
#83995=CARTESIAN_POINT('Ctrl Pts',(-14.8538657903651,2.51734516716821,3.12720309371405));
#83996=CARTESIAN_POINT('Ctrl Pts',(-14.9974916362546,2.52158018074536,3.13541620335771));
#83997=CARTESIAN_POINT('Ctrl Pts',(-15.1731847622204,2.51174705460864,3.14611277298168));
#83998=CARTESIAN_POINT('Ctrl Pts',(-15.2056510780705,2.50929743751347,3.14811730249084));
#83999=CARTESIAN_POINT('Ctrl Pts',(-15.2586326898,2.50426485818008,3.15144737695365));
#84000=CARTESIAN_POINT('Ctrl Pts',(-15.2791808960018,2.50205742394284,3.15275358573873));
#84001=CARTESIAN_POINT('Ctrl Pts',(-15.3236139009028,2.49672994168545,3.15561346334708));
#84002=CARTESIAN_POINT('Ctrl Pts',(-15.3474845935808,2.49351974291422,3.15717141546744));
#84003=CARTESIAN_POINT('Ctrl Pts',(-15.4216621063144,2.48245837924733,3.16207232464232));
#84004=CARTESIAN_POINT('Ctrl Pts',(-15.4717768600345,2.47342361427633,3.1654689918391));
#84005=CARTESIAN_POINT('Ctrl Pts',(-15.5991938543346,2.44643968908259,3.17427004021474));
#84006=CARTESIAN_POINT('Ctrl Pts',(-15.675984552029,2.42634378855768,3.17973070112641));
#84007=CARTESIAN_POINT('Ctrl Pts',(-15.9276072548158,2.34762120089638,3.19792656820457));
#84008=CARTESIAN_POINT('Ctrl Pts',(-16.0969729444548,2.2734228541718,3.21062117286218));
#84009=CARTESIAN_POINT('Ctrl Pts',(-16.2984913392214,2.15732449941014,3.22586609457039));
#84010=CARTESIAN_POINT('Ctrl Pts',(-16.3395521488667,2.13207160133538,3.22898437688953));
#84011=CARTESIAN_POINT('Ctrl Pts',(-16.409928326851,2.0859530884859,3.23435421242933));
#84012=CARTESIAN_POINT('Ctrl Pts',(-16.4395673938858,2.065609863513,3.23662399936454));
#84013=CARTESIAN_POINT('Ctrl Pts',(-16.5016550814389,2.0210092879739,3.24140132552338));
#84014=CARTESIAN_POINT('Ctrl Pts',(-16.5339745908237,1.99658928449236,3.24390180703324));
#84015=CARTESIAN_POINT('Ctrl Pts',(-16.6263707956021,1.92320787851969,3.25110496930146));
#84016=CARTESIAN_POINT('Ctrl Pts',(-16.6847953962513,1.87223838778244,3.25572839910409));
#84017=CARTESIAN_POINT('Ctrl Pts',(-16.8248440830177,1.73818632373008,3.26711846813765));
#84018=CARTESIAN_POINT('Ctrl Pts',(-16.9032306394381,1.65198732895874,3.27377864117047));
#84019=CARTESIAN_POINT('Ctrl Pts',(-17.0504374048973,1.46566502219285,3.2874442656608));
#84020=CARTESIAN_POINT('Ctrl Pts',(-17.1185413576125,1.36537328062916,3.29443675963154));
#84021=CARTESIAN_POINT('Ctrl Pts',(-17.1959856569462,1.23149602238749,3.30382291363717));
#84022=CARTESIAN_POINT('Ctrl Pts',(-17.2122269693059,1.2020761383984,3.30588892962065));
#84023=CARTESIAN_POINT('Ctrl Pts',(-17.2375711821288,1.15391295818733,3.30929100820269));
#84024=CARTESIAN_POINT('Ctrl Pts',(-17.2470393750153,1.13536511017195,3.31060591107133));
#84025=CARTESIAN_POINT('Ctrl Pts',(-17.2667746720633,1.09549029391578,3.31344669567697));
#84026=CARTESIAN_POINT('Ctrl Pts',(-17.2769728588546,1.07413262464057,3.31497607552966));
#84027=CARTESIAN_POINT('Ctrl Pts',(-17.3070868092074,1.0087095630365,3.31967743761322));
#84028=CARTESIAN_POINT('Ctrl Pts',(-17.3260344989279,0.964213345029977,
3.32289740531873));
#84029=CARTESIAN_POINT('Ctrl Pts',(-17.3497558351271,0.903731126947436,
3.32727908574531));
#84030=CARTESIAN_POINT('Ctrl Pts',(-17.3556698601044,0.888201464170371,
3.32840458537843));
#84031=CARTESIAN_POINT('Ctrl Pts',(-17.3614291865442,0.872615864477068,
3.32953388487208));
#84032=CARTESIAN_POINT('Origin',(-15.,0.,3.));
#84033=CARTESIAN_POINT('',(-17.3578782887762,0.871321062777569,4.33113094084205));
#84034=CARTESIAN_POINT('',(-17.3614291890287,0.872615857753799,4.05617654298853));
#84035=CARTESIAN_POINT('',(-17.3614291890287,0.872615857753799,3.));
#84036=CARTESIAN_POINT('',(-17.5174991368084,-0.00208474675815134,3.11258330249198));
#84037=CARTESIAN_POINT('Ctrl Pts',(-17.3614291890287,0.872615857753799,
4.05617654298853));
#84038=CARTESIAN_POINT('Ctrl Pts',(-17.3326458200154,0.950507964736045,
4.05093731159241));
#84039=CARTESIAN_POINT('Ctrl Pts',(-17.2999869751406,1.02702172058073,4.04569808019629));
#84040=CARTESIAN_POINT('Ctrl Pts',(-17.2636144934765,1.10175118557831,4.04045884880017));
#84041=CARTESIAN_POINT('Ctrl Pts',(-17.2272502797581,1.17646366358085,4.03522080835059));
#84042=CARTESIAN_POINT('Ctrl Pts',(-17.1871743080278,1.249392242068,4.02998276790101));
#84043=CARTESIAN_POINT('Ctrl Pts',(-17.1435956684316,1.32015296851596,4.02474472745143));
#84044=CARTESIAN_POINT('Ctrl Pts',(-17.1000138112337,1.3909189195379,4.01950630025441));
#84045=CARTESIAN_POINT('Ctrl Pts',(-17.0529290156622,1.45951630881581,4.01426787305739));
#84046=CARTESIAN_POINT('Ctrl Pts',(-17.0025945105235,1.52558889495866,4.00902944586036));
#84047=CARTESIAN_POINT('Ctrl Pts',(-16.9522080313203,1.5917297058877,4.00378560960345));
#84048=CARTESIAN_POINT('Ctrl Pts',(-16.8985654223714,1.65534014057156,3.99854177334654));
#84049=CARTESIAN_POINT('Ctrl Pts',(-16.8419608225546,1.71609631960855,3.99329793708963));
#84050=CARTESIAN_POINT('Ctrl Pts',(-16.7853255760493,1.7768853930693,3.988051261731));
#84051=CARTESIAN_POINT('Ctrl Pts',(-16.7257254759839,1.83481681200538,3.98280458637238));
#84052=CARTESIAN_POINT('Ctrl Pts',(-16.6634904713541,1.88960464164179,3.97755791101376));
#84053=CARTESIAN_POINT('Ctrl Pts',(-16.6011493175152,1.94448591844372,3.97230228682573));
#84054=CARTESIAN_POINT('Ctrl Pts',(-16.5361646442827,1.99621260983414,3.9670466626377));
#84055=CARTESIAN_POINT('Ctrl Pts',(-16.468898079244,2.04454021305361,3.96179103844968));
#84056=CARTESIAN_POINT('Ctrl Pts',(-16.4212781545174,2.07875270519151,3.95807043181425));
#84057=CARTESIAN_POINT('Ctrl Pts',(-16.3725152707675,2.11126259752159,3.95434982517882));
#84058=CARTESIAN_POINT('Ctrl Pts',(-16.322745146686,2.14199708844773,3.9506292185434));
#84059=CARTESIAN_POINT('Ctrl Pts',(-16.2524270553321,2.1854205433928,3.94537253168335));
#84060=CARTESIAN_POINT('Ctrl Pts',(-16.1798394464329,2.22545734520791,3.9401158448233));
#84061=CARTESIAN_POINT('Ctrl Pts',(-16.1053419672033,2.26186325526968,3.93485915796325));
#84062=CARTESIAN_POINT('Ctrl Pts',(-16.030949644946,2.29821777654194,3.92960989118346));
#84063=CARTESIAN_POINT('Ctrl Pts',(-15.9546532181557,2.3309513856163,3.92436062440367));
#84064=CARTESIAN_POINT('Ctrl Pts',(-15.8768397418617,2.35986404631538,3.91911135762388));
#84065=CARTESIAN_POINT('Ctrl Pts',(-15.7987020560729,2.3888971714836,3.91384021979795));
#84066=CARTESIAN_POINT('Ctrl Pts',(-15.7190350506276,2.41407718762873,3.90856908197203));
#84067=CARTESIAN_POINT('Ctrl Pts',(-15.6382540307266,2.43524907191465,3.9032979441461));
#84068=CARTESIAN_POINT('Ctrl Pts',(-15.5579508403316,2.45629572194359,3.89805798573813));
#84069=CARTESIAN_POINT('Ctrl Pts',(-15.4765472288899,2.47338140804105,3.89281802733017));
#84070=CARTESIAN_POINT('Ctrl Pts',(-15.3944678088657,2.48640330553366,3.8875780689222));
#84071=CARTESIAN_POINT('Ctrl Pts',(-15.3124151379961,2.49942095927368,3.88233981818296));
#84072=CARTESIAN_POINT('Ctrl Pts',(-15.2296875510342,2.5083773825551,3.87710156744371));
#84073=CARTESIAN_POINT('Ctrl Pts',(-15.146719160104,2.51322098870321,3.87186331670446));
#84074=CARTESIAN_POINT('Ctrl Pts',(-15.0637528219605,2.51806447501184,3.86662519556892));
#84075=CARTESIAN_POINT('Ctrl Pts',(-14.9805461520855,2.51879532071795,3.86138707443338));
#84076=CARTESIAN_POINT('Ctrl Pts',(-14.8975362952314,2.51541396974834,3.85614895329784));
#84077=CARTESIAN_POINT('Ctrl Pts',(-14.813618588759,2.51199563813205,3.85085354467316));
#84078=CARTESIAN_POINT('Ctrl Pts',(-14.7299025079231,2.50437461424801,3.84555813604848));
#84079=CARTESIAN_POINT('Ctrl Pts',(-14.6468356846868,2.4926053069809,3.8402627274238));
#84080=CARTESIAN_POINT('Ctrl Pts',(-14.5645499434984,2.48094666717722,3.8350171118266));
#84081=CARTESIAN_POINT('Ctrl Pts',(-14.4829017474058,2.4652175785989,3.82977149622941));
#84082=CARTESIAN_POINT('Ctrl Pts',(-14.4023154018894,2.44552231050575,3.82452588063222));
#84083=CARTESIAN_POINT('Ctrl Pts',(-14.3205816300957,2.42554661192524,3.81920557549379));
#84084=CARTESIAN_POINT('Ctrl Pts',(-14.2399406560968,2.40149104198238,3.81388527035537));
#84085=CARTESIAN_POINT('Ctrl Pts',(-14.1608168632588,2.37351593906786,3.80856496521694));
#84086=CARTESIAN_POINT('Ctrl Pts',(-14.0816930704208,2.34554083615334,3.80324466007851));
#84087=CARTESIAN_POINT('Ctrl Pts',(-14.0040868857404,2.31364644493991,3.79792435494008));
#84088=CARTESIAN_POINT('Ctrl Pts',(-13.9283976203273,2.27804183233754,3.79260404980165));
#84089=CARTESIAN_POINT('Ctrl Pts',(-13.8536134524737,2.24286298219697,3.78734736524628));
#84090=CARTESIAN_POINT('Ctrl Pts',(-13.7804262398426,2.20393315497003,3.78209068069091));
#84091=CARTESIAN_POINT('Ctrl Pts',(-13.709237021646,2.16142017750155,3.77683399613554));
#84092=CARTESIAN_POINT('Ctrl Pts',(-13.6381482914769,2.11896720975581,3.77158473171871));
#84093=CARTESIAN_POINT('Ctrl Pts',(-13.5690523463221,2.07294137281064,3.76633546730188));
#84094=CARTESIAN_POINT('Ctrl Pts',(-13.5023281726944,2.02355759683165,3.76108620288505));
#84095=CARTESIAN_POINT('Ctrl Pts',(-13.4353259555236,1.97396803576314,3.75581506447567));
#84096=CARTESIAN_POINT('Ctrl Pts',(-13.370715748042,1.92099268608187,3.75054392606629));
#84097=CARTESIAN_POINT('Ctrl Pts',(-13.308854265586,1.86489473026583,3.74527278765691));
#84098=CARTESIAN_POINT('Ctrl Pts',(-13.2473587372881,1.80912863329598,3.7400328317369));
#84099=CARTESIAN_POINT('Ctrl Pts',(-13.1885798478623,1.75027708590773,3.73479287581688));
#84100=CARTESIAN_POINT('Ctrl Pts',(-13.1328356743309,1.68863957994255,3.72955291989687));
#84101=CARTESIAN_POINT('Ctrl Pts',(-13.0771096679175,1.6270221617422,3.72431467168713));
#84102=CARTESIAN_POINT('Ctrl Pts',(-13.0244167221458,1.56262092998962,3.71907642347739));
#84103=CARTESIAN_POINT('Ctrl Pts',(-12.9750371856855,1.49577132297807,3.71383817526764));
#84104=CARTESIAN_POINT('Ctrl Pts',(-12.9256588713244,1.42892337043423,3.70860005669984));
#84105=CARTESIAN_POINT('Ctrl Pts',(-12.8795940763273,1.35962753465171,3.70336193813203));
#84106=CARTESIAN_POINT('Ctrl Pts',(-12.8370812244144,1.28825021646396,3.69812381956423));
#84107=CARTESIAN_POINT('Ctrl Pts',(-12.7941033796426,1.2160921945182,3.6928284080222));
#84108=CARTESIAN_POINT('Ctrl Pts',(-12.7547559148056,1.14180728256877,3.68753299648018));
#84109=CARTESIAN_POINT('Ctrl Pts',(-12.719237781177,1.06580014598871,3.68223758493815));
#84110=CARTESIAN_POINT('Ctrl Pts',(-12.6840536636373,0.990507788139913,
3.67699197197707));
#84111=CARTESIAN_POINT('Ctrl Pts',(-12.6526272758111,0.913525916800646,
3.671746359016));
#84112=CARTESIAN_POINT('Ctrl Pts',(-12.6251030621893,0.835266894338282,
3.66650074605492));
#84113=CARTESIAN_POINT('Ctrl Pts',(-12.5971869019666,0.755893458281015,
3.66118043522242));
#84114=CARTESIAN_POINT('Ctrl Pts',(-12.5732850637082,0.67520668328761,3.65586012438992));
#84115=CARTESIAN_POINT('Ctrl Pts',(-12.5534950705602,0.59364962749637,3.65053981355742));
#84116=CARTESIAN_POINT('Ctrl Pts',(-12.5337050774122,0.512092571705129,
3.64521950272493));
#84117=CARTESIAN_POINT('Ctrl Pts',(-12.5180269576855,0.429665726434531,
3.63989919189243));
#84118=CARTESIAN_POINT('Ctrl Pts',(-12.5065037224533,0.346817767509945,
3.63457888105993));
#84119=CARTESIAN_POINT('Ctrl Pts',(-12.4951182891101,0.264960555109053,
3.62932219375577));
#84120=CARTESIAN_POINT('Ctrl Pts',(-12.4877470890919,0.18239196057308,3.6240655064516));
#84121=CARTESIAN_POINT('Ctrl Pts',(-12.4844686202709,0.0995395780488252,
3.61880881914744));
#84122=CARTESIAN_POINT('Ctrl Pts',(-12.4811947791833,0.0168041460788885,
3.61355955193761));
#84123=CARTESIAN_POINT('Ctrl Pts',(-12.4820022120968,-0.0662138212331839,
3.60831028472778));
#84124=CARTESIAN_POINT('Ctrl Pts',(-12.4869179159025,-0.149079470713462,
3.60306101751796));
#84125=CARTESIAN_POINT('Ctrl Pts',(-12.491854100459,-0.232290371003117,
3.5977898798013));
#84126=CARTESIAN_POINT('Ctrl Pts',(-12.5009329329858,-0.315347215037223,
3.59251874208464));
#84127=CARTESIAN_POINT('Ctrl Pts',(-12.5141288277071,-0.397807446842296,
3.58724760436798));
#84128=CARTESIAN_POINT('Ctrl Pts',(-12.5272466683683,-0.479779924233319,
3.5820076455679));
#84129=CARTESIAN_POINT('Ctrl Pts',(-12.5444329271818,-0.561162367680381,
3.57676768676782));
#84130=CARTESIAN_POINT('Ctrl Pts',(-12.5656104984621,-0.64152474995281,
3.57152772796774));
#84131=CARTESIAN_POINT('Ctrl Pts',(-12.5867811680472,-0.721860942410311,
3.56628947685162));
#84132=CARTESIAN_POINT('Ctrl Pts',(-12.6119404492328,-0.801177288403083,
3.5610512257355));
#84133=CARTESIAN_POINT('Ctrl Pts',(-12.6409605175132,-0.879055726372575,
3.55581297461938));
#84134=CARTESIAN_POINT('Ctrl Pts',(-12.6699798676975,-0.956932237254603,
3.55057485312281));
#84135=CARTESIAN_POINT('Ctrl Pts',(-12.7028596530037,-1.03337047914813,
3.54533673162624));
#84136=CARTESIAN_POINT('Ctrl Pts',(-12.7394232122634,-1.10797059380949,
3.54009861012967));
#84137=CARTESIAN_POINT('Ctrl Pts',(-12.7763866484607,-1.18338657175096,
3.53480320197871));
#84138=CARTESIAN_POINT('Ctrl Pts',(-12.8171147307613,-1.25692353151196,
3.52950779382776));
#84139=CARTESIAN_POINT('Ctrl Pts',(-12.8613771856309,-1.32819377647239,
3.5242123856768));
#84140=CARTESIAN_POINT('Ctrl Pts',(-12.9052234447086,-1.39879387387489,
3.51896676976161));
#84141=CARTESIAN_POINT('Ctrl Pts',(-12.9525375723219,-1.46716935666535,
3.51372115384643));
#84142=CARTESIAN_POINT('Ctrl Pts',(-13.0030530720546,-1.53297397791662,
3.50847553793125));
#84143=CARTESIAN_POINT('Ctrl Pts',(-13.0542878237437,-1.59971554135044,
3.5031552336624));
#84144=CARTESIAN_POINT('Ctrl Pts',(-13.1088155092712,-1.66381208411523,
3.49783492939356));
#84145=CARTESIAN_POINT('Ctrl Pts',(-13.1663182913934,-1.72493989504607,
3.49251462512471));
#84146=CARTESIAN_POINT('Ctrl Pts',(-13.2238210735156,-1.78606770597692,
3.48719432085587));
#84147=CARTESIAN_POINT('Ctrl Pts',(-13.2842985561663,-1.84422649297438,
3.48187401658703));
#84148=CARTESIAN_POINT('Ctrl Pts',(-13.3473984190091,-1.89913513592538,
3.47655371231818));
#84149=CARTESIAN_POINT('Ctrl Pts',(-13.4097437609029,-1.95338720500255,
3.47129702595348));
#84150=CARTESIAN_POINT('Ctrl Pts',(-13.4748777887539,-2.00466549675405,
3.46604033958878));
#84151=CARTESIAN_POINT('Ctrl Pts',(-13.542485224122,-2.05267068184285,3.46078365322407));
#84152=CARTESIAN_POINT('Ctrl Pts',(-13.6099972278478,-2.10060810495213,
3.45553438696354));
#84153=CARTESIAN_POINT('Ctrl Pts',(-13.6799753312175,-2.14528133384807,
3.450285120703));
#84154=CARTESIAN_POINT('Ctrl Pts',(-13.7520700424885,-2.18643021181684,
3.44503585444246));
#84155=CARTESIAN_POINT('Ctrl Pts',(-13.8244651449489,-2.22775054147983,
3.43976471648971));
#84156=CARTESIAN_POINT('Ctrl Pts',(-13.8989941790308,-2.26551677425097,
3.43449357853696));
#84157=CARTESIAN_POINT('Ctrl Pts',(-13.9752724768328,-2.29950858951725,
3.42922244058421));
#84158=CARTESIAN_POINT('Ctrl Pts',(-14.0510995691444,-2.33329933456931,
3.42398248275023));
#84159=CARTESIAN_POINT('Ctrl Pts',(-14.1286548620561,-2.36336000224891,
3.41874252491625));
#84160=CARTESIAN_POINT('Ctrl Pts',(-14.2075360388061,-2.38952026988868,
3.41350256708228));
#84161=CARTESIAN_POINT('Ctrl Pts',(-14.2863915083938,-2.41567201196792,
3.4082643169364));
#84162=CARTESIAN_POINT('Ctrl Pts',(-14.3665715662811,-2.43792573358534,
3.40302606679052));
#84163=CARTESIAN_POINT('Ctrl Pts',(-14.4476562125589,-2.45616013127712,
3.39778781664463));
#84164=CARTESIAN_POINT('Ctrl Pts',(-14.5287388523686,-2.47439407775231,
3.3925496961211));
#84165=CARTESIAN_POINT('Ctrl Pts',(-14.6107255859485,-2.48860879794204,
3.38731157559756));
#84166=CARTESIAN_POINT('Ctrl Pts',(-14.6931849831347,-2.49873383845218,
3.38207345507403));
#84167=CARTESIAN_POINT('Ctrl Pts',(-14.7765462299916,-2.5089696154552,3.37677804578256));
#84168=CARTESIAN_POINT('Ctrl Pts',(-14.8603900673708,-2.51502563260598,
3.3714826364911));
#84169=CARTESIAN_POINT('Ctrl Pts',(-14.9442659649256,-2.51688298642077,
3.36618722719963));
#84170=CARTESIAN_POINT('Ctrl Pts',(-15.0273531518726,-2.51872287497201,
3.36094161225437));
#84171=CARTESIAN_POINT('Ctrl Pts',(-15.110471334073,-2.5164428059925,3.35569599730912));
#84172=CARTESIAN_POINT('Ctrl Pts',(-15.1931849133998,-2.51007685922856,
3.35045038236386));
#84173=CARTESIAN_POINT('Ctrl Pts',(-15.2770762388958,-2.50362026870968,
3.34513007589929));
#84174=CARTESIAN_POINT('Ctrl Pts',(-15.3605508609467,-2.49296059169368,
3.33980976943472));
#84175=CARTESIAN_POINT('Ctrl Pts',(-15.4431640113846,-2.47818722234893,
3.33448946297016));
#84176=CARTESIAN_POINT('Ctrl Pts',(-15.5257771618225,-2.46341385300418,
3.32916915650559));
#84177=CARTESIAN_POINT('Ctrl Pts',(-15.6075283796236,-2.44452696351927,
3.32384885004102));
#84178=CARTESIAN_POINT('Ctrl Pts',(-15.6879897347522,-2.42166809758803,
3.31852854357646));
#84179=CARTESIAN_POINT('Ctrl Pts',(-15.7674889341989,-2.3990825776339,3.31327185725707));
#84180=CARTESIAN_POINT('Ctrl Pts',(-15.846020607845,-2.37253675293294,3.30801517093768));
#84181=CARTESIAN_POINT('Ctrl Pts',(-15.9231618085221,-2.34213119301335,
3.30275848461829));
#84182=CARTESIAN_POINT('Ctrl Pts',(-16.0001941200367,-2.31176855225924,
3.29750921840859));
#84183=CARTESIAN_POINT('Ctrl Pts',(-16.0758394317685,-2.27755716600603,
3.2922599521989));
#84184=CARTESIAN_POINT('Ctrl Pts',(-16.149688918676,-2.23964765985046,3.28701068598921));
#84185=CARTESIAN_POINT('Ctrl Pts',(-16.2238461091416,-2.20158019877307,
3.28173954802444));
#84186=CARTESIAN_POINT('Ctrl Pts',(-16.2961920223794,-2.15978385801918,
3.27646841005967));
#84187=CARTESIAN_POINT('Ctrl Pts',(-16.3663319852265,-2.11446048819715,
3.2711972720949));
#84188=CARTESIAN_POINT('Ctrl Pts',(-16.4360570513818,-2.06940521826339,
3.26595731432491));
#84189=CARTESIAN_POINT('Ctrl Pts',(-16.5036018011638,-2.02086478346146,
3.26071735655493));
#84190=CARTESIAN_POINT('Ctrl Pts',(-16.5686037995229,-1.96908312930725,
3.25547739878494));
#84191=CARTESIAN_POINT('Ctrl Pts',(-16.6335846138464,-1.91731835070199,
3.25023914870787));
#84192=CARTESIAN_POINT('Ctrl Pts',(-16.6960239622171,-1.86231473778499,
3.2450008986308));
#84193=CARTESIAN_POINT('Ctrl Pts',(-16.7555908091454,-1.80435782505698,
3.23976264855373));
#84194=CARTESIAN_POINT('Ctrl Pts',(-16.8151561820169,-1.74640234654574,
3.23452452810375));
#84195=CARTESIAN_POINT('Ctrl Pts',(-16.8718488650438,-1.68549403586695,
3.22928640765377));
#84196=CARTESIAN_POINT('Ctrl Pts',(-16.925374171573,-1.62195577912576,3.2240482872038));
#84197=CARTESIAN_POINT('Ctrl Pts',(-16.9794848801979,-1.55772260943477,
3.21875287783971));
#84198=CARTESIAN_POINT('Ctrl Pts',(-17.0303581823909,-1.49080197123738,
3.21345746847561));
#84199=CARTESIAN_POINT('Ctrl Pts',(-17.0777321367213,-1.42156090901366,
3.20816205911152));
#84200=CARTESIAN_POINT('Ctrl Pts',(-17.1246606179321,-1.35297094363052,
3.20291644425081));
#84201=CARTESIAN_POINT('Ctrl Pts',(-17.1681550948794,-1.28210444033667,
3.19767082939009));
#84202=CARTESIAN_POINT('Ctrl Pts',(-17.2080061625757,-1.20934487886118,
3.19242521452938));
#84203=CARTESIAN_POINT('Ctrl Pts',(-17.248424665409,-1.13554930168715,3.1871049079136));
#84204=CARTESIAN_POINT('Ctrl Pts',(-17.2850949728687,-1.05980677511648,
3.18178460129782));
#84205=CARTESIAN_POINT('Ctrl Pts',(-17.3178490028582,-0.982538676057817,
3.17646429468204));
#84206=CARTESIAN_POINT('Ctrl Pts',(-17.3506030328476,-0.905270576999156,
3.17114398806627));
#84207=CARTESIAN_POINT('Ctrl Pts',(-17.3794406777545,-0.826477385673053,
3.16582368145049));
#84208=CARTESIAN_POINT('Ctrl Pts',(-17.4042467347159,-0.746594862430815,
3.16050337483471));
#84209=CARTESIAN_POINT('Ctrl Pts',(-17.4339138432341,-0.651058377554528,
3.15414048878773));
#84210=CARTESIAN_POINT('Ctrl Pts',(-17.4579043977056,-0.553681574447381,
3.14777760274075));
#84211=CARTESIAN_POINT('Ctrl Pts',(-17.4760270826673,-0.455078164602668,
3.14141471669378));
#84212=CARTESIAN_POINT('Ctrl Pts',(-17.4939245284781,-0.35770025464125,
3.13513091225381));
#84213=CARTESIAN_POINT('Ctrl Pts',(-17.5060990149422,-0.259126055024416,
3.12884710781385));
#84214=CARTESIAN_POINT('Ctrl Pts',(-17.5124125335096,-0.159967219966266,
3.12256330337389));
#84215=CARTESIAN_POINT('Ctrl Pts',(-17.5157549312281,-0.107472203039025,
3.11923663641326));
#84216=CARTESIAN_POINT('Ctrl Pts',(-17.517455471861,-0.0548136774819967,
3.11590996945262));
#84217=CARTESIAN_POINT('Ctrl Pts',(-17.5174991368084,-0.00208474675815134,
3.11258330249198));
#84218=CARTESIAN_POINT('Ctrl Pts',(-17.5158506929074,-0.00208338167800927,
3.11258330249198));
#84219=CARTESIAN_POINT('Ctrl Pts',(-17.5134950467056,0.294763138477447,
3.09384312768927));
#84220=CARTESIAN_POINT('Ctrl Pts',(-17.4600137745389,0.592359407396509,
3.07510295288657));
#84221=CARTESIAN_POINT('Ctrl Pts',(-17.3591485432458,0.871797030805393,
3.05636277808387));
#84222=CARTESIAN_POINT('',(-17.5137714174146,0.00044567345935998,3.38754613095039));
#84223=CARTESIAN_POINT('Ctrl Pts',(-17.3614291865442,0.872615864477068,
3.32953388487208));
#84224=CARTESIAN_POINT('Ctrl Pts',(-17.3809756275514,0.819720268412054,
3.33336658756098));
#84225=CARTESIAN_POINT('Ctrl Pts',(-17.3987401945501,0.766180343022783,
3.33724267734535));
#84226=CARTESIAN_POINT('Ctrl Pts',(-17.4666913825592,0.535757271946432,
3.35380824336746));
#84227=CARTESIAN_POINT('Ctrl Pts',(-17.4992277272465,0.354234193360712,
3.36651646510683));
#84228=CARTESIAN_POINT('Ctrl Pts',(-17.5139281816499,0.13801801640971,3.38080025921794));
#84229=CARTESIAN_POINT('Ctrl Pts',(-17.5155142151089,0.105224851673531,
3.38294571868902));
#84230=CARTESIAN_POINT('Ctrl Pts',(-17.517147176403,0.048473737035035,3.38662289728093));
#84231=CARTESIAN_POINT('Ctrl Pts',(-17.5174943818047,0.0245295727084708,
3.38816339559275));
#84232=CARTESIAN_POINT('Ctrl Pts',(-17.5174999323689,0.000583543289451465,
3.38969342428349));
#84233=CARTESIAN_POINT('Ctrl Pts',(-17.5135466719092,0.000437363012700809,
3.38741669750803));
#84234=CARTESIAN_POINT('Ctrl Pts',(-17.512848798928,-0.445064979324669,
3.41547689838276));
#84235=CARTESIAN_POINT('Ctrl Pts',(-17.1880561406799,-1.72782200703888,
3.49621215550473));
#84236=CARTESIAN_POINT('Ctrl Pts',(-15.1454344547701,-2.96733695176447,
3.62962246887397));
#84237=CARTESIAN_POINT('Ctrl Pts',(-12.593960767586,-1.74276188959023,3.78764763761569));
#84238=CARTESIAN_POINT('Ctrl Pts',(-12.2259104525059,1.06333032658794,3.94567280635744));
#84239=CARTESIAN_POINT('Ctrl Pts',(-14.3752804154246,2.90447128399857,4.10369797509916));
#84240=CARTESIAN_POINT('Ctrl Pts',(-16.5838217551577,2.25841194757869,4.23218401992738));
#84241=CARTESIAN_POINT('Ctrl Pts',(-17.231678627738,1.21621768087466,4.30799500850834));
#84242=CARTESIAN_POINT('Ctrl Pts',(-17.3578782887762,0.871321062777582,
4.33113094084205));
#84243=CARTESIAN_POINT('Origin',(-15.,0.,3.));
#84244=CARTESIAN_POINT('',(-17.3614291890287,0.872615857753799,5.33098035402157));
#84245=CARTESIAN_POINT('',(-17.3614291890287,0.872615857753801,5.05624492860065));
#84246=CARTESIAN_POINT('',(-17.3614291890287,0.872615857753799,3.));
#84247=CARTESIAN_POINT('',(-17.517499506146,0.00157688125814863,5.38741669754798));
#84248=CARTESIAN_POINT('Ctrl Pts',(-17.3614291890287,0.872615857753799,
5.33098035402157));
#84249=CARTESIAN_POINT('Ctrl Pts',(-17.3901822610416,0.794805738991659,
5.3362220473329));
#84250=CARTESIAN_POINT('Ctrl Pts',(-17.4150567487437,0.715650742612291,
5.34146374064422));
#84251=CARTESIAN_POINT('Ctrl Pts',(-17.4359499453844,0.635573845891745,
5.34670543395554));
#84252=CARTESIAN_POINT('Ctrl Pts',(-17.4568769901463,0.555367220219244,
5.35195561909669));
#84253=CARTESIAN_POINT('Ctrl Pts',(-17.4738097794136,0.474236165619432,
5.35720580423783));
#84254=CARTESIAN_POINT('Ctrl Pts',(-17.486696953703,0.392612417587985,5.36245598937898));
#84255=CARTESIAN_POINT('Ctrl Pts',(-17.4911507150723,0.364403542031883,
5.364270434597));
#84256=CARTESIAN_POINT('Ctrl Pts',(-17.4951217376959,0.336135847325646,
5.36608487981503));
#84257=CARTESIAN_POINT('Ctrl Pts',(-17.4986093480335,0.307827185154029,
5.36789932503306));
#84258=CARTESIAN_POINT('Ctrl Pts',(-17.5111143622989,0.206324955825689,
5.37440511585805));
#84259=CARTESIAN_POINT('Ctrl Pts',(-17.5174353191478,0.104051732231825,
5.38091090668304));
#84260=CARTESIAN_POINT('Ctrl Pts',(-17.5174995061456,0.00157688188738101,
5.38741669750803));
#84261=CARTESIAN_POINT('',(-13.0865340033349,1.63598720337492,6.));
#84262=CARTESIAN_POINT('Ctrl Pts',(-17.517499506146,0.00157688125815036,
5.38741669754798));
#84263=CARTESIAN_POINT('Ctrl Pts',(-17.5175506917775,-0.0801412578474424,
5.39260471312289));
#84264=CARTESIAN_POINT('Ctrl Pts',(-17.5136187948921,-0.162011558498384,
5.39779272869779));
#84265=CARTESIAN_POINT('Ctrl Pts',(-17.5056857952746,-0.24360817999176,
5.4029807442727));
#84266=CARTESIAN_POINT('Ctrl Pts',(-17.4977635242424,-0.32509445024975,
5.4081617435776));
#84267=CARTESIAN_POINT('Ctrl Pts',(-17.4858509458476,-0.406307308451282,
5.4133427428825));
#84268=CARTESIAN_POINT('Ctrl Pts',(-17.469982063722,-0.486821173421537,
5.41852374218741));
#84269=CARTESIAN_POINT('Ctrl Pts',(-17.4541250536408,-0.567274803262042,
5.42370086541251));
#84270=CARTESIAN_POINT('Ctrl Pts',(-17.4343177025306,-0.647030014235198,
5.42887798863762));
#84271=CARTESIAN_POINT('Ctrl Pts',(-17.4106456605887,-0.725667795265136,
5.43405511186272));
#84272=CARTESIAN_POINT('Ctrl Pts',(-17.3869837657392,-0.804271867972273,
5.43923001589829));
#84273=CARTESIAN_POINT('Ctrl Pts',(-17.3594606041422,-0.88175900826378,
5.44440491993386));
#84274=CARTESIAN_POINT('Ctrl Pts',(-17.3282122408189,-0.957723348207147,
5.44957982396943));
#84275=CARTESIAN_POINT('Ctrl Pts',(-17.2969672898254,-1.03367939282381,
5.45475416290406));
#84276=CARTESIAN_POINT('Ctrl Pts',(-17.2619981263441,-1.10811252969544,
5.4599285018387));
#84277=CARTESIAN_POINT('Ctrl Pts',(-17.2234891423927,-1.18063638926725,
5.46510284077333));
#84278=CARTESIAN_POINT('Ctrl Pts',(-17.1849469545557,-1.25322278162183,
5.47028164121642));
#84279=CARTESIAN_POINT('Ctrl Pts',(-17.1428590711736,-1.32389618834014,
5.47546044165951));
#84280=CARTESIAN_POINT('Ctrl Pts',(-17.0974557680501,-1.39229506609533,
5.48063924210259));
#84281=CARTESIAN_POINT('Ctrl Pts',(-17.0520337642731,-1.4607221158913,5.48582017558327));
#84282=CARTESIAN_POINT('Ctrl Pts',(-17.0032939027791,-1.52687238923967,
5.49100110906394));
#84283=CARTESIAN_POINT('Ctrl Pts',(-16.9515082126632,-1.59041565193128,
5.49618204254462));
#84284=CARTESIAN_POINT('Ctrl Pts',(-16.8996343119159,-1.65406715285072,
5.50137180111602));
#84285=CARTESIAN_POINT('Ctrl Pts',(-16.8447045358485,-1.71510241925704,
5.50656155968743));
#84286=CARTESIAN_POINT('Ctrl Pts',(-16.7870291651781,-1.77322672346285,
5.51175131825883));
#84287=CARTESIAN_POINT('Ctrl Pts',(-16.7345255570165,-1.82613900919618,
5.51647571009749));
#84288=CARTESIAN_POINT('Ctrl Pts',(-16.6797473282794,-1.87663927633195,
5.52120010193614));
#84289=CARTESIAN_POINT('Ctrl Pts',(-16.6229512374387,-1.9245351467033,5.52592449377479));
#84290=CARTESIAN_POINT('Ctrl Pts',(-16.5596876662159,-1.97788501218986,
5.53118686122199));
#84291=CARTESIAN_POINT('Ctrl Pts',(-16.4936776611168,-2.02820751974803,
5.5364492286692));
#84292=CARTESIAN_POINT('Ctrl Pts',(-16.4252425458023,-2.07520840775929,
5.54171159611641));
#84293=CARTESIAN_POINT('Ctrl Pts',(-16.3569024508384,-2.12214403627861,
5.54696665690537));
#84294=CARTESIAN_POINT('Ctrl Pts',(-16.2861443106519,-2.16576694867464,
5.55222171769432));
#84295=CARTESIAN_POINT('Ctrl Pts',(-16.213322938943,-2.20582268005266,5.55747677848328));
#84296=CARTESIAN_POINT('Ctrl Pts',(-16.1402986576109,-2.24599002280477,
5.56274648198467));
#84297=CARTESIAN_POINT('Ctrl Pts',(-16.0651999919237,-2.28256998106267,
5.56801618548606));
#84298=CARTESIAN_POINT('Ctrl Pts',(-15.9884145738686,-2.3153494077923,5.57328588898744));
#84299=CARTESIAN_POINT('Ctrl Pts',(-15.9119748195411,-2.34798127188417,
5.57853186994617));
#84300=CARTESIAN_POINT('Ctrl Pts',(-15.8338638904551,-2.37684656188086,
5.5837778509049));
#84301=CARTESIAN_POINT('Ctrl Pts',(-15.7544877926499,-2.4017815097844,5.58902383186362));
#84302=CARTESIAN_POINT('Ctrl Pts',(-15.6751364531732,-2.42670868018759,
5.59426817653986));
#84303=CARTESIAN_POINT('Ctrl Pts',(-15.5945211671943,-2.44770780581581,
5.59951252121609));
#84304=CARTESIAN_POINT('Ctrl Pts',(-15.5130647766136,-2.4646644365914,5.60475686589233));
#84305=CARTESIAN_POINT('Ctrl Pts',(-15.4316094321405,-2.48162084960066,
5.61000114321781));
#84306=CARTESIAN_POINT('Ctrl Pts',(-15.3493134549685,-2.49453477841334,
5.6152454205433));
#84307=CARTESIAN_POINT('Ctrl Pts',(-15.266610255963,-2.50334280940812,5.62048969786879));
#84308=CARTESIAN_POINT('Ctrl Pts',(-15.1832123322294,-2.51222482976499,
5.62577802825611));
#84309=CARTESIAN_POINT('Ctrl Pts',(-15.0994007833268,-2.51693157891885,
5.63106635864342));
#84310=CARTESIAN_POINT('Ctrl Pts',(-15.0156238870574,-2.51745151773638,
5.63635468903073));
#84311=CARTESIAN_POINT('Ctrl Pts',(-14.9324247782823,-2.51796787067093,
5.64160654717688));
#84312=CARTESIAN_POINT('Ctrl Pts',(-14.8492603069933,-2.5143550643388,5.64685840532304));
#84313=CARTESIAN_POINT('Ctrl Pts',(-14.766566350805,-2.50665414076683,5.65211026346919));
#84314=CARTESIAN_POINT('Ctrl Pts',(-14.683010975526,-2.49887299703264,5.65741682997708));
#84315=CARTESIAN_POINT('Ctrl Pts',(-14.5999364514597,-2.48691813775506,
5.66272339648497));
#84316=CARTESIAN_POINT('Ctrl Pts',(-14.5177820160702,-2.47088487509529,
5.66802996299286));
#84317=CARTESIAN_POINT('Ctrl Pts',(-14.4356275806807,-2.45485161243553,
5.67333652950076));
#84318=CARTESIAN_POINT('Ctrl Pts',(-14.3543936825517,-2.43474012166965,
5.67864309600865));
#84319=CARTESIAN_POINT('Ctrl Pts',(-14.2745022103349,-2.41069683021135,
5.68394966251654));
#84320=CARTESIAN_POINT('Ctrl Pts',(-14.1961576792013,-2.38711908975994,
5.68915347781064));
#84321=CARTESIAN_POINT('Ctrl Pts',(-14.1188034503992,-2.35966984140079,
5.69435729310473));
#84322=CARTESIAN_POINT('Ctrl Pts',(-14.0428548434092,-2.32844999929455,
5.69956110839883));
#84323=CARTESIAN_POINT('Ctrl Pts',(-13.9670149075025,-2.29727482810716,
5.70475747781252));
#84324=CARTESIAN_POINT('Ctrl Pts',(-13.8925770325293,-2.26233995083739,
5.70995384722621));
#84325=CARTESIAN_POINT('Ctrl Pts',(-13.8199422128753,-2.22379627417764,
5.71515021663989));
#84326=CARTESIAN_POINT('Ctrl Pts',(-13.7460774761305,-2.18459994185093,
5.72043457558233));
#84327=CARTESIAN_POINT('Ctrl Pts',(-13.6740779020757,-2.14167158844339,
5.72571893452476));
#84328=CARTESIAN_POINT('Ctrl Pts',(-13.604344655256,-2.0952213268978,5.73100329346719));
#84329=CARTESIAN_POINT('Ctrl Pts',(-13.5358915569486,-2.04962378963984,
5.73619064324186));
#84330=CARTESIAN_POINT('Ctrl Pts',(-13.4696226850228,-2.0006328384358,5.74137799301654));
#84331=CARTESIAN_POINT('Ctrl Pts',(-13.4058915618119,-1.94849288869568,
5.74656534279121));
#84332=CARTESIAN_POINT('Ctrl Pts',(-13.3421788451239,-1.89636799777022,
5.75175119437996));
#84333=CARTESIAN_POINT('Ctrl Pts',(-13.2810027870364,-1.84109621155005,
5.75693704596871));
#84334=CARTESIAN_POINT('Ctrl Pts',(-13.2226849451813,-1.78296310839982,
5.76212289755745));
#84335=CARTESIAN_POINT('Ctrl Pts',(-13.164365513943,-1.72482842090131,5.76730889048039));
#84336=CARTESIAN_POINT('Ctrl Pts',(-13.1089047865671,-1.66383259523297,
5.77249488340333));
#84337=CARTESIAN_POINT('Ctrl Pts',(-13.0565873668425,-1.6002979682808,5.77768087632627));
#84338=CARTESIAN_POINT('Ctrl Pts',(-13.0025364217307,-1.53465813642051,
5.78303870590393));
#84339=CARTESIAN_POINT('Ctrl Pts',(-12.9518411019522,-1.46630870913287,
5.7883965354816));
#84340=CARTESIAN_POINT('Ctrl Pts',(-12.9047686108457,-1.3956402387086,5.79375436505926));
#84341=CARTESIAN_POINT('Ctrl Pts',(-12.8591296664014,-1.32712390741102,
5.7989490271791));
#84342=CARTESIAN_POINT('Ctrl Pts',(-12.8168962386622,-1.25642820507263,
5.80414368929893));
#84343=CARTESIAN_POINT('Ctrl Pts',(-12.7782654509723,-1.18393489840308,
5.80933835141876));
#84344=CARTESIAN_POINT('Ctrl Pts',(-12.7378145389097,-1.10802600426515,
5.81477776472534));
#84345=CARTESIAN_POINT('Ctrl Pts',(-12.7013143561152,-1.0301464821464,5.82021717803193));
#84346=CARTESIAN_POINT('Ctrl Pts',(-12.6689341617185,-0.950756702630547,
5.82565659133851));
#84347=CARTESIAN_POINT('Ctrl Pts',(-12.6365539673218,-0.871366923114693,
5.83109600464509));
#84348=CARTESIAN_POINT('Ctrl Pts',(-12.6082938669127,-0.790467465934306,
5.83653541795168));
#84349=CARTESIAN_POINT('Ctrl Pts',(-12.5842625352617,-0.708532816078131,
5.84197483125826));
#84350=CARTESIAN_POINT('Ctrl Pts',(-12.5604075507015,-0.627199420341229,
5.84737432897769));
#84351=CARTESIAN_POINT('Ctrl Pts',(-12.5406282933367,-0.544537571501273,
5.85277382669713));
#84352=CARTESIAN_POINT('Ctrl Pts',(-12.5250648886467,-0.460979874387583,
5.85817332441656));
#84353=CARTESIAN_POINT('Ctrl Pts',(-12.5095258535533,-0.377553014158294,
5.86356436745757));
#84354=CARTESIAN_POINT('Ctrl Pts',(-12.4981896199338,-0.293233516083529,
5.86895541049858));
#84355=CARTESIAN_POINT('Ctrl Pts',(-12.4911461993907,-0.208467880423357,
5.87434645353959));
#84356=CARTESIAN_POINT('Ctrl Pts',(-12.4841138157941,-0.123835071389566,
5.87972904888768));
#84357=CARTESIAN_POINT('Ctrl Pts',(-12.4813608876519,-0.0387579436036267,
5.88511164423578));
#84358=CARTESIAN_POINT('Ctrl Pts',(-12.4829259670636,0.0463094236313834,
5.89049423958387));
#84359=CARTESIAN_POINT('Ctrl Pts',(-12.4844896004099,0.131298192320445,
5.89587186164806));
#84360=CARTESIAN_POINT('Ctrl Pts',(-12.4903632997179,0.216276789606525,
5.90124948371226));
#84361=CARTESIAN_POINT('Ctrl Pts',(-12.5005336242105,0.300789106016054,
5.90662710577646));
#84362=CARTESIAN_POINT('Ctrl Pts',(-12.5106969819602,0.385243530901373,
5.91200104413216));
#84363=CARTESIAN_POINT('Ctrl Pts',(-12.5251510591745,0.469231883712493,
5.91737498248785));
#84364=CARTESIAN_POINT('Ctrl Pts',(-12.5438305052846,0.552302148492445,
5.92274892084355));
#84365=CARTESIAN_POINT('Ctrl Pts',(-12.562501615029,0.635335340218851,5.92812046088856));
#84366=CARTESIAN_POINT('Ctrl Pts',(-12.5853942467993,0.717450839630115,
5.93349200093357));
#84367=CARTESIAN_POINT('Ctrl Pts',(-12.6123919578486,0.798206794667818,
5.93886354097857));
#84368=CARTESIAN_POINT('Ctrl Pts',(-12.6393919087419,0.87896944956017,5.9442355266692));
#84369=CARTESIAN_POINT('Ctrl Pts',(-12.6704974923905,0.958371923001608,
5.94960751235982));
#84370=CARTESIAN_POINT('Ctrl Pts',(-12.7055425620702,1.03598808657666,5.95497949805045));
#84371=CARTESIAN_POINT('Ctrl Pts',(-12.7405870578792,1.11360297916988,5.96035139577362));
#84372=CARTESIAN_POINT('Ctrl Pts',(-12.7795707285717,1.18943122984611,5.96572329349679));
#84373=CARTESIAN_POINT('Ctrl Pts',(-12.8222800921186,1.26306858595125,5.97109519121996));
#84374=CARTESIAN_POINT('Ctrl Pts',(-12.8650202361876,1.33675901229866,5.97647096045521));
#84375=CARTESIAN_POINT('Ctrl Pts',(-12.9114912178688,1.4082550182372,5.98184672969046));
#84376=CARTESIAN_POINT('Ctrl Pts',(-12.9614347488706,1.4771790571517,5.98722249892571));
#84377=CARTESIAN_POINT('Ctrl Pts',(-13.0010044980607,1.53178686878043,5.99148166595047));
#84378=CARTESIAN_POINT('Ctrl Pts',(-13.0427531278297,1.58478068023668,5.99574083297524));
#84379=CARTESIAN_POINT('Ctrl Pts',(-13.0865340033349,1.63598720337491,6.));
#84380=CARTESIAN_POINT('',(-16.9136749826265,1.63574273981861,5.99999801496045));
#84381=CARTESIAN_POINT('Origin',(-15.,0.,6.));
#84382=CARTESIAN_POINT('',(-17.5174994024224,0.00173459013034562,5.11258330243345));
#84383=CARTESIAN_POINT('Ctrl Pts',(-16.9136749826265,1.63574273981861,5.99999801496045));
#84384=CARTESIAN_POINT('Ctrl Pts',(-16.8601965196756,1.69830783282948,5.99476349978788));
#84385=CARTESIAN_POINT('Ctrl Pts',(-16.8035449309859,1.75836640750039,5.98952898461531));
#84386=CARTESIAN_POINT('Ctrl Pts',(-16.7439851401069,1.81557761637624,5.98429446944274));
#84387=CARTESIAN_POINT('Ctrl Pts',(-16.6845090819951,1.8727083942639,5.97906731326916));
#84388=CARTESIAN_POINT('Ctrl Pts',(-16.6221332740411,1.92699943625717,5.97384015709558));
#84389=CARTESIAN_POINT('Ctrl Pts',(-16.557162345648,1.97814349310056,5.96861300092199));
#84390=CARTESIAN_POINT('Ctrl Pts',(-16.4922644958838,2.02923002363727,5.96339172419966));
#84391=CARTESIAN_POINT('Ctrl Pts',(-16.4247776903303,2.07717631690996,5.95817044747733));
#84392=CARTESIAN_POINT('Ctrl Pts',(-16.3550417101776,2.12171350886001,5.95294917075501));
#84393=CARTESIAN_POINT('Ctrl Pts',(-16.2853482658885,2.16622353509269,5.94773107878056));
#84394=CARTESIAN_POINT('Ctrl Pts',(-16.2134087614017,2.20732833758437,5.94251298680611));
#84395=CARTESIAN_POINT('Ctrl Pts',(-16.1395932525319,2.2448014319275,5.93729489483166));
#84396=CARTESIAN_POINT('Ctrl Pts',(-16.0658000387901,2.28226320795219,5.93207837892206));
#84397=CARTESIAN_POINT('Ctrl Pts',(-15.9901323607169,2.31609524368733,5.92686186301246));
#84398=CARTESIAN_POINT('Ctrl Pts',(-15.9129849843731,2.34611693406559,5.92164534710286));
#84399=CARTESIAN_POINT('Ctrl Pts',(-15.8358371547648,2.37613880083048,5.91642880054463));
#84400=CARTESIAN_POINT('Ctrl Pts',(-15.757210044023,2.40235011060392,5.9112122539864));
#84401=CARTESIAN_POINT('Ctrl Pts',(-15.6775171570007,2.4246188879842,5.90599570742817));
#84402=CARTESIAN_POINT('Ctrl Pts',(-15.5977474302612,2.44690913687365,5.90077413108652));
#84403=CARTESIAN_POINT('Ctrl Pts',(-15.5169103242883,2.46524913643255,5.89555255474486));
#84404=CARTESIAN_POINT('Ctrl Pts',(-15.4354326403361,2.47955735278093,5.89033097840321));
#84405=CARTESIAN_POINT('Ctrl Pts',(-15.3539147288184,2.49387263345271,5.88510682403904));
#84406=CARTESIAN_POINT('Ctrl Pts',(-15.271756071707,2.50415210913948,5.87988266967487));
#84407=CARTESIAN_POINT('Ctrl Pts',(-15.1893893031049,2.51036609717974,5.8746585153107));
#84408=CARTESIAN_POINT('Ctrl Pts',(-15.106883223358,2.51659059525703,5.86942552506602));
#84409=CARTESIAN_POINT('Ctrl Pts',(-15.0241687948877,2.51873585959447,5.86419253482135));
#84410=CARTESIAN_POINT('Ctrl Pts',(-14.9416790545137,2.51682437156779,5.85895954457667));
#84411=CARTESIAN_POINT('Ctrl Pts',(-14.8784767303382,2.51535981991115,5.85495011086586));
#84412=CARTESIAN_POINT('Ctrl Pts',(-14.8154063246288,2.51151487864047,5.85094067715504));
#84413=CARTESIAN_POINT('Ctrl Pts',(-14.7526593292125,2.50532010780546,5.84693124344423));
#84414=CARTESIAN_POINT('Ctrl Pts',(-14.6702583922819,2.49718497850584,5.84166595397276));
#84415=CARTESIAN_POINT('Ctrl Pts',(-14.5881137877399,2.48496590139176,5.83640066450129));
#84416=CARTESIAN_POINT('Ctrl Pts',(-14.5066608682957,2.46868846781631,5.83113537502982));
#84417=CARTESIAN_POINT('Ctrl Pts',(-14.4253200203583,2.45243343044863,5.82587733009825));
#84418=CARTESIAN_POINT('Ctrl Pts',(-14.3446694138389,2.43213121875691,5.82061928516668));
#84419=CARTESIAN_POINT('Ctrl Pts',(-14.2651391662254,2.40785917465787,5.81536124023511));
#84420=CARTESIAN_POINT('Ctrl Pts',(-14.1854437442759,2.3835367205716,5.81009227500459));
#84421=CARTESIAN_POINT('Ctrl Pts',(-14.1068738011778,2.35522798594923,5.80482330977406));
#84422=CARTESIAN_POINT('Ctrl Pts',(-14.0298517638134,2.32306234307735,5.79955434454353));
#84423=CARTESIAN_POINT('Ctrl Pts',(-13.9531201457552,2.29101798398354,5.79430524647414));
#84424=CARTESIAN_POINT('Ctrl Pts',(-13.8779252111009,2.25514591893329,5.78905614840474));
#84425=CARTESIAN_POINT('Ctrl Pts',(-13.8046676830752,2.21562336648521,5.78380705033534));
#84426=CARTESIAN_POINT('Ctrl Pts',(-13.7314323779831,2.17611280334497,5.77855954459864));
#84427=CARTESIAN_POINT('Ctrl Pts',(-13.6601337160636,2.13295417041961,5.77331203886195));
#84428=CARTESIAN_POINT('Ctrl Pts',(-13.5911487758554,2.08637112667577,5.76806453312525));
#84429=CARTESIAN_POINT('Ctrl Pts',(-13.5221641904685,2.03978832252991,5.76281705437888));
#84430=CARTESIAN_POINT('Ctrl Pts',(-13.4554936831094,1.98978140064578,5.75756957563252));
#84431=CARTESIAN_POINT('Ctrl Pts',(-13.3914850943114,1.9366171661373,5.75232209688615));
#84432=CARTESIAN_POINT('Ctrl Pts',(-13.3270228658242,1.88307614771168,5.74703742837085));
#84433=CARTESIAN_POINT('Ctrl Pts',(-13.2652608096926,1.82633317558718,5.74175275985554));
#84434=CARTESIAN_POINT('Ctrl Pts',(-13.2065187026773,1.76670062154112,5.73646809134024));
#84435=CARTESIAN_POINT('Ctrl Pts',(-13.1481049378488,1.70740138688368,5.73121296176565));
#84436=CARTESIAN_POINT('Ctrl Pts',(-13.0926777140496,1.64524517442741,5.72595783219106));
#84437=CARTESIAN_POINT('Ctrl Pts',(-13.0405117460184,1.58057332398982,5.72070270261647));
#84438=CARTESIAN_POINT('Ctrl Pts',(-12.9879059427514,1.51535619547806,5.7154032646308));
#84439=CARTESIAN_POINT('Ctrl Pts',(-12.9386169285418,1.44758119327516,5.71010382664514));
#84440=CARTESIAN_POINT('Ctrl Pts',(-12.8928815082733,1.37762763903144,5.70480438865948));
#84441=CARTESIAN_POINT('Ctrl Pts',(-12.8471460880048,1.30767408478771,5.69950495067382));
#84442=CARTESIAN_POINT('Ctrl Pts',(-12.8049644468416,1.23554241740766,5.69420551268816));
#84443=CARTESIAN_POINT('Ctrl Pts',(-12.7665250421787,1.16163499550633,5.68890607470249));
#84444=CARTESIAN_POINT('Ctrl Pts',(-12.7284410731948,1.08841096958696,5.68365563875929));
#84445=CARTESIAN_POINT('Ctrl Pts',(-12.6938903941338,1.01317465067371,5.67840520281609));
#84446=CARTESIAN_POINT('Ctrl Pts',(-12.6630904979597,0.936301356014029,
5.67315476687288));
#84447=CARTESIAN_POINT('Ctrl Pts',(-12.6323346458374,0.85953799066573,5.66791183908723));
#84448=CARTESIAN_POINT('Ctrl Pts',(-12.6053190939635,0.781142724539222,
5.66266891130157));
#84449=CARTESIAN_POINT('Ctrl Pts',(-12.5822153011964,0.701515074842446,
5.65742598351592));
#84450=CARTESIAN_POINT('Ctrl Pts',(-12.5589802614831,0.621435080114545,
5.65215327195112));
#84451=CARTESIAN_POINT('Ctrl Pts',(-12.5397017903316,0.540109073435913,
5.64688056038632));
#84452=CARTESIAN_POINT('Ctrl Pts',(-12.5245049589619,0.457963483037581,
5.64160784882152));
#84453=CARTESIAN_POINT('Ctrl Pts',(-12.5094212832647,0.376429549062439,
5.63637439788996));
#84454=CARTESIAN_POINT('Ctrl Pts',(-12.4983587538537,0.294088656736649,
5.63114094695839));
#84455=CARTESIAN_POINT('Ctrl Pts',(-12.4913891062827,0.211370844542663,
5.62590749602682));
#84456=CARTESIAN_POINT('Ctrl Pts',(-12.4844217981767,0.128680797804159,
5.62067580178037));
#84457=CARTESIAN_POINT('Ctrl Pts',(-12.4815446823358,0.0456145428386839,
5.61544410753391));
#84458=CARTESIAN_POINT('Ctrl Pts',(-12.482777705359,-0.0373921029430333,
5.61021241328745));
#84459=CARTESIAN_POINT('Ctrl Pts',(-12.4840106883402,-0.120396053103662,
5.60498088893902));
#84460=CARTESIAN_POINT('Ctrl Pts',(-12.4893535369254,-0.203339935605386,
5.59974936459058));
#84461=CARTESIAN_POINT('Ctrl Pts',(-12.4987740843549,-0.285788678756373,
5.59451784024215));
#84462=CARTESIAN_POINT('Ctrl Pts',(-12.5083234801227,-0.369365104096854,
5.58921476238537));
#84463=CARTESIAN_POINT('Ctrl Pts',(-12.5220629271967,-0.452432256540895,
5.58391168452859));
#84464=CARTESIAN_POINT('Ctrl Pts',(-12.5399048951221,-0.534544970003299,
5.5786086066718));
#84465=CARTESIAN_POINT('Ctrl Pts',(-12.5575312290757,-0.615665287861296,
5.57336962060949));
#84466=CARTESIAN_POINT('Ctrl Pts',(-12.5791612747311,-0.695853676048327,
5.56813063454718));
#84467=CARTESIAN_POINT('Ctrl Pts',(-12.6046601177278,-0.7746954875279,5.56289164848487));
#84468=CARTESIAN_POINT('Ctrl Pts',(-12.6306268756755,-0.854984080822838,
5.55755652473085));
#84469=CARTESIAN_POINT('Ctrl Pts',(-12.6606056605673,-0.933875712213862,
5.55222140097683));
#84470=CARTESIAN_POINT('Ctrl Pts',(-12.6944032211741,-1.01095486717645,
5.54688627722281));
#84471=CARTESIAN_POINT('Ctrl Pts',(-12.728200781781,-1.08803402213904,5.54155115346879));
#84472=CARTESIAN_POINT('Ctrl Pts',(-12.7658168358398,-1.1633002836756,5.53621602971477));
#84473=CARTESIAN_POINT('Ctrl Pts',(-12.8070106502183,-1.23636724388184,
5.53088090596075));
#84474=CARTESIAN_POINT('Ctrl Pts',(-12.8476084736572,-1.30837707337739,
5.52562297062609));
#84475=CARTESIAN_POINT('Ctrl Pts',(-12.8918310921115,-1.37851681878063,
5.52036503529143));
#84476=CARTESIAN_POINT('Ctrl Pts',(-12.9394814179558,-1.44639877732612,
5.51510709995677));
#84477=CARTESIAN_POINT('Ctrl Pts',(-12.9870645433647,-1.51418500311242,
5.50985657979792));
#84478=CARTESIAN_POINT('Ctrl Pts',(-13.0380655113944,-1.5797193927513,5.50460605963908));
#84479=CARTESIAN_POINT('Ctrl Pts',(-13.0922418902519,-1.64263971846856,
5.49935553948023));
#84480=CARTESIAN_POINT('Ctrl Pts',(-13.1466277812793,-1.70580337115317,
5.49408471438601));
#84481=CARTESIAN_POINT('Ctrl Pts',(-13.2042134634477,-1.76633228979876,
5.4888138892918));
#84482=CARTESIAN_POINT('Ctrl Pts',(-13.2647102936331,-1.82389031604891,
5.48354306419758));
#84483=CARTESIAN_POINT('Ctrl Pts',(-13.3248672587503,-1.88112498713392,
5.4783018500652));
#84484=CARTESIAN_POINT('Ctrl Pts',(-13.3879024126295,-1.93542173658785,
5.47306063593282));
#84485=CARTESIAN_POINT('Ctrl Pts',(-13.4534935008024,-1.98648531279234,
5.46781942180044));
#84486=CARTESIAN_POINT('Ctrl Pts',(-13.5190631933413,-2.03753223219757,
5.46257991733781));
#84487=CARTESIAN_POINT('Ctrl Pts',(-13.5871868008729,-2.08534779016708,
5.45734041287518));
#84488=CARTESIAN_POINT('Ctrl Pts',(-13.6575090010332,-2.12967701018091,
5.45210090841256));
#84489=CARTESIAN_POINT('Ctrl Pts',(-13.7278294112263,-2.17400510184766,
5.44686153731522));
#84490=CARTESIAN_POINT('Ctrl Pts',(-13.8003479123409,-2.21484678715634,
5.44162216621789));
#84491=CARTESIAN_POINT('Ctrl Pts',(-13.8746813908686,-2.25199118069822,
5.43638279512056));
#84492=CARTESIAN_POINT('Ctrl Pts',(-13.9497888020879,-2.2895223079305,5.43108887362876));
#84493=CARTESIAN_POINT('Ctrl Pts',(-14.0267487836657,-2.32327847440813,
5.42579495213697));
#84494=CARTESIAN_POINT('Ctrl Pts',(-14.1051436162847,-2.35309122273742,
5.42050103064517));
#84495=CARTESIAN_POINT('Ctrl Pts',(-14.1828412936084,-2.38263885008021,
5.4152541873252));
#84496=CARTESIAN_POINT('Ctrl Pts',(-14.2619479411992,-2.40831283198857,
5.41000734400523));
#84497=CARTESIAN_POINT('Ctrl Pts',(-14.342041527954,-2.429999361947,5.40476050068526));
#84498=CARTESIAN_POINT('Ctrl Pts',(-14.4232130941935,-2.45197777088524,
5.39944304010755));
#84499=CARTESIAN_POINT('Ctrl Pts',(-14.5053978855086,-2.46986048981595,
5.39412557952984));
#84500=CARTESIAN_POINT('Ctrl Pts',(-14.5881477291731,-2.48358288708365,
5.38880811895214));
#84501=CARTESIAN_POINT('Ctrl Pts',(-14.6708975728377,-2.49730528435134,
5.38349065837443));
#84502=CARTESIAN_POINT('Ctrl Pts',(-14.7542119789289,-2.50686736759322,
5.37817319779672));
#84503=CARTESIAN_POINT('Ctrl Pts',(-14.8376411648922,-2.51225911455456,
5.37285573721902));
#84504=CARTESIAN_POINT('Ctrl Pts',(-14.9201316740945,-2.5175901980021,5.36759810434566));
#84505=CARTESIAN_POINT('Ctrl Pts',(-15.0030356775818,-2.51886382893295,
5.3623404714723));
#84506=CARTESIAN_POINT('Ctrl Pts',(-15.0859207937919,-2.51603335971409,
5.35708283859894));
#84507=CARTESIAN_POINT('Ctrl Pts',(-15.1686892613134,-2.51320687396702,
5.35183260507552));
#84508=CARTESIAN_POINT('Ctrl Pts',(-15.2514384374779,-2.50628777674198,
5.3465823715521));
#84509=CARTESIAN_POINT('Ctrl Pts',(-15.3337325172041,-2.49528131820053,
5.34133213802868));
#84510=CARTESIAN_POINT('Ctrl Pts',(-15.4163505109539,-2.48423153763296,
5.33606123929737));
#84511=CARTESIAN_POINT('Ctrl Pts',(-15.4985093486618,-2.46906212071437,
5.33079034056606));
#84512=CARTESIAN_POINT('Ctrl Pts',(-15.5797697411648,-2.44983127933939,
5.32551944183476));
#84513=CARTESIAN_POINT('Ctrl Pts',(-15.6605687069665,-2.43070963782707,
5.32027847322488));
#84514=CARTESIAN_POINT('Ctrl Pts',(-15.7404789506386,-2.40757268016484,
5.315037504615));
#84515=CARTESIAN_POINT('Ctrl Pts',(-15.819077180215,-2.3805291056509,5.30979653600512));
#84516=CARTESIAN_POINT('Ctrl Pts',(-15.8976500117061,-2.35349426994715,
5.30455726095206));
#84517=CARTESIAN_POINT('Ctrl Pts',(-15.9749112356448,-2.32255547450268,
5.29931798589899));
#84518=CARTESIAN_POINT('Ctrl Pts',(-16.0504532418526,-2.28787111452574,
5.29407871084593));
#84519=CARTESIAN_POINT('Ctrl Pts',(-16.1259935631639,-2.25318752815229,
5.28883955265019));
#84520=CARTESIAN_POINT('Ctrl Pts',(-16.1998143245709,-2.21475873667251,
5.28360039445445));
#84521=CARTESIAN_POINT('Ctrl Pts',(-16.2715296766866,-2.1727904941124,5.27836123625871));
#84522=CARTESIAN_POINT('Ctrl Pts',(-16.3439987649109,-2.13038116078311,
5.27306701394359));
#84523=CARTESIAN_POINT('Ctrl Pts',(-16.4143175040774,-2.0843577657645,5.26777279162847));
#84524=CARTESIAN_POINT('Ctrl Pts',(-16.4821165896087,-2.03497829590555,
5.26247856931335));
#84525=CARTESIAN_POINT('Ctrl Pts',(-16.5493067545363,-1.98604231545892,
5.25723189573762));
#84526=CARTESIAN_POINT('Ctrl Pts',(-16.6140220197145,-1.93381064268263,
5.25198522216188));
#84527=CARTESIAN_POINT('Ctrl Pts',(-16.675936614042,-1.87857465002416,5.24673854858615));
#84528=CARTESIAN_POINT('Ctrl Pts',(-16.7386928733409,-1.82258778108712,
5.24142055190134));
#84529=CARTESIAN_POINT('Ctrl Pts',(-16.7985713958735,-1.76351464093587,
5.23610255521653));
#84530=CARTESIAN_POINT('Ctrl Pts',(-16.8552732205997,-1.70169548595674,
5.23078455853172));
#84531=CARTESIAN_POINT('Ctrl Pts',(-16.9119750453259,-1.63987633097761,
5.22546656184691));
#84532=CARTESIAN_POINT('Ctrl Pts',(-16.9654999110301,-1.57531157616454,
5.22014856516209));
#84533=CARTESIAN_POINT('Ctrl Pts',(-17.0155937543497,-1.50837265535626,
5.21483056847728));
#84534=CARTESIAN_POINT('Ctrl Pts',(-17.0652590935927,-1.44200633186824,
5.20955806207845));
#84535=CARTESIAN_POINT('Ctrl Pts',(-17.1117359074679,-1.37306056413704,
5.20428555567962));
#84536=CARTESIAN_POINT('Ctrl Pts',(-17.1547466573534,-1.30187291723276,
5.1990130492808));
#84537=CARTESIAN_POINT('Ctrl Pts',(-17.197696533977,-1.23078602244963,5.19374800507838));
#84538=CARTESIAN_POINT('Ctrl Pts',(-17.2371898539945,-1.15746393684039,
5.18848296087597));
#84539=CARTESIAN_POINT('Ctrl Pts',(-17.272990456247,-1.08227567459038,5.18321791667355));
#84540=CARTESIAN_POINT('Ctrl Pts',(-17.3087509397028,-1.00717166965515,
5.17795877257407));
#84541=CARTESIAN_POINT('Ctrl Pts',(-17.3408267304195,-0.930206052660622,
5.17269962847459));
#84542=CARTESIAN_POINT('Ctrl Pts',(-17.3690266765522,-0.851773946410638,
5.16744048437511));
#84543=CARTESIAN_POINT('Ctrl Pts',(-17.3972030141169,-0.773407502332921,
5.16218574315147));
#84544=CARTESIAN_POINT('Ctrl Pts',(-17.4215098023069,-0.693577437973085,
5.15693100192783));
#84545=CARTESIAN_POINT('Ctrl Pts',(-17.4418038266195,-0.612699210303533,
5.15167626070419));
#84546=CARTESIAN_POINT('Ctrl Pts',(-17.4620878926168,-0.531860669729495,
5.14642409799177));
#84547=CARTESIAN_POINT('Ctrl Pts',(-17.4783629982323,-0.449975431039625,
5.14117193527934));
#84548=CARTESIAN_POINT('Ctrl Pts',(-17.4905360163053,-0.367473266355765,
5.13591977256691));
#84549=CARTESIAN_POINT('Ctrl Pts',(-17.5027088852941,-0.284972112083975,
5.13066767417824));
#84550=CARTESIAN_POINT('Ctrl Pts',(-17.5107796928322,-0.201854497924812,
5.12541557578956));
#84551=CARTESIAN_POINT('Ctrl Pts',(-17.51470677117,-0.118558445635614,5.12016347740088));
#84552=CARTESIAN_POINT('Ctrl Pts',(-17.5165960440205,-0.0784856595574208,
5.11763675243125));
#84553=CARTESIAN_POINT('Ctrl Pts',(-17.5175270361368,-0.0383716548339769,
5.11511002746161));
#84554=CARTESIAN_POINT('Ctrl Pts',(-17.517499402423,0.00173458920130465,
5.11258330249198));
#84555=CARTESIAN_POINT('Ctrl Pts',(-17.5174994024224,0.00173459013034678,
5.11258330243345));
#84556=CARTESIAN_POINT('Ctrl Pts',(-17.5174339072919,0.0967910238682339,
5.1065946722231));
#84557=CARTESIAN_POINT('Ctrl Pts',(-17.5119806399526,0.191636187933136,
5.10060604201275));
#84558=CARTESIAN_POINT('Ctrl Pts',(-17.5012351672351,0.28570769710728,5.0946174118024));
#84559=CARTESIAN_POINT('Ctrl Pts',(-17.4899274076477,0.38470176072171,5.08831540979126));
#84560=CARTESIAN_POINT('Ctrl Pts',(-17.4727588141368,0.482838716783771,
5.08201340778011));
#84561=CARTESIAN_POINT('Ctrl Pts',(-17.4498986037571,0.579485186444757,
5.07571140576897));
#84562=CARTESIAN_POINT('Ctrl Pts',(-17.4270383933775,0.676131656105743,
5.06940940375783));
#84563=CARTESIAN_POINT('Ctrl Pts',(-17.3984867566974,0.771287459178277,
5.06310740174669));
#84564=CARTESIAN_POINT('Ctrl Pts',(-17.3644692274603,0.864344562309186,
5.05680539973555));
#84565=CARTESIAN_POINT('Ctrl Pts',(-17.363460773153,0.867103252860236,5.05661857602391));
#84566=CARTESIAN_POINT('Ctrl Pts',(-17.3624474254085,0.869860357624826,
5.05643175231228));
#84567=CARTESIAN_POINT('Ctrl Pts',(-17.3614291890287,0.872615857753804,
5.05624492860065));
#84568=CARTESIAN_POINT('Origin',(15.,0.,3.));
#84569=CARTESIAN_POINT('',(12.6385711154041,0.872616681594025,0.329758541657823));
#84570=CARTESIAN_POINT('',(12.638571011945,0.872616401618522,0.0533220355972278));
#84571=CARTESIAN_POINT('',(12.6385710119932,0.872616401748847,3.));
#84572=CARTESIAN_POINT('',(13.0865340033349,1.63598720337496,0.));
#84573=CARTESIAN_POINT('Ctrl Pts',(12.6385710118969,0.872616401488192,0.0533220355972278));
#84574=CARTESIAN_POINT('Ctrl Pts',(12.7166299025009,1.08385529951616,0.0396751487715243));
#84575=CARTESIAN_POINT('Ctrl Pts',(12.8226742739707,1.28365497417919,0.0268312150403422));
#84576=CARTESIAN_POINT('Ctrl Pts',(12.9793449478575,1.50222218660785,0.0106203823935272));
#84577=CARTESIAN_POINT('Ctrl Pts',(13.0057407311186,1.53709073746681,0.007956856747876));
#84578=CARTESIAN_POINT('Ctrl Pts',(13.0423686652523,1.58294336564474,0.00432561398330578));
#84579=CARTESIAN_POINT('Ctrl Pts',(13.051811403343,1.59455050544773,0.00339493848341432));
#84580=CARTESIAN_POINT('Ctrl Pts',(13.0696718411553,1.61610931727312,0.0016434387339535));
#84581=CARTESIAN_POINT('Ctrl Pts',(13.0780644827079,1.62608117251209,0.000823946587482173));
#84582=CARTESIAN_POINT('Ctrl Pts',(13.0865340033349,1.63598720337495,-1.60982338570648E-14));
#84583=CARTESIAN_POINT('',(16.8880578635265,1.66524585391345,0.));
#84584=CARTESIAN_POINT('Origin',(15.,0.,0.));
#84585=CARTESIAN_POINT('Ctrl Pts',(16.8880578635265,1.66524585391345,3.08840071030179E-15));
#84586=CARTESIAN_POINT('Ctrl Pts',(16.886468234627,1.66704817717801,0.000157709303802153));
#84587=CARTESIAN_POINT('Ctrl Pts',(16.8848760275067,1.66884822143744,0.000315569528701009));
#84588=CARTESIAN_POINT('Ctrl Pts',(16.8675293390091,1.68840274915651,0.0020342519324443));
#84589=CARTESIAN_POINT('Ctrl Pts',(16.8515276439882,1.70593522077278,0.00360923991232524));
#84590=CARTESIAN_POINT('Ctrl Pts',(16.746920121793,1.81734419855081,0.0138250880846664));
#84591=CARTESIAN_POINT('Ctrl Pts',(16.6514572692786,1.90450911841386,0.0227735767256802));
#84592=CARTESIAN_POINT('Ctrl Pts',(16.4655835905919,2.04970103866705,0.0390520747993906));
#84593=CARTESIAN_POINT('Ctrl Pts',(16.3773252408062,2.11002087102476,0.0463805523543274));
#84594=CARTESIAN_POINT('Ctrl Pts',(16.2216753731421,2.20245891379776,0.0585289141545112));
#84595=CARTESIAN_POINT('Ctrl Pts',(16.1562045639331,2.23752290892545,0.0634280294569529));
#84596=CARTESIAN_POINT('Ctrl Pts',(16.0528497743807,2.28712612817112,0.0708430408491615));
#84597=CARTESIAN_POINT('Ctrl Pts',(16.0160083287123,2.30372870673535,0.0734266879775329));
#84598=CARTESIAN_POINT('Ctrl Pts',(15.94497261254,2.33370512157807,0.0783006526532379));
#84599=CARTESIAN_POINT('Ctrl Pts',(15.910854614212,2.34723175800297,0.0805955447360372));
#84600=CARTESIAN_POINT('Ctrl Pts',(15.8288656360263,2.37768053869943,0.0860089184852513));
#84601=CARTESIAN_POINT('Ctrl Pts',(15.7807538665597,2.39391038027243,0.0891045683531706));
#84602=CARTESIAN_POINT('Ctrl Pts',(15.5990595642084,2.44914125421226,0.100539787843066));
#84603=CARTESIAN_POINT('Ctrl Pts',(15.462808046805,2.47850325418664,0.108591467885766));
#84604=CARTESIAN_POINT('Ctrl Pts',(15.2253859502372,2.50939468051778,0.122422059661358));
#84605=CARTESIAN_POINT('Ctrl Pts',(15.125273894214,2.516379343425,0.128200030717063));
#84606=CARTESIAN_POINT('Ctrl Pts',(14.9667513012163,2.51795474179782,0.137591990224574));
#84607=CARTESIAN_POINT('Ctrl Pts',(14.9084866311484,2.5165106479514,0.141096639099316));
#84608=CARTESIAN_POINT('Ctrl Pts',(14.8248665008829,2.51153044071001,0.146267321924945));
#84609=CARTESIAN_POINT('Ctrl Pts',(14.7994295285805,2.50962711623503,0.14785907411809));
#84610=CARTESIAN_POINT('Ctrl Pts',(14.7530459802166,2.50544681514215,0.15080313989314));
#84611=CARTESIAN_POINT('Ctrl Pts',(14.7320916688765,2.50329284006455,0.152149268741038));
#84612=CARTESIAN_POINT('Ctrl Pts',(14.6794099856822,2.49720849657372,0.155572683213796));
#84613=CARTESIAN_POINT('Ctrl Pts',(14.6477270715622,2.49293637939985,0.157666654694749));
#84614=CARTESIAN_POINT('Ctrl Pts',(14.4673669781114,2.46511000129541,0.169756462952325));
#84615=CARTESIAN_POINT('Ctrl Pts',(14.3209665486788,2.42886252867742,0.180210756369125));
#84616=CARTESIAN_POINT('Ctrl Pts',(14.0843315655944,2.34719445402622,0.197453226058448));
#84617=CARTESIAN_POINT('Ctrl Pts',(13.9919860859851,2.30904336494997,0.204280269545649));
#84618=CARTESIAN_POINT('Ctrl Pts',(13.8382433131025,2.23454018949238,0.215718581124496));
#84619=CARTESIAN_POINT('Ctrl Pts',(13.7756768419529,2.20088228388439,0.220396685642392));
#84620=CARTESIAN_POINT('Ctrl Pts',(13.6805397286415,2.14438828975984,0.227545574717692));
#84621=CARTESIAN_POINT('Ctrl Pts',(13.6469483082922,2.12335299794718,0.230077301403896));
#84622=CARTESIAN_POINT('Ctrl Pts',(13.5834506362853,2.08147104146295,0.234881828283064));
#84623=CARTESIAN_POINT('Ctrl Pts',(13.5534733149894,2.06075097106388,0.237158484389709));
#84624=CARTESIAN_POINT('Ctrl Pts',(13.482662082323,2.00949999029175,0.242563725080266));
#84625=CARTESIAN_POINT('Ctrl Pts',(13.4422844013235,1.97836478432708,0.245668417791289));
#84626=CARTESIAN_POINT('Ctrl Pts',(13.279613462669,1.84485899511896,0.258319460919686));
#84627=CARTESIAN_POINT('Ctrl Pts',(13.1662371057772,1.73221062665261,0.267457248192311));
#84628=CARTESIAN_POINT('Ctrl Pts',(13.00517208062,1.53850980009479,0.281947428721557));
#84629=CARTESIAN_POINT('Ctrl Pts',(12.9500342716112,1.46423683991663,0.287272277954226));
#84630=CARTESIAN_POINT('Ctrl Pts',(12.8683536417112,1.34052439862417,0.296051962677933));
#84631=CARTESIAN_POINT('Ctrl Pts',(12.8391588983321,1.29293721878651,0.299410139190968));
#84632=CARTESIAN_POINT('Ctrl Pts',(12.7992790396188,1.22280495597283,0.304390131558912));
#84633=CARTESIAN_POINT('Ctrl Pts',(12.7873077518174,1.20100691329311,0.305942156141811));
#84634=CARTESIAN_POINT('Ctrl Pts',(12.7660063472958,1.16082025214006,0.308817609561179));
#84635=CARTESIAN_POINT('Ctrl Pts',(12.7565759229868,1.1424883350368,0.310135114495249));
#84636=CARTESIAN_POINT('Ctrl Pts',(12.7335338142861,1.09631101818298,0.313466563384216));
#84637=CARTESIAN_POINT('Ctrl Pts',(12.720209704722,1.06832711268394,0.315496282044171));
#84638=CARTESIAN_POINT('Ctrl Pts',(12.6824463866629,0.985089492982362,0.321550207798017));
#84639=CARTESIAN_POINT('Ctrl Pts',(12.6594887716053,0.929222931042817,0.325634208538604));
#84640=CARTESIAN_POINT('Ctrl Pts',(12.6385711154041,0.872616681594026,0.329758541657824));
#84641=CARTESIAN_POINT('Origin',(15.,0.,3.));
#84642=CARTESIAN_POINT('',(12.6385710124998,0.872616403119952,1.33336808075876));
#84643=CARTESIAN_POINT('',(12.6385710119932,0.872616401748846,1.05617156246159));
#84644=CARTESIAN_POINT('',(12.6385710119932,0.872616401748847,3.));
#84645=CARTESIAN_POINT('',(12.4825021902374,-0.00332081924700182,0.112584992770917));
#84646=CARTESIAN_POINT('Ctrl Pts',(12.6385710119932,0.872616401748845,1.05617156246159));
#84647=CARTESIAN_POINT('Ctrl Pts',(12.6673553413416,0.950511052350811,1.05093096369482));
#84648=CARTESIAN_POINT('Ctrl Pts',(12.7000170560672,1.02703174438234,1.04569036492805));
#84649=CARTESIAN_POINT('Ctrl Pts',(12.736395609459,1.10177194242888,1.04044976616129));
#84650=CARTESIAN_POINT('Ctrl Pts',(12.7727641011313,1.17649146854538,1.03521061685939));
#84651=CARTESIAN_POINT('Ctrl Pts',(12.8128471878283,1.2494310646912,1.02997146755749));
#84652=CARTESIAN_POINT('Ctrl Pts',(12.85643698191,1.32020598297274,1.0247323182556));
#84653=CARTESIAN_POINT('Ctrl Pts',(12.9000278329709,1.39098261742689,1.01949304191315));
#84654=CARTESIAN_POINT('Ctrl Pts',(12.9471253173508,1.4595940780719,1.0142537655707));
#84655=CARTESIAN_POINT('Ctrl Pts',(12.9974772901859,1.52568314098265,1.00901448922826));
#84656=CARTESIAN_POINT('Ctrl Pts',(13.0478795569234,1.59183821673646,1.00376997965188));
#84657=CARTESIAN_POINT('Ctrl Pts',(13.1015425249499,1.6554654950733,0.998525470075494));
#84658=CARTESIAN_POINT('Ctrl Pts',(13.1581729809938,1.71623992555195,0.993280960499111));
#84659=CARTESIAN_POINT('Ctrl Pts',(13.2148315550953,1.77704453164743,0.988033846927755));
#84660=CARTESIAN_POINT('Ctrl Pts',(13.2744602214017,1.83499314665331,0.982786733356399));
#84661=CARTESIAN_POINT('Ctrl Pts',(13.3367297778327,1.8897985125541,0.977539619785042));
#84662=CARTESIAN_POINT('Ctrl Pts',(13.3991082283029,1.94469971947257,0.972283330310994));
#84663=CARTESIAN_POINT('Ctrl Pts',(13.4641364345657,1.99644640751603,0.967027040836946));
#84664=CARTESIAN_POINT('Ctrl Pts',(13.5314532192717,2.04479255740346,0.961770751362896));
#84665=CARTESIAN_POINT('Ctrl Pts',(13.5895954402337,2.08654963985611,0.957230838392084));
#84666=CARTESIAN_POINT('Ctrl Pts',(13.6494442930343,2.12577054198976,0.95269092542127));
#84667=CARTESIAN_POINT('Ctrl Pts',(13.7107523710849,2.16232439780365,0.948151012450456));
#84668=CARTESIAN_POINT('Ctrl Pts',(13.7817562354166,2.20465919448186,0.942893118631136));
#84669=CARTESIAN_POINT('Ctrl Pts',(13.8549771790876,2.24357028609219,0.937635224811814));
#84670=CARTESIAN_POINT('Ctrl Pts',(13.9300515382914,2.27881911069908,0.932377330992491));
#84671=CARTESIAN_POINT('Ctrl Pts',(14.0050201766223,2.31401829736638,0.927126841420507));
#84672=CARTESIAN_POINT('Ctrl Pts',(14.0818366323,2.34556526698025,0.921876351848521));
#84673=CARTESIAN_POINT('Ctrl Pts',(14.1601105462379,2.37326609453285,0.916625862276535));
#84674=CARTESIAN_POINT('Ctrl Pts',(14.2386877550134,2.40107425692501,0.911355028169543));
#84675=CARTESIAN_POINT('Ctrl Pts',(14.3187333363833,2.42500616826725,0.906084194062551));
#84676=CARTESIAN_POINT('Ctrl Pts',(14.3998297718509,2.4449134846132,0.900813359955558));
#84677=CARTESIAN_POINT('Ctrl Pts',(14.4804704191395,2.46470891540691,0.895572149639866));
#84678=CARTESIAN_POINT('Ctrl Pts',(14.56214968765,2.48052475906152,0.890330939324172));
#84679=CARTESIAN_POINT('Ctrl Pts',(14.644441218443,2.49226487413712,0.885089729008479));
#84680=CARTESIAN_POINT('Ctrl Pts',(14.7267060638877,2.50400118214949,0.879850218302962));
#84681=CARTESIAN_POINT('Ctrl Pts',(14.8095823213893,2.51166432158278,0.874610707597444));
#84682=CARTESIAN_POINT('Ctrl Pts',(14.8926349439582,2.5152095329696,0.869371196891926));
#84683=CARTESIAN_POINT('Ctrl Pts',(14.9756856116639,2.51875466091049,0.864131809512157));
#84684=CARTESIAN_POINT('Ctrl Pts',(15.0589121756989,2.51818203495976,0.858892422132388));
#84685=CARTESIAN_POINT('Ctrl Pts',(15.1418773763537,2.5134989675906,0.853653034752618));
#84686=CARTESIAN_POINT('Ctrl Pts',(15.2257062951751,2.50876714664366,0.848359102165621));
#84687=CARTESIAN_POINT('Ctrl Pts',(15.3092678970014,2.49983881025923,0.843065169578624));
#84688=CARTESIAN_POINT('Ctrl Pts',(15.3921159728945,2.48677528413827,0.837771236991626));
#84689=CARTESIAN_POINT('Ctrl Pts',(15.4742277569492,2.47382785688336,0.832524352924652));
#84690=CARTESIAN_POINT('Ctrl Pts',(15.5556382037615,2.45681860473001,0.827277468857679));
#84691=CARTESIAN_POINT('Ctrl Pts',(15.6359245095989,2.43585842529721,0.822030584790705));
#84692=CARTESIAN_POINT('Ctrl Pts',(15.7172906997503,2.41461632270512,0.816713127943696));
#84693=CARTESIAN_POINT('Ctrl Pts',(15.7975018164948,2.38931636558638,0.811395671096688));
#84694=CARTESIAN_POINT('Ctrl Pts',(15.8761368135256,2.36012510981624,0.80607821424968));
#84695=CARTESIAN_POINT('Ctrl Pts',(15.9547718105564,2.33093385404611,0.800760757402672));
#84696=CARTESIAN_POINT('Ctrl Pts',(16.0318302665396,2.29785154969403,0.795443300555665));
#84697=CARTESIAN_POINT('Ctrl Pts',(16.1069168706898,2.2610929417833,0.790125843708659));
#84698=CARTESIAN_POINT('Ctrl Pts',(16.1810520127557,2.22480012163988,0.784875767170463));
#84699=CARTESIAN_POINT('Ctrl Pts',(16.2535384001907,2.1847898098043,0.779625690632268));
#84700=CARTESIAN_POINT('Ctrl Pts',(16.3239782521661,2.14123511968937,0.774375614094074));
#84701=CARTESIAN_POINT('Ctrl Pts',(16.394318339877,2.0977421162689,0.769132973261804));
#84702=CARTESIAN_POINT('Ctrl Pts',(16.462617259154,2.05071494621835,0.763890332429535));
#84703=CARTESIAN_POINT('Ctrl Pts',(16.5284999384715,2.0003735121453,0.758647691597266));
#84704=CARTESIAN_POINT('Ctrl Pts',(16.5947615229,1.94974255392328,0.753374899237668));
#84705=CARTESIAN_POINT('Ctrl Pts',(16.6585785565492,1.89575929024698,0.74810210687807));
#84706=CARTESIAN_POINT('Ctrl Pts',(16.7195972934524,1.83869285046503,0.742829314518473));
#84707=CARTESIAN_POINT('Ctrl Pts',(16.7801594987239,1.78205337191156,0.737595972278981));
#84708=CARTESIAN_POINT('Ctrl Pts',(16.8379647960742,1.72237701765057,0.732362630039489));
#84709=CARTESIAN_POINT('Ctrl Pts',(16.8927002954464,1.65996742185417,0.727129287799997));
#84710=CARTESIAN_POINT('Ctrl Pts',(16.9474181233827,1.59757797508687,0.721897635152686));
#84711=CARTESIAN_POINT('Ctrl Pts',(16.9990678169288,1.5324573866207,0.716665982505374));
#84712=CARTESIAN_POINT('Ctrl Pts',(17.0473747558102,1.46494466082204,0.711434329858064));
#84713=CARTESIAN_POINT('Ctrl Pts',(17.095680745222,1.39743326198149,0.706202780038535));
#84714=CARTESIAN_POINT('Ctrl Pts',(17.1406438424178,1.32753019598549,0.700971230219008));
#84715=CARTESIAN_POINT('Ctrl Pts',(17.1820318275012,1.25560477610262,0.69573968039948));
#84716=CARTESIAN_POINT('Ctrl Pts',(17.2239870526643,1.18269358750389,0.690436429946769));
#84717=CARTESIAN_POINT('Ctrl Pts',(17.2622681664442,1.10770460373393,0.685133179494059));
#84718=CARTESIAN_POINT('Ctrl Pts',(17.2966815251688,1.03104811815365,0.679829929041348));
#84719=CARTESIAN_POINT('Ctrl Pts',(17.33067909875,0.955317802788523,0.674590752914191));
#84720=CARTESIAN_POINT('Ctrl Pts',(17.3609017606068,0.87796052028999,0.669351576787034));
#84721=CARTESIAN_POINT('Ctrl Pts',(17.3872121270175,0.799390086641513,0.664112400659877));
#84722=CARTESIAN_POINT('Ctrl Pts',(17.4140051510851,0.719378296349657,0.658777113044389));
#84723=CARTESIAN_POINT('Ctrl Pts',(17.4367407694382,0.638108884838129,0.653441825428902));
#84724=CARTESIAN_POINT('Ctrl Pts',(17.4553280524873,0.556030938589552,0.648106537813414));
#84725=CARTESIAN_POINT('Ctrl Pts',(17.4739153355365,0.473952992340981,0.642771250197926));
#84726=CARTESIAN_POINT('Ctrl Pts',(17.4883542636022,0.391067014483707,0.637435962582438));
#84727=CARTESIAN_POINT('Ctrl Pts',(17.4986093954603,0.307826800194012,0.63210067496695));
#84728=CARTESIAN_POINT('Ctrl Pts',(17.5087318015308,0.225663912178923,0.62683443865773));
#84729=CARTESIAN_POINT('Ctrl Pts',(17.5148155050885,0.142852881066483,0.62156820234851));
#84730=CARTESIAN_POINT('Ctrl Pts',(17.5167890973848,0.0598238187100271,
0.616301966039289));
#84731=CARTESIAN_POINT('Ctrl Pts',(17.5187598990122,-0.0230878401543792,
0.611043176213446));
#84732=CARTESIAN_POINT('Ctrl Pts',(17.5166321236805,-0.106216462358676,
0.605784386387601));
#84733=CARTESIAN_POINT('Ctrl Pts',(17.5103859807718,-0.189125560262059,
0.600525596561758));
#84734=CARTESIAN_POINT('Ctrl Pts',(17.5041280031666,-0.272191747753212,
0.595256842797735));
#84735=CARTESIAN_POINT('Ctrl Pts',(17.4937359923408,-0.355037115582707,
0.589988089033713));
#84736=CARTESIAN_POINT('Ctrl Pts',(17.4792425788845,-0.43722132272559,0.58471933526969));
#84737=CARTESIAN_POINT('Ctrl Pts',(17.4648025487528,-0.519102822282364,
0.579469987809983));
#84738=CARTESIAN_POINT('Ctrl Pts',(17.4462913438407,-0.600327566507047,
0.574220640350275));
#84739=CARTESIAN_POINT('Ctrl Pts',(17.4237930655656,-0.68046559451328,0.568971292890567));
#84740=CARTESIAN_POINT('Ctrl Pts',(17.4013024125812,-0.76057646151839,0.563723724580357));
#84741=CARTESIAN_POINT('Ctrl Pts',(17.3748274944993,-0.839600902075373,
0.558476156270146));
#84742=CARTESIAN_POINT('Ctrl Pts',(17.3445029388326,-0.917121703922343,
0.553228587959936));
#84743=CARTESIAN_POINT('Ctrl Pts',(17.314179617978,-0.994639349132042,0.547981233330045));
#84744=CARTESIAN_POINT('Ctrl Pts',(17.2800071394821,-1.07065305001508,0.542733878700155));
#84745=CARTESIAN_POINT('Ctrl Pts',(17.2421686879526,-1.14476452808648,0.537486524070264));
#84746=CARTESIAN_POINT('Ctrl Pts',(17.2040641747517,-1.21939712218985,0.532202272583175));
#84747=CARTESIAN_POINT('Ctrl Pts',(17.1622421292968,-1.2921002088261,0.526918021096086));
#84748=CARTESIAN_POINT('Ctrl Pts',(17.1169363851008,-1.36249278582903,0.521633769608997));
#84749=CARTESIAN_POINT('Ctrl Pts',(17.0718852968847,-1.43248969797793,0.516379220012112));
#84750=CARTESIAN_POINT('Ctrl Pts',(17.0233898863071,-1.50020166271471,0.511124670415227));
#84751=CARTESIAN_POINT('Ctrl Pts',(16.9717222308726,-1.56528517985794,0.505870120818341));
#84752=CARTESIAN_POINT('Ctrl Pts',(16.9196164902129,-1.63092053406481,0.500571018386151));
#84753=CARTESIAN_POINT('Ctrl Pts',(16.8642847681636,-1.69388229767138,0.495271915953962));
#84754=CARTESIAN_POINT('Ctrl Pts',(16.8060446762978,-1.75385543224533,0.489972813521772));
#84755=CARTESIAN_POINT('Ctrl Pts',(16.747804584432,-1.81382856681928,0.484673711089583));
#84756=CARTESIAN_POINT('Ctrl Pts',(16.6866565091649,-1.87081279348982,0.479374608657392));
#84757=CARTESIAN_POINT('Ctrl Pts',(16.6229513048051,-1.92453508989352,0.474075506225203));
#84758=CARTESIAN_POINT('Ctrl Pts',(16.5596871988428,-1.97788541011264,0.468813095074594));
#84759=CARTESIAN_POINT('Ctrl Pts',(16.4936766262849,-2.02820830944165,0.463550683923985));
#84760=CARTESIAN_POINT('Ctrl Pts',(16.4252409185095,-2.0752095253748,0.458288272773376));
#84761=CARTESIAN_POINT('Ctrl Pts',(16.3569002284007,-2.122145483769,0.453033168072055));
#84762=CARTESIAN_POINT('Ctrl Pts',(16.2861414678863,-2.1657686620384,0.447778063370734));
#84763=CARTESIAN_POINT('Ctrl Pts',(16.2133194579239,-2.20582459479969,0.442522958669413));
#84764=CARTESIAN_POINT('Ctrl Pts',(16.1402952985317,-2.24599172037171,0.437253266119998));
#84765=CARTESIAN_POINT('Ctrl Pts',(16.0651967800906,-2.28257147155383,0.431983573570583));
#84766=CARTESIAN_POINT('Ctrl Pts',(15.9884115291994,-2.31535070754857,0.426713881021168));
#84767=CARTESIAN_POINT('Ctrl Pts',(15.911971140087,-2.34798272379082,0.421467855979837));
#84768=CARTESIAN_POINT('Ctrl Pts',(15.8338595608591,-2.3768481031062,0.416221830938508));
#84769=CARTESIAN_POINT('Ctrl Pts',(15.7544828038383,-2.40178307694768,0.410975805897177));
#84770=CARTESIAN_POINT('Ctrl Pts',(15.6751308057191,-2.42671027316528,0.405731417176377));
#84771=CARTESIAN_POINT('Ctrl Pts',(15.5945148520336,-2.44770936130754,0.400487028455576));
#84772=CARTESIAN_POINT('Ctrl Pts',(15.5130577907785,-2.46466589080985,0.395242639734777));
#84773=CARTESIAN_POINT('Ctrl Pts',(15.4316017771907,-2.48162220222423,0.389998318465158));
#84774=CARTESIAN_POINT('Ctrl Pts',(15.3493051279597,-2.49453596581245,0.38475399719554));
#84775=CARTESIAN_POINT('Ctrl Pts',(15.2666012599693,-2.50334376748036,0.379509675925921));
#84776=CARTESIAN_POINT('Ctrl Pts',(15.1832041834066,-2.51222539451785,0.374221397722384));
#84777=CARTESIAN_POINT('Ctrl Pts',(15.0993934998851,-2.51693183770499,0.368933119518846));
#84778=CARTESIAN_POINT('Ctrl Pts',(15.0156174689234,-2.51745155756063,0.363644841315309));
#84779=CARTESIAN_POINT('Ctrl Pts',(14.9324177135075,-2.51796770238603,0.358392939929495));
#84780=CARTESIAN_POINT('Ctrl Pts',(14.8492525967313,-2.51435462410235,0.353141038543681));
#84781=CARTESIAN_POINT('Ctrl Pts',(14.7665580024741,-2.50665336330956,0.347889137157867));
#84782=CARTESIAN_POINT('Ctrl Pts',(14.6830042433276,-2.49887208939213,0.342582670545468));
#84783=CARTESIAN_POINT('Ctrl Pts',(14.5999313168712,-2.48691725938727,0.337276203933069));
#84784=CARTESIAN_POINT('Ctrl Pts',(14.5177784320523,-2.47088417563553,0.33196973732067));
#84785=CARTESIAN_POINT('Ctrl Pts',(14.4356255472334,-2.45485109188379,0.326663270708271));
#84786=CARTESIAN_POINT('Ctrl Pts',(14.3543931525699,-2.43473992962642,0.321356804095871));
#84787=CARTESIAN_POINT('Ctrl Pts',(14.2745031108374,-2.41069710121685,0.316050337483472));
#84788=CARTESIAN_POINT('Ctrl Pts',(14.1961598457118,-2.38711977368503,0.310846611065516));
#84789=CARTESIAN_POINT('Ctrl Pts',(14.1188068158017,-2.35967105367289,0.305642884647561));
#84790=CARTESIAN_POINT('Ctrl Pts',(14.0428593314625,-2.32845184417279,0.300439158229605));
#84791=CARTESIAN_POINT('Ctrl Pts',(13.9670205221751,-2.29727730697799,0.295242877946866));
#84792=CARTESIAN_POINT('Ctrl Pts',(13.892583697609,-2.26234316820717,0.290046597664128));
#84793=CARTESIAN_POINT('Ctrl Pts',(13.819949844129,-2.22380032368664,0.284850317381388));
#84794=CARTESIAN_POINT('Ctrl Pts',(13.7460845119215,-2.18460400023237,0.27956593618807));
#84795=CARTESIAN_POINT('Ctrl Pts',(13.6740843350892,-2.14167559289604,0.274281554994751));
#84796=CARTESIAN_POINT('Ctrl Pts',(13.6043504961369,-2.09522521757605,0.268997173801433));
#84797=CARTESIAN_POINT('Ctrl Pts',(13.5358982830545,-2.04962854547354,0.263809913313728));
#84798=CARTESIAN_POINT('Ctrl Pts',(13.4696302129777,-2.00063854734632,0.258622652826023));
#84799=CARTESIAN_POINT('Ctrl Pts',(13.4058998011075,-1.94849962943049,0.253435392338318));
#84800=CARTESIAN_POINT('Ctrl Pts',(13.3421877949375,-1.89637576952653,0.24824962996053));
#84801=CARTESIAN_POINT('Ctrl Pts',(13.2810123569752,-1.84110509297578,0.24306386758274));
#84802=CARTESIAN_POINT('Ctrl Pts',(13.2226950380091,-1.78297316919876,0.237878105204951));
#84803=CARTESIAN_POINT('Ctrl Pts',(13.1643761279054,-1.7248396593424,0.232692201338114));
#84804=CARTESIAN_POINT('Ctrl Pts',(13.1089158246076,-1.6638450808606,0.227506297471279));
#84805=CARTESIAN_POINT('Ctrl Pts',(13.0565987251675,-1.60031176180751,0.222320393604442));
#84806=CARTESIAN_POINT('Ctrl Pts',(13.0025461151334,-1.53467085748167,0.216962458199217));
#84807=CARTESIAN_POINT('Ctrl Pts',(12.951849267774,-1.46632022224946,0.211604522793991));
#84808=CARTESIAN_POINT('Ctrl Pts',(12.9047754075953,-1.39565044240401,0.206246587388766));
#84809=CARTESIAN_POINT('Ctrl Pts',(12.859136809538,-1.32713535430808,0.201052013171835));
#84810=CARTESIAN_POINT('Ctrl Pts',(12.8169036271155,-1.2564409598805,0.195857438954905));
#84811=CARTESIAN_POINT('Ctrl Pts',(12.778272975014,-1.18394901767212,0.190662864737975));
#84812=CARTESIAN_POINT('Ctrl Pts',(12.737820013046,-1.10803743912983,0.185223248738602));
#84813=CARTESIAN_POINT('Ctrl Pts',(12.7013180887242,-1.03015508091847,0.179783632739229));
#84814=CARTESIAN_POINT('Ctrl Pts',(12.6689364767625,-0.950762378637098,
0.174344016739856));
#84815=CARTESIAN_POINT('Ctrl Pts',(12.6365548648009,-0.871369676355722,
0.168904400740483));
#84816=CARTESIAN_POINT('Ctrl Pts',(12.6082936708023,-0.790467209915332,
0.163464784741111));
#84817=CARTESIAN_POINT('Ctrl Pts',(12.5842615716475,-0.708529530634442,
0.158025168741738));
#84818=CARTESIAN_POINT('Ctrl Pts',(12.5533439584859,-0.603115623382605,
0.151027030870664));
#84819=CARTESIAN_POINT('Ctrl Pts',(12.5293259598537,-0.495662097745632,
0.144028892999589));
#84820=CARTESIAN_POINT('Ctrl Pts',(12.5124152219306,-0.386947311552094,
0.137030755128515));
#84821=CARTESIAN_POINT('Ctrl Pts',(12.4959203534034,-0.280906042781049,
0.130204715682857));
#84822=CARTESIAN_POINT('Ctrl Pts',(12.4861873976345,-0.173664393537871,
0.1233786762372));
#84823=CARTESIAN_POINT('Ctrl Pts',(12.4833644063538,-0.0659661943196923,
0.116552636791542));
#84824=CARTESIAN_POINT('Ctrl Pts',(12.4828174506086,-0.0450996230298626,
0.115230088784667));
#84825=CARTESIAN_POINT('Ctrl Pts',(12.482529752956,-0.0242159895210024,
0.113907540777792));
#84826=CARTESIAN_POINT('Ctrl Pts',(12.4825021902374,-0.00332081924700182,
0.112584992770917));
#84827=CARTESIAN_POINT('Ctrl Pts',(12.4825022739887,-0.00338371508027381,
0.111635339680572));
#84828=CARTESIAN_POINT('Ctrl Pts',(12.4823675913716,0.0968206975641423,
0.104704442175761));
#84829=CARTESIAN_POINT('Ctrl Pts',(12.4882156443794,0.196951503677597,0.0978501008475581));
#84830=CARTESIAN_POINT('Ctrl Pts',(12.5069280030255,0.354740533776522,0.0872189342832773));
#84831=CARTESIAN_POINT('Ctrl Pts',(12.5158729127969,0.41274968462613,0.0833463613678871));
#84832=CARTESIAN_POINT('Ctrl Pts',(12.5352006621777,0.514367388117053,0.0766211706808165));
#84833=CARTESIAN_POINT('Ctrl Pts',(12.5447353595632,0.558108879288796,0.0737456119838154));
#84834=CARTESIAN_POINT('Ctrl Pts',(12.5648857957226,0.639992447749824,0.068391451530109));
#84835=CARTESIAN_POINT('Ctrl Pts',(12.575244442901,0.67818306066525,0.0659062655892474));
#84836=CARTESIAN_POINT('Ctrl Pts',(12.601878361662,0.76794651483863,0.0600832067456229));
#84837=CARTESIAN_POINT('Ctrl Pts',(12.6189236479036,0.819271141012264,0.0567683063242814));
#84838=CARTESIAN_POINT('Ctrl Pts',(12.6379294358328,0.870878727335478,0.053434295920754));
#84839=CARTESIAN_POINT('Ctrl Pts',(12.6382499872001,0.871747661199217,0.0533781597321072));
#84840=CARTESIAN_POINT('Ctrl Pts',(12.6385710118969,0.872616401488192,0.0533220355972284));
#84841=CARTESIAN_POINT('Ctrl Pts',(12.6385711154041,0.872616681594026,0.329758541657824));
#84842=CARTESIAN_POINT('Ctrl Pts',(12.604742168923,0.781070584618255,0.336428593169256));
#84843=CARTESIAN_POINT('Ctrl Pts',(12.5762486803767,0.687589650928952,0.343201336130416));
#84844=CARTESIAN_POINT('Ctrl Pts',(12.5304438206718,0.49848259594701,0.356611734577644));
#84845=CARTESIAN_POINT('Ctrl Pts',(12.5130895120278,0.403077620634501,0.363235540803975));
#84846=CARTESIAN_POINT('Ctrl Pts',(12.4927843145818,0.237758076097962,0.374383878584141));
#84847=CARTESIAN_POINT('Ctrl Pts',(12.4871647804762,0.168285650935039,0.3789716204258));
#84848=CARTESIAN_POINT('Ctrl Pts',(12.4829009703236,0.0595741557933482,
0.38599867336799));
#84849=CARTESIAN_POINT('Ctrl Pts',(12.4822790884716,0.0204523564103614,
0.38849716768747));
#84850=CARTESIAN_POINT('Ctrl Pts',(12.4828363091139,-0.0546826133986007,
0.393241445280683));
#84851=CARTESIAN_POINT('Ctrl Pts',(12.4838761255024,-0.0906868069017626,
0.395490986094705));
#84852=CARTESIAN_POINT('Ctrl Pts',(12.4882219026152,-0.176955756085008,
0.400830467162363));
#84853=CARTESIAN_POINT('Ctrl Pts',(12.4922644730078,-0.227168665815338,
0.403896861580725));
#84854=CARTESIAN_POINT('Ctrl Pts',(12.5189888492276,-0.468374960492772,
0.418480888627921));
#84855=CARTESIAN_POINT('Ctrl Pts',(12.5619977837427,-0.656460864068143,
0.429352037481086));
#84856=CARTESIAN_POINT('Ctrl Pts',(12.6498945262017,-0.905518527406008,
0.444598126285946));
#84857=CARTESIAN_POINT('Ctrl Pts',(12.676668289437,-0.972156439160653,0.448774464393134));
#84858=CARTESIAN_POINT('Ctrl Pts',(12.7259518357056,-1.08110880071214,0.455901856630064));
#84859=CARTESIAN_POINT('Ctrl Pts',(12.7468880072878,-1.1240894107314,0.458794903871633));
#84860=CARTESIAN_POINT('Ctrl Pts',(12.7799106944797,-1.18724928464749,0.463207055548019));
#84861=CARTESIAN_POINT('Ctrl Pts',(12.7910780798627,-1.2078995154515,0.464676033404665));
#84862=CARTESIAN_POINT('Ctrl Pts',(12.8126780674132,-1.24653976343559,0.467480689348058));
#84863=CARTESIAN_POINT('Ctrl Pts',(12.8230477174689,-1.26456208154167,0.468812668418927));
#84864=CARTESIAN_POINT('Ctrl Pts',(12.8507318399904,-1.3113270067994,0.472328119495822));
#84865=CARTESIAN_POINT('Ctrl Pts',(12.8683995321564,-1.33985496631125,0.474531859886888));
#84866=CARTESIAN_POINT('Ctrl Pts',(12.9436419208379,-1.45609228270961,0.48373188173108));
#84867=CARTESIAN_POINT('Ctrl Pts',(13.006098355106,-1.54050839470345,0.4909391503102));
#84868=CARTESIAN_POINT('Ctrl Pts',(13.1555257252679,-1.71810983826825,0.50695408024129));
#84869=CARTESIAN_POINT('Ctrl Pts',(13.2446846144548,-1.80910448024971,0.515748458881631));
#84870=CARTESIAN_POINT('Ctrl Pts',(13.3836516743425,-1.93094317007374,0.528209632277172));
#84871=CARTESIAN_POINT('Ctrl Pts',(13.4282514391545,-1.96741726238998,0.53204723959394));
#84872=CARTESIAN_POINT('Ctrl Pts',(13.5134539725199,-2.03234829268834,0.539080395520705));
#84873=CARTESIAN_POINT('Ctrl Pts',(13.5537211831046,-2.06119790882775,0.542289072819348));
#84874=CARTESIAN_POINT('Ctrl Pts',(13.624823211575,-2.10902892129922,0.547763646985517));
#84875=CARTESIAN_POINT('Ctrl Pts',(13.6552634107837,-2.12856710377433,0.550049780318644));
#84876=CARTESIAN_POINT('Ctrl Pts',(13.7202664698996,-2.16833835850625,0.554816634319897));
#84877=CARTESIAN_POINT('Ctrl Pts',(13.7549125412612,-2.18841646998942,0.557291296145527));
#84878=CARTESIAN_POINT('Ctrl Pts',(13.8549960906644,-2.24327030812304,0.564267624468481));
#84879=CARTESIAN_POINT('Ctrl Pts',(13.9215116740373,-2.27599648112374,0.568698738434944));
#84880=CARTESIAN_POINT('Ctrl Pts',(14.1464490997509,-2.37458792540086,0.58316495893481));
#84881=CARTESIAN_POINT('Ctrl Pts',(14.310136774633,-2.42720093368182,0.592842289956259));
#84882=CARTESIAN_POINT('Ctrl Pts',(14.5335679095169,-2.47456774938233,0.606150784004289));
#84883=CARTESIAN_POINT('Ctrl Pts',(14.5896170245296,-2.48447772146856,0.609500801979481));
#84884=CARTESIAN_POINT('Ctrl Pts',(14.6866139918683,-2.49825586132311,0.615388697619319));
#84885=CARTESIAN_POINT('Ctrl Pts',(14.727410285451,-2.50303566919724,0.617892425804689));
#84886=CARTESIAN_POINT('Ctrl Pts',(14.7906346651955,-2.50887930949783,0.621839634283163));
#84887=CARTESIAN_POINT('Ctrl Pts',(14.8129923700133,-2.51064479590491,0.623248372960291));
#84888=CARTESIAN_POINT('Ctrl Pts',(14.8572913051837,-2.51354791076056,0.626070380636404));
#84889=CARTESIAN_POINT('Ctrl Pts',(14.8792296089908,-2.51469745299752,0.627482973797375));
#84890=CARTESIAN_POINT('Ctrl Pts',(14.9399378175018,-2.51708230927156,0.631428394811506));
#84891=CARTESIAN_POINT('Ctrl Pts',(14.9787243377328,-2.51770883705923,0.633990149912726));
#84892=CARTESIAN_POINT('Ctrl Pts',(15.1890960338925,-2.51624582516177,0.648054101231258));
#84893=CARTESIAN_POINT('Ctrl Pts',(15.3601070881016,-2.49751301650272,0.660062135035727));
#84894=CARTESIAN_POINT('Ctrl Pts',(15.6445667064522,-2.43651022208841,0.679997661878572));
#84895=CARTESIAN_POINT('Ctrl Pts',(15.7593388291444,-2.40321855648549,0.688038260867876));
#84896=CARTESIAN_POINT('Ctrl Pts',(15.913635752508,-2.34629695965286,0.698772286654597));
#84897=CARTESIAN_POINT('Ctrl Pts',(15.955517676486,-2.32955491627493,0.701679248999914));
#84898=CARTESIAN_POINT('Ctrl Pts',(16.0297211530866,-2.2975543236392,0.706821549061802));
#84899=CARTESIAN_POINT('Ctrl Pts',(16.0622094237457,-2.28271611763231,0.709070190562082));
#84900=CARTESIAN_POINT('Ctrl Pts',(16.1326496108087,-2.24871466226891,0.713944562186402));
#84901=CARTESIAN_POINT('Ctrl Pts',(16.1704543985394,-2.22927109277121,0.716559855515438));
#84902=CARTESIAN_POINT('Ctrl Pts',(16.2886176974978,-2.16466284075243,0.724750554638095));
#84903=CARTESIAN_POINT('Ctrl Pts',(16.3670003538676,-2.1160371565166,0.730205426687023));
#84904=CARTESIAN_POINT('Ctrl Pts',(16.5803356849875,-1.96687891523612,0.745378402081721));
#84905=CARTESIAN_POINT('Ctrl Pts',(16.7081202263537,-1.85698519904677,0.754846285568924));
#84906=CARTESIAN_POINT('Ctrl Pts',(16.8681809198738,-1.68873220738179,0.768504443517352));
#84907=CARTESIAN_POINT('Ctrl Pts',(16.9105750877766,-1.64061510531638,0.772334718895013));
#84908=CARTESIAN_POINT('Ctrl Pts',(16.9677402874505,-1.57050920308719,0.777897461646474));
#84909=CARTESIAN_POINT('Ctrl Pts',(16.9840746337631,-1.54982215423057,0.779536892014463));
#84910=CARTESIAN_POINT('Ctrl Pts',(17.0124992674903,-1.51263714107904,0.782487836536395));
#84911=CARTESIAN_POINT('Ctrl Pts',(17.0247183876664,-1.4962418862075,0.78379079890158));
#84912=CARTESIAN_POINT('Ctrl Pts',(17.0536569346944,-1.45640934590498,0.786960386040286));
#84913=CARTESIAN_POINT('Ctrl Pts',(17.0701758237359,-1.43283176793966,0.788839073800151));
#84914=CARTESIAN_POINT('Ctrl Pts',(17.1400700340562,-1.32933876117576,0.797078676662087));
#84915=CARTESIAN_POINT('Ctrl Pts',(17.1892454009603,-1.24669264688285,0.803638388431322));
#84916=CARTESIAN_POINT('Ctrl Pts',(17.3291773256558,-0.977590286218625,
0.824520220170332));
#84917=CARTESIAN_POINT('Ctrl Pts',(17.4017334207819,-0.78259477751762,0.838889351353303));
#84918=CARTESIAN_POINT('Ctrl Pts',(17.4595214645086,-0.538908338722196,
0.855299759443689));
#84919=CARTESIAN_POINT('Ctrl Pts',(17.4683970460975,-0.49667336057499,0.858094428341065));
#84920=CARTESIAN_POINT('Ctrl Pts',(17.4827343463794,-0.418515013268738,
0.863178213122588));
#84921=CARTESIAN_POINT('Ctrl Pts',(17.4885125151201,-0.382662169774976,
0.865476654945772));
#84922=CARTESIAN_POINT('Ctrl Pts',(17.4989021121014,-0.307937768290788,
0.87020202856891));
#84923=CARTESIAN_POINT('Ctrl Pts',(17.503386770235,-0.269058318328164,0.872624413454042));
#84924=CARTESIAN_POINT('Ctrl Pts',(17.5132544936217,-0.161543007546097,
0.879235048842481));
#84925=CARTESIAN_POINT('Ctrl Pts',(17.5167320423799,-0.0927647962934042,
0.883364556165057));
#84926=CARTESIAN_POINT('Ctrl Pts',(17.5182872636156,0.0708697245805634,
0.893035066516843));
#84927=CARTESIAN_POINT('Ctrl Pts',(17.5138330712852,0.165644200625899,0.898511535287157));
#84928=CARTESIAN_POINT('Ctrl Pts',(17.4872184688903,0.422022059387645,0.913342091520537));
#84929=CARTESIAN_POINT('Ctrl Pts',(17.4546991609139,0.582063159446605,0.92260663816126));
#84930=CARTESIAN_POINT('Ctrl Pts',(17.3980007661231,0.767027995927043,0.934405086453369));
#84931=CARTESIAN_POINT('Ctrl Pts',(17.3885164728805,0.796070651897628,0.936291480449378));
#84932=CARTESIAN_POINT('Ctrl Pts',(17.3717559080207,0.84439598649696,0.939498500985057));
#84933=CARTESIAN_POINT('Ctrl Pts',(17.3647673133553,0.863774386117301,0.940803399676279));
#84934=CARTESIAN_POINT('Ctrl Pts',(17.3487097700778,0.906643567050734,0.943734874261015));
#84935=CARTESIAN_POINT('Ctrl Pts',(17.3395255523565,0.93008613090563,0.945367338722355));
#84936=CARTESIAN_POINT('Ctrl Pts',(17.3079519772803,1.00724918952326,0.950829516955083));
#84937=CARTESIAN_POINT('Ctrl Pts',(17.2840526845121,1.06032803391536,0.954730699734162));
#84938=CARTESIAN_POINT('Ctrl Pts',(17.2142483121891,1.20202517595606,0.96545559880941));
#84939=CARTESIAN_POINT('Ctrl Pts',(17.1648787842151,1.28882069783537,0.972363724015122));
#84940=CARTESIAN_POINT('Ctrl Pts',(17.0305639094022,1.49536326497365,0.989362248487098));
#84941=CARTESIAN_POINT('Ctrl Pts',(16.9400430366759,1.61106945679474,0.999377773926579));
#84942=CARTESIAN_POINT('Ctrl Pts',(16.8050749328937,1.75559736152835,1.01238635017896));
#84943=CARTESIAN_POINT('Ctrl Pts',(16.7690661105209,1.79187703851152,1.01570290337216));
#84944=CARTESIAN_POINT('Ctrl Pts',(16.7056223531936,1.85201977267528,1.02129471491247));
#84945=CARTESIAN_POINT('Ctrl Pts',(16.6787306126256,1.87642974904936,1.02359290561397));
#84946=CARTESIAN_POINT('Ctrl Pts',(16.6216645485043,1.92602019926174,1.0283274503941));
#84947=CARTESIAN_POINT('Ctrl Pts',(16.5914097477963,1.95109328277504,1.03075903632243));
#84948=CARTESIAN_POINT('Ctrl Pts',(16.5059489382381,2.01860621182805,1.0374259745998));
#84949=CARTESIAN_POINT('Ctrl Pts',(16.4495491216316,2.05948095589878,1.04160094114627));
#84950=CARTESIAN_POINT('Ctrl Pts',(16.3110329376754,2.15135487339746,1.0514192140602));
#84951=CARTESIAN_POINT('Ctrl Pts',(16.2275336786949,2.20006765597637,1.05699500218606));
#84952=CARTESIAN_POINT('Ctrl Pts',(16.0000357708245,2.31579438345819,1.07168057128616));
#84953=CARTESIAN_POINT('Ctrl Pts',(15.8521664388527,2.37418947103169,1.08071639932309));
#84954=CARTESIAN_POINT('Ctrl Pts',(15.6700216152687,2.42689901065738,1.09227268039386));
#84955=CARTESIAN_POINT('Ctrl Pts',(15.6400801596817,2.43496713687307,1.09418616400736));
#84956=CARTESIAN_POINT('Ctrl Pts',(15.5899448238934,2.44748822419849,1.09742476684954));
#84957=CARTESIAN_POINT('Ctrl Pts',(15.5698318104211,2.45224900477874,1.09873341705746));
#84958=CARTESIAN_POINT('Ctrl Pts',(15.5253055319549,2.46221104603106,1.10165409204259));
#84959=CARTESIAN_POINT('Ctrl Pts',(15.5008714141582,2.46729747813692,1.10327157696218));
#84960=CARTESIAN_POINT('Ctrl Pts',(15.4207418694658,2.48273872448992,1.10861519571037));
#84961=CARTESIAN_POINT('Ctrl Pts',(15.3647749790611,2.49157651365271,1.1124088341832));
#84962=CARTESIAN_POINT('Ctrl Pts',(15.2142058107458,2.51017151938912,1.12270002374003));
#84963=CARTESIAN_POINT('Ctrl Pts',(15.1192682563172,2.51646956154645,1.12927538876171));
#84964=CARTESIAN_POINT('Ctrl Pts',(14.8705182732249,2.5188613990881,1.1464457567487));
#84965=CARTESIAN_POINT('Ctrl Pts',(14.716998759213,2.50626229996753,1.15696458653425));
#84966=CARTESIAN_POINT('Ctrl Pts',(14.5153664340098,2.47093796125292,1.1704286939267));
#84967=CARTESIAN_POINT('Ctrl Pts',(14.4654379187208,2.46061945326338,1.17373625719563));
#84968=CARTESIAN_POINT('Ctrl Pts',(14.3805596809748,2.44037220863774,1.17931731211773));
#84969=CARTESIAN_POINT('Ctrl Pts',(14.3454500820677,2.43119054226346,1.18161353750134));
#84970=CARTESIAN_POINT('Ctrl Pts',(14.272739853022,2.41048634656855,1.18634756077971));
#84971=CARTESIAN_POINT('Ctrl Pts',(14.2351858625547,2.3988354157261,1.18878051434161));
#84972=CARTESIAN_POINT('Ctrl Pts',(14.1317285603217,2.36406155072531,1.19546108494195));
#84973=CARTESIAN_POINT('Ctrl Pts',(14.0664893755381,2.33906850123898,1.199647805954));
#84974=CARTESIAN_POINT('Ctrl Pts',(13.9132596500795,2.27293234662019,1.20950408643882));
#84975=CARTESIAN_POINT('Ctrl Pts',(13.8264452391703,2.22934894972906,1.21510525830822));
#84976=CARTESIAN_POINT('Ctrl Pts',(13.6056551196452,2.10202570493024,1.22976722969446));
#84977=CARTESIAN_POINT('Ctrl Pts',(13.4766802936759,2.01052109272765,1.23875710519235));
#84978=CARTESIAN_POINT('Ctrl Pts',(13.3335645145612,1.88726430825271,1.25026581253358));
#84979=CARTESIAN_POINT('Ctrl Pts',(13.3103747679457,1.86653158702515,1.25218494018752));
#84980=CARTESIAN_POINT('Ctrl Pts',(13.2724220956371,1.83131325492163,1.25542943166501));
#84981=CARTESIAN_POINT('Ctrl Pts',(13.2574431634037,1.81706612314704,1.25673814211022));
#84982=CARTESIAN_POINT('Ctrl Pts',(13.2248234303855,1.78526567765905,1.25965390177186));
#84983=CARTESIAN_POINT('Ctrl Pts',(13.2072657831394,1.76763381495852,1.26126629411108));
#84984=CARTESIAN_POINT('Ctrl Pts',(13.1509453397864,1.70937304890351,1.26657172570376));
#84985=CARTESIAN_POINT('Ctrl Pts',(13.1132820308486,1.667709116314,1.27033104088656));
#84986=CARTESIAN_POINT('Ctrl Pts',(13.0166235947319,1.55331539048402,1.28048698565395));
#84987=CARTESIAN_POINT('Ctrl Pts',(12.9602391315948,1.47849418169828,1.28695941847178));
#84988=CARTESIAN_POINT('Ctrl Pts',(12.8213037578709,1.27100558895069,1.30419718779099));
#84989=CARTESIAN_POINT('Ctrl Pts',(12.7466933591226,1.13348771233836,1.31488680045159));
#84990=CARTESIAN_POINT('Ctrl Pts',(12.6687435921548,0.951221329104753,1.32792405305236));
#84991=CARTESIAN_POINT('Ctrl Pts',(12.6531633245514,0.912105356742518,1.33066211520459));
#84992=CARTESIAN_POINT('Ctrl Pts',(12.6385710124998,0.872616403119952,1.33336808075876));
#84993=CARTESIAN_POINT('Origin',(15.,0.,3.));
#84994=CARTESIAN_POINT('',(12.6385710877721,0.872616606817863,2.33071866803842));
#84995=CARTESIAN_POINT('',(12.6385710119932,0.872616401748851,2.05625948175199));
#84996=CARTESIAN_POINT('',(12.6385710119932,0.872616401748847,3.));
#84997=CARTESIAN_POINT('',(12.482500077493,0.000624641887345871,1.11258330254392));
#84998=CARTESIAN_POINT('Ctrl Pts',(12.6385710119932,0.872616401748851,2.05625948175199));
#84999=CARTESIAN_POINT('Ctrl Pts',(12.6420817776151,0.882117052542451,2.05561538571552));
#85000=CARTESIAN_POINT('Ctrl Pts',(12.6456495005229,0.891595491259146,2.05497128967904));
#85001=CARTESIAN_POINT('Ctrl Pts',(12.6492738991091,0.901051079900762,2.05432719364257));
#85002=CARTESIAN_POINT('Ctrl Pts',(12.6788539027848,0.978221495935984,2.04907049720776));
#85003=CARTESIAN_POINT('Ctrl Pts',(12.7122922497419,1.05407532159594,2.04381380077295));
#85004=CARTESIAN_POINT('Ctrl Pts',(12.7494510805673,1.12820025316438,2.03855710433814));
#85005=CARTESIAN_POINT('Ctrl Pts',(12.7865574588937,1.20222055178812,2.03330782812775));
#85006=CARTESIAN_POINT('Ctrl Pts',(12.8273736844179,1.27451639508405,2.02805855191736));
#85007=CARTESIAN_POINT('Ctrl Pts',(12.8717132992482,1.34469400586271,2.02280927570697));
#85008=CARTESIAN_POINT('Ctrl Pts',(12.9162375548247,1.41516385297371,2.01753814025671));
#85009=CARTESIAN_POINT('Ctrl Pts',(12.9643144432659,1.48349734572078,2.01226700480646));
#85010=CARTESIAN_POINT('Ctrl Pts',(13.0157077482685,1.54931936982614,2.0069958693562));
#85011=CARTESIAN_POINT('Ctrl Pts',(13.0667971665732,1.61475219075496,2.0017559019335));
#85012=CARTESIAN_POINT('Ctrl Pts',(13.1211636033577,1.67770279408537,1.9965159345108));
#85013=CARTESIAN_POINT('Ctrl Pts',(13.1785317860396,1.73783192384415,1.9912759670881));
#85014=CARTESIAN_POINT('Ctrl Pts',(13.2358812709124,1.79794145592808,1.98603770750948));
#85015=CARTESIAN_POINT('Ctrl Pts',(13.296230240507,1.85523100749621,1.98079944793085));
#85016=CARTESIAN_POINT('Ctrl Pts',(13.3592647967259,1.90939630321658,1.97556118835222));
#85017=CARTESIAN_POINT('Ctrl Pts',(13.4222977911159,1.96356025686479,1.97032305856375));
#85018=CARTESIAN_POINT('Ctrl Pts',(13.4880158893933,2.01459980887977,1.96508492877528));
#85019=CARTESIAN_POINT('Ctrl Pts',(13.5560712294798,2.06225021655082,1.95984679898681));
#85020=CARTESIAN_POINT('Ctrl Pts',(13.6248706131303,2.11042158229963,1.95455140114631));
#85021=CARTESIAN_POINT('Ctrl Pts',(13.6960582729743,2.15512895369361,1.94925600330581));
#85022=CARTESIAN_POINT('Ctrl Pts',(13.7692452867183,2.19614414047322,1.94396060546531));
#85023=CARTESIAN_POINT('Ctrl Pts',(13.8417443785649,2.23677380468988,1.93871498175746));
#85024=CARTESIAN_POINT('Ctrl Pts',(13.9162049509551,2.27378025032919,1.93346935804961));
#85025=CARTESIAN_POINT('Ctrl Pts',(13.9922263886963,2.30698907634168,1.92822373434176));
#85026=CARTESIAN_POINT('Ctrl Pts',(14.0693298429917,2.34067056507355,1.92290344943494));
#85027=CARTESIAN_POINT('Ctrl Pts',(14.1480384835152,2.37044530737412,1.91758316452811));
#85028=CARTESIAN_POINT('Ctrl Pts',(14.2279176382871,2.39618343970819,1.91226287962129));
#85029=CARTESIAN_POINT('Ctrl Pts',(14.307796793059,2.42192157204227,1.90694259471447));
#85030=CARTESIAN_POINT('Ctrl Pts',(14.3888459741961,2.4436230300173,1.90162230980764));
#85031=CARTESIAN_POINT('Ctrl Pts',(14.470620895541,2.46121189940286,1.89630202490082));
#85032=CARTESIAN_POINT('Ctrl Pts',(14.5514188943887,2.47859064370457,1.8910452986735));
#85033=CARTESIAN_POINT('Ctrl Pts',(14.6332217605528,2.49201832667614,1.88578857244619));
#85034=CARTESIAN_POINT('Ctrl Pts',(14.7156088295062,2.50138519867396,1.88053184621887));
#85035=CARTESIAN_POINT('Ctrl Pts',(14.7978796096309,2.51073884939097,1.8752825398275));
#85036=CARTESIAN_POINT('Ctrl Pts',(14.8807325002353,2.51604302277806,1.87003323343612));
#85037=CARTESIAN_POINT('Ctrl Pts',(14.9637358079743,2.5172387964547,1.86478392704475));
#85038=CARTESIAN_POINT('Ctrl Pts',(15.0470841635553,2.51843954100706,1.85951279909118));
#85039=CARTESIAN_POINT('Ctrl Pts',(15.1305837295089,2.51549755083754,1.85424167113761));
#85040=CARTESIAN_POINT('Ctrl Pts',(15.2137912737799,2.50840577683427,1.84897054318404));
#85041=CARTESIAN_POINT('Ctrl Pts',(15.2965074202738,2.50135588463405,1.8437305448664));
#85042=CARTESIAN_POINT('Ctrl Pts',(15.3789345204306,2.49020512748366,1.83849054654875));
#85043=CARTESIAN_POINT('Ctrl Pts',(15.4606380334944,2.47499875799936,1.83325054823111));
#85044=CARTESIAN_POINT('Ctrl Pts',(15.5423149204558,2.45979734407129,1.82801225756014));
#85045=CARTESIAN_POINT('Ctrl Pts',(15.6232682356974,2.44054302711176,1.82277396688917));
#85046=CARTESIAN_POINT('Ctrl Pts',(15.7030716394199,2.4173325215707,1.81753567621821));
#85047=CARTESIAN_POINT('Ctrl Pts',(15.7828730681785,2.39412259044014,1.81229751518376));
#85048=CARTESIAN_POINT('Ctrl Pts',(15.8615241995453,2.36695679520795,1.80705935414931));
#85049=CARTESIAN_POINT('Ctrl Pts',(15.9386132538092,2.33598189414508,1.80182119311486));
#85050=CARTESIAN_POINT('Ctrl Pts',(16.0165441155426,2.30466874917293,1.79652583170188));
#85051=CARTESIAN_POINT('Ctrl Pts',(16.0928781233521,2.26946296278871,1.7912304702889));
#85052=CARTESIAN_POINT('Ctrl Pts',(16.1672117001879,2.23056564506508,1.78593510887592));
#85053=CARTESIAN_POINT('Ctrl Pts',(16.2408475238947,2.19203344800837,1.78068945386955));
#85054=CARTESIAN_POINT('Ctrl Pts',(16.3125199438519,2.14987902217788,1.77544379886318));
#85055=CARTESIAN_POINT('Ctrl Pts',(16.381864034631,2.10434266216157,1.7701981438568));
#85056=CARTESIAN_POINT('Ctrl Pts',(16.4521937541547,2.05815906681708,1.76487792924052));
#85057=CARTESIAN_POINT('Ctrl Pts',(16.5201280402855,2.00849693418549,1.75955771462424));
#85058=CARTESIAN_POINT('Ctrl Pts',(16.5853206882403,1.95564939737096,1.75423750000795));
#85059=CARTESIAN_POINT('Ctrl Pts',(16.650513336195,1.90280186055643,1.74891728539167));
#85060=CARTESIAN_POINT('Ctrl Pts',(16.7129640255581,1.84676929299895,1.74359707077538));
#85061=CARTESIAN_POINT('Ctrl Pts',(16.7723664851078,1.78788234860868,1.7382768561591));
#85062=CARTESIAN_POINT('Ctrl Pts',(16.831058252292,1.72969992894892,1.73302029271045));
#85063=CARTESIAN_POINT('Ctrl Pts',(16.8869896882907,1.66851764379647,1.7277637292618));
#85064=CARTESIAN_POINT('Ctrl Pts',(16.9398390787621,1.60462786916696,1.72250716581314));
#85065=CARTESIAN_POINT('Ctrl Pts',(16.992613866375,1.54082828214002,1.71725802259501));
#85066=CARTESIAN_POINT('Ctrl Pts',(17.0423149588083,1.47432914965126,1.71200887937687));
#85067=CARTESIAN_POINT('Ctrl Pts',(17.0886571892918,1.40545985201274,1.70675973615873));
#85068=CARTESIAN_POINT('Ctrl Pts',(17.135193872432,1.33630157782419,1.70148856746117));
#85069=CARTESIAN_POINT('Ctrl Pts',(17.1783431060488,1.26475353319337,1.69621739876362));
#85070=CARTESIAN_POINT('Ctrl Pts',(17.2178568409913,1.19118314413369,1.69094623006606));
#85071=CARTESIAN_POINT('Ctrl Pts',(17.2571356951225,1.11805007826535,1.68570639468543));
#85072=CARTESIAN_POINT('Ctrl Pts',(17.2928219309709,1.04291905461402,1.6804665593048));
#85073=CARTESIAN_POINT('Ctrl Pts',(17.3247160849578,0.966178748647717,1.67522672392417));
#85074=CARTESIAN_POINT('Ctrl Pts',(17.3565998474769,0.889463445521055,1.6699885957398));
#85075=CARTESIAN_POINT('Ctrl Pts',(17.384693805145,0.811140326937861,1.66475046755544));
#85076=CARTESIAN_POINT('Ctrl Pts',(17.4088460792308,0.731619311236649,1.65951233937107));
#85077=CARTESIAN_POINT('Ctrl Pts',(17.4329977586653,0.652100253416509,1.65427434015428));
#85078=CARTESIAN_POINT('Ctrl Pts',(17.4532078144991,0.571383798667101,1.64903634093748));
#85079=CARTESIAN_POINT('Ctrl Pts',(17.4693742390353,0.489895006699017,1.64379834172068));
#85080=CARTESIAN_POINT('Ctrl Pts',(17.4857183007786,0.407510813192036,1.63850278719541));
#85081=CARTESIAN_POINT('Ctrl Pts',(17.4979292111129,0.324337673737048,1.63320723267013));
#85082=CARTESIAN_POINT('Ctrl Pts',(17.5059549605607,0.24082355707255,1.62791167814485));
#85083=CARTESIAN_POINT('Ctrl Pts',(17.5139048438455,0.158098886382231,1.62266618167404));
#85084=CARTESIAN_POINT('Ctrl Pts',(17.5177483960051,0.0750401264698005,
1.61742068520324));
#85085=CARTESIAN_POINT('Ctrl Pts',(17.51748755506,-0.0079158144197794,1.61217518873243));
#85086=CARTESIAN_POINT('Ctrl Pts',(17.5172229802862,-0.0920592348065238,
1.60685460517992));
#85087=CARTESIAN_POINT('Ctrl Pts',(17.5127356050044,-0.176096377978873,
1.6015340216274));
#85088=CARTESIAN_POINT('Ctrl Pts',(17.5040818716157,-0.259577021798146,
1.59621343807489));
#85089=CARTESIAN_POINT('Ctrl Pts',(17.495428138227,-0.343057665617419,1.59089285452238));
#85090=CARTESIAN_POINT('Ctrl Pts',(17.4826081846109,-0.425981337446218,
1.58557227096986));
#85091=CARTESIAN_POINT('Ctrl Pts',(17.4657317156099,-0.507910776254469,
1.58025168741735));
#85092=CARTESIAN_POINT('Ctrl Pts',(17.4490575726161,-0.588857992050123,
1.57499489045586));
#85093=CARTESIAN_POINT('Ctrl Pts',(17.4283625190827,-0.669131702942927,
1.56973809349437));
#85094=CARTESIAN_POINT('Ctrl Pts',(17.4037157334411,-0.748302694641591,
1.56448129653287));
#85095=CARTESIAN_POINT('Ctrl Pts',(17.3791037409477,-0.827361922960895,
1.5592319204383));
#85096=CARTESIAN_POINT('Ctrl Pts',(17.3505512331481,-0.905321087546031,
1.55398254434372));
#85097=CARTESIAN_POINT('Ctrl Pts',(17.3181783479629,-0.981761374793338,
1.54873316824914));
#85098=CARTESIAN_POINT('Ctrl Pts',(17.2856714273941,-1.05851815231214,1.54346205785025));
#85099=CARTESIAN_POINT('Ctrl Pts',(17.2493125166114,-1.13374298531113,1.53819094745135));
#85100=CARTESIAN_POINT('Ctrl Pts',(17.2092738670235,-1.20702743568121,1.53291983705245));
#85101=CARTESIAN_POINT('Ctrl Pts',(17.1694710338388,-1.27988026121685,1.52767977201368));
#85102=CARTESIAN_POINT('Ctrl Pts',(17.1260319110588,-1.35081508884042,1.52243970697491));
#85103=CARTESIAN_POINT('Ctrl Pts',(17.0791731159878,-1.41945250140804,1.51719964193614));
#85104=CARTESIAN_POINT('Ctrl Pts',(17.0323296026566,-1.48806752972353,1.5119612858041));
#85105=CARTESIAN_POINT('Ctrl Pts',(16.9820688918041,-1.5543862505504,1.50672292967207));
#85106=CARTESIAN_POINT('Ctrl Pts',(16.9286513878899,-1.6180575002114,1.50148457354004));
#85107=CARTESIAN_POINT('Ctrl Pts',(16.8752352196017,-1.68172715786649,1.4962463483854));
#85108=CARTESIAN_POINT('Ctrl Pts',(16.8186627123708,-1.74274912342548,1.49100812323075));
#85109=CARTESIAN_POINT('Ctrl Pts',(16.7592341963719,-1.80080573419667,1.48576989807611));
#85110=CARTESIAN_POINT('Ctrl Pts',(16.6991583655349,-1.85949471656551,1.4804746164594));
#85111=CARTESIAN_POINT('Ctrl Pts',(16.636164261308,-1.91515300259753,1.4751793348427));
#85112=CARTESIAN_POINT('Ctrl Pts',(16.570598616877,-1.9674923721997,1.46988405322599));
#85113=CARTESIAN_POINT('Ctrl Pts',(16.5056466986456,-2.01934181994305,1.46463833801087));
#85114=CARTESIAN_POINT('Ctrl Pts',(16.4381715953401,-2.06793400260606,1.45939262279575));
#85115=CARTESIAN_POINT('Ctrl Pts',(16.3685403427349,-2.11303184554967,1.45414690758064));
#85116=CARTESIAN_POINT('Ctrl Pts',(16.2979221787682,-2.15876887810874,1.44882684276313));
#85117=CARTESIAN_POINT('Ctrl Pts',(16.2250866927709,-2.20091149619349,1.44350677794563));
#85118=CARTESIAN_POINT('Ctrl Pts',(16.1504416786233,-2.23926108216223,1.43818671312813));
#85119=CARTESIAN_POINT('Ctrl Pts',(16.0757966644757,-2.27761066813096,1.43286664831063));
#85120=CARTESIAN_POINT('Ctrl Pts',(15.9993425929955,-2.31216707934187,1.42754658349313));
#85121=CARTESIAN_POINT('Ctrl Pts',(15.9215054922675,-2.34278336124381,1.42222651867563));
#85122=CARTESIAN_POINT('Ctrl Pts',(15.8445922768582,-2.37303624403277,1.41696960022064));
#85123=CARTESIAN_POINT('Ctrl Pts',(15.766046716246,-2.39955299249558,1.41171268176565));
#85124=CARTESIAN_POINT('Ctrl Pts',(15.6862661453634,-2.42215710219798,1.40645576331066));
#85125=CARTESIAN_POINT('Ctrl Pts',(15.6065981524194,-2.44472931536157,1.4012062628653));
#85126=CARTESIAN_POINT('Ctrl Pts',(15.5256990507878,-2.46339973191149,1.39595676241995));
#85127=CARTESIAN_POINT('Ctrl Pts',(15.4439852976864,-2.47804021465317,1.39070726197459));
#85128=CARTESIAN_POINT('Ctrl Pts',(15.3619356422798,-2.4927408803104,1.38543618230623));
#85129=CARTESIAN_POINT('Ctrl Pts',(15.2790650606302,-2.50337823301684,1.38016510263786));
#85130=CARTESIAN_POINT('Ctrl Pts',(15.1958097448168,-2.5098734617177,1.3748940229695));
#85131=CARTESIAN_POINT('Ctrl Pts',(15.1130422387048,-2.51633063356245,1.36965382762095));
#85132=CARTESIAN_POINT('Ctrl Pts',(15.0298949590122,-2.51869405103694,1.3644136322724));
#85133=CARTESIAN_POINT('Ctrl Pts',(14.9468040613674,-2.51693790986448,1.35917343692384));
#85134=CARTESIAN_POINT('Ctrl Pts',(14.8637402302972,-2.51518234074898,1.35393494855093));
#85135=CARTESIAN_POINT('Ctrl Pts',(14.7807332054025,-2.50930988796735,1.34869646017802));
#85136=CARTESIAN_POINT('Ctrl Pts',(14.6982193938658,-2.49934685783331,1.3434579718051));
#85137=CARTESIAN_POINT('Ctrl Pts',(14.6157076180462,-2.48938407349948,1.33821961267214));
#85138=CARTESIAN_POINT('Ctrl Pts',(14.5336894890003,-2.47533096881395,1.33298125353917));
#85139=CARTESIAN_POINT('Ctrl Pts',(14.4525951610934,-2.45726559255235,1.3277428944062));
#85140=CARTESIAN_POINT('Ctrl Pts',(14.3706219911186,-2.43900443672095,1.32244776570018));
#85141=CARTESIAN_POINT('Ctrl Pts',(14.2895932397855,-2.41664360508234,1.31715263699415));
#85142=CARTESIAN_POINT('Ctrl Pts',(14.2099396769268,-2.39031607447748,1.31185750828812));
#85143=CARTESIAN_POINT('Ctrl Pts',(14.1310273731703,-2.3642335488793,1.30661165625234));
#85144=CARTESIAN_POINT('Ctrl Pts',(14.0534651817788,-2.33425807187132,1.30136580421656));
#85145=CARTESIAN_POINT('Ctrl Pts',(13.977652192976,-2.300567584635,1.29611995218078));
#85146=CARTESIAN_POINT('Ctrl Pts',(13.900770985429,-2.26640239233115,1.29080018513963));
#85147=CARTESIAN_POINT('Ctrl Pts',(13.8256890957265,-2.22841690655591,1.28548041809848));
#85148=CARTESIAN_POINT('Ctrl Pts',(13.7527955721518,-2.18684415657719,1.28016065105733));
#85149=CARTESIAN_POINT('Ctrl Pts',(13.6799020485771,-2.14527140659847,1.27484088401618));
#85150=CARTESIAN_POINT('Ctrl Pts',(13.6091972676224,-2.10011170871136,1.26952111697503));
#85151=CARTESIAN_POINT('Ctrl Pts',(13.5410369757164,-2.05164157292967,1.26420134993388));
#85152=CARTESIAN_POINT('Ctrl Pts',(13.4741232279713,-2.00405787943052,1.25897887303567));
#85153=CARTESIAN_POINT('Ctrl Pts',(13.4094090849756,-1.95310411137364,1.25375639613746));
#85154=CARTESIAN_POINT('Ctrl Pts',(13.347256781384,-1.89901187550754,1.24853391923926));
#85155=CARTESIAN_POINT('Ctrl Pts',(13.2851924765386,-1.84499622648807,1.24331883661919));
#85156=CARTESIAN_POINT('Ctrl Pts',(13.2256831586008,-1.78785123762157,1.23810375399912));
#85157=CARTESIAN_POINT('Ctrl Pts',(13.1690612555907,-1.72785114064289,1.23288867137906));
#85158=CARTESIAN_POINT('Ctrl Pts',(13.1125034378521,-1.66791895241148,1.22767949124491));
#85159=CARTESIAN_POINT('Ctrl Pts',(13.0588268608299,-1.60513841555441,1.22247031111076));
#85160=CARTESIAN_POINT('Ctrl Pts',(13.0083289359024,-1.53982226975597,1.21726113097661));
#85161=CARTESIAN_POINT('Ctrl Pts',(12.957861901448,-1.47454607899821,1.21205513739001));
#85162=CARTESIAN_POINT('Ctrl Pts',(12.9105699454521,-1.40673772684094,1.20684914380342));
#85163=CARTESIAN_POINT('Ctrl Pts',(12.8667110190326,-1.33674394469659,1.20164315021682));
#85164=CARTESIAN_POINT('Ctrl Pts',(12.8228652630735,-1.26677118108634,1.19643871994556));
#85165=CARTESIAN_POINT('Ctrl Pts',(12.7824507378214,-1.19461468686452,1.19123428967431));
#85166=CARTESIAN_POINT('Ctrl Pts',(12.7456819263984,-1.12064993331245,1.18602985940305));
#85167=CARTESIAN_POINT('Ctrl Pts',(12.7089127056805,-1.04668435641591,1.18082537119827));
#85168=CARTESIAN_POINT('Ctrl Pts',(12.675789485934,-0.970910900012858,1.17562088299349));
#85169=CARTESIAN_POINT('Ctrl Pts',(12.6464799915257,-0.893728045722679,
1.17041639478872));
#85170=CARTESIAN_POINT('Ctrl Pts',(12.6171422653402,-0.816470846610217,
1.16520689346601));
#85171=CARTESIAN_POINT('Ctrl Pts',(12.591625765819,-0.737801977180131,1.1599973921433));
#85172=CARTESIAN_POINT('Ctrl Pts',(12.570049153169,-0.658137623894178,1.15478789082059));
#85173=CARTESIAN_POINT('Ctrl Pts',(12.5484616479362,-0.578433053426348,
1.14957575957052));
#85174=CARTESIAN_POINT('Ctrl Pts',(12.5308180891762,-0.497732455885842,
1.14436362832046));
#85175=CARTESIAN_POINT('Ctrl Pts',(12.5171860071357,-0.416462395466049,
1.13915149707039));
#85176=CARTESIAN_POINT('Ctrl Pts',(12.5035311990925,-0.335056849974474,
1.13393067669209));
#85177=CARTESIAN_POINT('Ctrl Pts',(12.493901276518,-0.253080410737266,1.12870985631379));
#85178=CARTESIAN_POINT('Ctrl Pts',(12.4883118481157,-0.17096455095729,1.12348903593549));
#85179=CARTESIAN_POINT('Ctrl Pts',(12.4844199427861,-0.113787478575951,
1.11985379147163));
#85180=CARTESIAN_POINT('Ctrl Pts',(12.4824858930936,-0.0565428733787466,
1.11621854700778));
#85181=CARTESIAN_POINT('Ctrl Pts',(12.482500077493,0.000624641887355624,
1.11258330254392));
#85182=CARTESIAN_POINT('Ctrl Pts',(12.4825000774932,0.000624642704131756,
1.11258330249198));
#85183=CARTESIAN_POINT('Ctrl Pts',(12.4825084108427,0.0342105732934546,
1.11044759539204));
#85184=CARTESIAN_POINT('Ctrl Pts',(12.483188820319,0.0677874220149789,1.10831188829209));
#85185=CARTESIAN_POINT('Ctrl Pts',(12.4845403861397,0.101336967774151,1.10617618119214));
#85186=CARTESIAN_POINT('Ctrl Pts',(12.487867196913,0.183917474445178,1.10091924639843));
#85187=CARTESIAN_POINT('Ctrl Pts',(12.4952709795173,0.266485193006332,1.09566231160471));
#85188=CARTESIAN_POINT('Ctrl Pts',(12.5067530227982,0.348605451297277,1.090405376811));
#85189=CARTESIAN_POINT('Ctrl Pts',(12.5182208248965,0.430623855801245,1.08515496219548));
#85190=CARTESIAN_POINT('Ctrl Pts',(12.5337567860609,0.512195448942675,1.07990454757996));
#85191=CARTESIAN_POINT('Ctrl Pts',(12.5533102255289,0.592887339634366,1.07465413296444));
#85192=CARTESIAN_POINT('Ctrl Pts',(12.5728415567011,0.67348799521644,1.06940965478378));
#85193=CARTESIAN_POINT('Ctrl Pts',(12.5963812299632,0.753210479528745,1.06416517660313));
#85194=CARTESIAN_POINT('Ctrl Pts',(12.6238272147944,0.831630413614315,1.05892069842248));
#85195=CARTESIAN_POINT('Ctrl Pts',(12.6286229091916,0.845332892896281,1.05800431976885));
#85196=CARTESIAN_POINT('Ctrl Pts',(12.6335377426765,0.858995630875053,1.05708794111522));
#85197=CARTESIAN_POINT('Ctrl Pts',(12.6385710119932,0.872616401748845,1.05617156246159));
#85198=CARTESIAN_POINT('',(12.4825009284562,-0.00216212305302416,1.38677784361821));
#85199=CARTESIAN_POINT('Ctrl Pts',(12.6385710124998,0.872616403119952,1.33336808075876));
#85200=CARTESIAN_POINT('Ctrl Pts',(12.6355305680993,0.8643885110971,1.33393189393573));
#85201=CARTESIAN_POINT('Ctrl Pts',(12.6325330147833,0.856144426973078,1.33449432094504));
#85202=CARTESIAN_POINT('Ctrl Pts',(12.6173637559732,0.813735893510851,1.33737482604954));
#85203=CARTESIAN_POINT('Ctrl Pts',(12.6058878915727,0.779325997287395,1.33966980309984));
#85204=CARTESIAN_POINT('Ctrl Pts',(12.5835218975054,0.707097983881072,1.344404214739));
#85205=CARTESIAN_POINT('Ctrl Pts',(12.5727667838583,0.669248206453787,1.34683874017852));
#85206=CARTESIAN_POINT('Ctrl Pts',(12.5453463927905,0.563369916881544,1.35353261847241));
#85207=CARTESIAN_POINT('Ctrl Pts',(12.5306251909079,0.494873000545777,1.35773061810491));
#85208=CARTESIAN_POINT('Ctrl Pts',(12.4945139350419,0.28446855221848,1.37033632056842));
#85209=CARTESIAN_POINT('Ctrl Pts',(12.482377734934,0.141280026253996,1.3785060527829));
#85210=CARTESIAN_POINT('Ctrl Pts',(12.4825009284562,-0.00216212305302416,
1.38677784361821));
#85211=CARTESIAN_POINT('Ctrl Pts',(12.4825009299462,-0.00216385721130979,
1.38677794362086));
#85212=CARTESIAN_POINT('Ctrl Pts',(12.4825892483069,-0.104916196833896,
1.39270330065558));
#85213=CARTESIAN_POINT('Ctrl Pts',(12.4889682976042,-0.207560627536312,
1.3986735855389));
#85214=CARTESIAN_POINT('Ctrl Pts',(12.5048507408771,-0.335761172816142,
1.40649340025748));
#85215=CARTESIAN_POINT('Ctrl Pts',(12.5085147022134,-0.361947903654483,
1.40811012268778));
#85216=CARTESIAN_POINT('Ctrl Pts',(12.5162476916813,-0.411513873520081,
1.41121534118018));
#85217=CARTESIAN_POINT('Ctrl Pts',(12.520236180417,-0.434902856207706,1.41269981151196));
#85218=CARTESIAN_POINT('Ctrl Pts',(12.5283404218897,-0.478683422575586,
1.41552050337111));
#85219=CARTESIAN_POINT('Ctrl Pts',(12.5323793961633,-0.499086486809031,
1.41685272620698));
#85220=CARTESIAN_POINT('Ctrl Pts',(12.5435701409766,-0.552156532842023,
1.42036090508382));
#85221=CARTESIAN_POINT('Ctrl Pts',(12.5511207110053,-0.584734522784112,
1.42255687870184));
#85222=CARTESIAN_POINT('Ctrl Pts',(12.5898208418566,-0.737784271775964,
1.43304460782569));
#85223=CARTESIAN_POINT('Ctrl Pts',(12.6292237528481,-0.855981706468816,
1.44163978898629));
#85224=CARTESIAN_POINT('Ctrl Pts',(12.7213243261735,-1.07635404331246,1.45812984796642));
#85225=CARTESIAN_POINT('Ctrl Pts',(12.7726008054748,-1.17881185003668,1.46600707315879));
#85226=CARTESIAN_POINT('Ctrl Pts',(12.8696346885768,-1.34359419022276,1.47886567489774));
#85227=CARTESIAN_POINT('Ctrl Pts',(12.9116047242935,-1.40794490190253,1.48394247053915));
#85228=CARTESIAN_POINT('Ctrl Pts',(12.98004715759,-1.50307306120157,1.49152961640535));
#85229=CARTESIAN_POINT('Ctrl Pts',(13.0044264765366,-1.53529304490731,1.49411517126841));
#85230=CARTESIAN_POINT('Ctrl Pts',(13.0519589120643,-1.59506610975866,1.49894622858357));
#85231=CARTESIAN_POINT('Ctrl Pts',(13.0749475629069,-1.62273636235345,1.50119737576193));
#85232=CARTESIAN_POINT('Ctrl Pts',(13.13024775295,-1.6864685397244,1.50642393084478));
#85233=CARTESIAN_POINT('Ctrl Pts',(13.1630226564683,-1.72211042331781,1.50937939223633));
#85234=CARTESIAN_POINT('Ctrl Pts',(13.3242278965214,-1.88757397845849,1.52330546163752));
#85235=CARTESIAN_POINT('Ctrl Pts',(13.4654987813836,-2.00411064473487,1.5336958325686));
#85236=CARTESIAN_POINT('Ctrl Pts',(13.6850933788845,-2.14831148067518,1.54883717387851));
#85237=CARTESIAN_POINT('Ctrl Pts',(13.7541011920106,-2.18905376466235,1.55347870452628));
#85238=CARTESIAN_POINT('Ctrl Pts',(13.8702200028078,-2.25033909973641,1.56128444311747));
#85239=CARTESIAN_POINT('Ctrl Pts',(13.916226581866,-2.2728535651194,1.56437634709942));
#85240=CARTESIAN_POINT('Ctrl Pts',(13.9848749127448,-2.30389013378527,1.56903456425697));
#85241=CARTESIAN_POINT('Ctrl Pts',(14.0070064947898,-2.31351517900331,1.57054299525911));
#85242=CARTESIAN_POINT('Ctrl Pts',(14.0483277918833,-2.33078373093992,1.57337777282385));
#85243=CARTESIAN_POINT('Ctrl Pts',(14.0674791081453,-2.33851180385144,1.57469933416925));
#85244=CARTESIAN_POINT('Ctrl Pts',(14.1169631171702,-2.35777547884206,1.57813098772628));
#85245=CARTESIAN_POINT('Ctrl Pts',(14.1474270361532,-2.36896147095265,1.5802594486682));
#85246=CARTESIAN_POINT('Ctrl Pts',(14.3148833064831,-2.42680120916045,1.59201338086093));
#85247=CARTESIAN_POINT('Ctrl Pts',(14.4554793639651,-2.4621618230667,1.60206073063141));
#85248=CARTESIAN_POINT('Ctrl Pts',(14.7001148641056,-2.50170090304566,1.61915343978747));
#85249=CARTESIAN_POINT('Ctrl Pts',(14.8028283632692,-2.51188473217001,1.62622000138453));
#85250=CARTESIAN_POINT('Ctrl Pts',(14.9782121176192,-2.51844599464298,1.63798655529033));
#85251=CARTESIAN_POINT('Ctrl Pts',(15.0506284814945,-2.51803164444162,1.64276002376625));
#85252=CARTESIAN_POINT('Ctrl Pts',(15.1626026507913,-2.51255728619015,1.65000757925224));
#85253=CARTESIAN_POINT('Ctrl Pts',(15.2022231379348,-2.50967922932441,1.65254636893324));
#85254=CARTESIAN_POINT('Ctrl Pts',(15.2777386914124,-2.50239363856914,1.65734025358771));
#85255=CARTESIAN_POINT('Ctrl Pts',(15.3136389826725,-2.49814801535511,1.65959975926562));
#85256=CARTESIAN_POINT('Ctrl Pts',(15.3988644029457,-2.48620282888378,1.66492380853644));
#85257=CARTESIAN_POINT('Ctrl Pts',(15.4480772062119,-2.47780641812479,1.6679659463003));
#85258=CARTESIAN_POINT('Ctrl Pts',(15.6114402148443,-2.44490742603661,1.67799269507686));
#85259=CARTESIAN_POINT('Ctrl Pts',(15.7241337920546,-2.41393149915663,1.68478407736683));
#85260=CARTESIAN_POINT('Ctrl Pts',(15.9505326720198,-2.33441127903611,1.69861748860469));
#85261=CARTESIAN_POINT('Ctrl Pts',(16.0636257656841,-2.28510085937189,1.70563446276486));
#85262=CARTESIAN_POINT('Ctrl Pts',(16.2301373500441,-2.19745058220073,1.71670126144634));
#85263=CARTESIAN_POINT('Ctrl Pts',(16.2864285066132,-2.16497743004938,1.72058322386198));
#85264=CARTESIAN_POINT('Ctrl Pts',(16.363449672329,-2.1164806704514,1.7261840735252));
#85265=CARTESIAN_POINT('Ctrl Pts',(16.3852852783155,-2.10225355397403,1.72780599617266));
#85266=CARTESIAN_POINT('Ctrl Pts',(16.4238841942221,-2.07624173984677,1.73074196355354));
#85267=CARTESIAN_POINT('Ctrl Pts',(16.4407311235664,-2.06458705151344,1.73204799773991));
#85268=CARTESIAN_POINT('Ctrl Pts',(16.4812585302018,-2.03581265527393,1.73524924518821));
#85269=CARTESIAN_POINT('Ctrl Pts',(16.5047857137513,-2.01848452501289,1.73715721951164));
#85270=CARTESIAN_POINT('Ctrl Pts',(16.6069693764728,-1.94044530022182,1.74564598920864));
#85271=CARTESIAN_POINT('Ctrl Pts',(16.6822878264905,-1.87552198042389,1.75243769924464));
#85272=CARTESIAN_POINT('Ctrl Pts',(16.8518608558646,-1.71090184000058,1.76871839540953));
#85273=CARTESIAN_POINT('Ctrl Pts',(16.9422097971594,-1.60760679634545,1.77821819657449));
#85274=CARTESIAN_POINT('Ctrl Pts',(17.0738212460485,-1.42974460685774,1.79316314695867));
#85275=CARTESIAN_POINT('Ctrl Pts',(17.1205075522731,-1.35954200723028,1.79875588217141));
#85276=CARTESIAN_POINT('Ctrl Pts',(17.184790037352,-1.25148639879039,1.80691307446885));
#85277=CARTESIAN_POINT('Ctrl Pts',(17.2051078310174,-1.21532937950084,1.80957213251245));
#85278=CARTESIAN_POINT('Ctrl Pts',(17.2412782557656,-1.14706518937248,1.81446706412267));
#85279=CARTESIAN_POINT('Ctrl Pts',(17.25735692092,-1.11509044926652,1.81671043248044));
#85280=CARTESIAN_POINT('Ctrl Pts',(17.2924073181679,-1.04152002741431,1.82176677462674));
#85281=CARTESIAN_POINT('Ctrl Pts',(17.3109390574179,-0.999728140014245,
1.82456423269701));
#85282=CARTESIAN_POINT('Ctrl Pts',(17.4042153827483,-0.772899745720214,
1.83939365813419));
#85283=CARTESIAN_POINT('Ctrl Pts',(17.4578958067133,-0.579982247226776,
1.85069374923668));
#85284=CARTESIAN_POINT('Ctrl Pts',(17.4993450584043,-0.310516115700269,
1.86644054002961));
#85285=CARTESIAN_POINT('Ctrl Pts',(17.5073040946449,-0.237846517424953,
1.87069213030698));
#85286=CARTESIAN_POINT('Ctrl Pts',(17.5152606123427,-0.116664778559043,
1.87793122705907));
#85287=CARTESIAN_POINT('Ctrl Pts',(17.5170377935756,-0.0683133356656833,
1.88085910329622));
#85288=CARTESIAN_POINT('Ctrl Pts',(17.517608524097,0.0037259544731554,1.88531917079733));
#85289=CARTESIAN_POINT('Ctrl Pts',(17.5174621925834,0.0273965498554707,
1.88680038766788));
#85290=CARTESIAN_POINT('Ctrl Pts',(17.5165597759672,0.0718803955753969,
1.88961945263629));
#85291=CARTESIAN_POINT('Ctrl Pts',(17.5158791451036,0.0926925086391416,
1.89095341406106));
#85292=CARTESIAN_POINT('Ctrl Pts',(17.5134260278189,0.147052398414725,1.89447359008228));
#85293=CARTESIAN_POINT('Ctrl Pts',(17.5112400549014,0.180576670410615,1.89668007933511));
#85294=CARTESIAN_POINT('Ctrl Pts',(17.4988012058636,0.326346885681827,1.90640136823097));
#85295=CARTESIAN_POINT('Ctrl Pts',(17.4816880976136,0.43786993804315,1.91416191140293));
#85296=CARTESIAN_POINT('Ctrl Pts',(17.4306564751432,0.666747111005294,1.93034945422796));
#85297=CARTESIAN_POINT('Ctrl Pts',(17.3955541265528,0.783560543061855,1.93875597559673));
#85298=CARTESIAN_POINT('Ctrl Pts',(17.3238259030189,0.971568041452843,1.95230904323382));
#85299=CARTESIAN_POINT('Ctrl Pts',(17.2920255170955,1.0443813841952,1.95756681384005));
#85300=CARTESIAN_POINT('Ctrl Pts',(17.2387610699576,1.15213644022985,1.96535494368297));
#85301=CARTESIAN_POINT('Ctrl Pts',(17.219802414759,1.18825378687309,1.96796709407843));
#85302=CARTESIAN_POINT('Ctrl Pts',(17.1825262863821,1.25525823529334,1.97282047676086));
#85303=CARTESIAN_POINT('Ctrl Pts',(17.1644096465376,1.28624465844413,1.97506803624026));
#85304=CARTESIAN_POINT('Ctrl Pts',(17.1211458153943,1.35673827949321,1.98019454043744));
#85305=CARTESIAN_POINT('Ctrl Pts',(17.0955462649591,1.3959529392483,1.98305622246118));
#85306=CARTESIAN_POINT('Ctrl Pts',(16.9599922186528,1.59146103927357,1.99741846958626));
#85307=CARTESIAN_POINT('Ctrl Pts',(16.8335965174715,1.73558270055007,2.00826530212706));
#85308=CARTESIAN_POINT('Ctrl Pts',(16.6354761722271,1.91543031199457,2.02370243437099));
#85309=CARTESIAN_POINT('Ctrl Pts',(16.5765374994451,1.96422600629548,2.02814336314053));
#85310=CARTESIAN_POINT('Ctrl Pts',(16.475725445798,2.04022508747897,2.0356588733976));
#85311=CARTESIAN_POINT('Ctrl Pts',(16.4351005888672,2.0690020774596,2.03866779232439));
#85312=CARTESIAN_POINT('Ctrl Pts',(16.3737471440655,2.10978585218213,2.04322584831046));
#85313=CARTESIAN_POINT('Ctrl Pts',(16.353655179001,2.12273293430859,2.04472064667779));
#85314=CARTESIAN_POINT('Ctrl Pts',(16.315796830307,2.14637247547994,2.0475471671789));
#85315=CARTESIAN_POINT('Ctrl Pts',(16.2980773879768,2.15713492253999,2.04887454940363));
#85316=CARTESIAN_POINT('Ctrl Pts',(16.2518140099119,2.18445803425106,2.05234853733703));
#85317=CARTESIAN_POINT('Ctrl Pts',(16.2230743446823,2.20067810460126,2.05451442449593));
#85318=CARTESIAN_POINT('Ctrl Pts',(16.0765527714209,2.27961523632146,2.06556467230243));
#85319=CARTESIAN_POINT('Ctrl Pts',(15.9542423588839,2.33345838445376,2.07480287282561));
#85320=CARTESIAN_POINT('Ctrl Pts',(15.7250141946449,2.41331977972933,2.09155788131163));
#85321=CARTESIAN_POINT('Ctrl Pts',(15.6195359333951,2.44252667976103,2.09906899473149));
#85322=CARTESIAN_POINT('Ctrl Pts',(15.4599903239398,2.47569991955132,2.11001272623214));
#85323=CARTESIAN_POINT('Ctrl Pts',(15.4071565630592,2.48493568833214,2.11357175830024));
#85324=CARTESIAN_POINT('Ctrl Pts',(15.3074572408588,2.49909832027411,2.12016291192237));
#85325=CARTESIAN_POINT('Ctrl Pts',(15.260670592234,2.50441084814274,2.12320507377839));
#85326=CARTESIAN_POINT('Ctrl Pts',(15.1780557861838,2.51145105875922,2.12849144563821));
#85327=CARTESIAN_POINT('Ctrl Pts',(15.1422895026663,2.51373113006754,2.13075211386224));
#85328=CARTESIAN_POINT('Ctrl Pts',(15.0654104952545,2.51698587026842,2.13555631238731));
#85329=CARTESIAN_POINT('Ctrl Pts',(15.0242976787143,2.51771847698641,2.13809171566911));
#85330=CARTESIAN_POINT('Ctrl Pts',(14.9014902289023,2.51689812121091,2.14557988627));
#85331=CARTESIAN_POINT('Ctrl Pts',(14.8198674198282,2.51237624622363,2.150442400473));
#85332=CARTESIAN_POINT('Ctrl Pts',(14.6935232123984,2.49918637817835,2.15788702321381));
#85333=CARTESIAN_POINT('Ctrl Pts',(14.6485778876443,2.49326357614882,2.16051953685836));
#85334=CARTESIAN_POINT('Ctrl Pts',(14.471537435022,2.46505081649111,2.17088193332234));
#85335=CARTESIAN_POINT('Ctrl Pts',(14.3411584247098,2.43344881236856,2.17848704099896));
#85336=CARTESIAN_POINT('Ctrl Pts',(14.1496998141575,2.37052006330617,2.19031949517956));
#85337=CARTESIAN_POINT('Ctrl Pts',(14.086362808083,2.34683645070651,2.19435154665354));
#85338=CARTESIAN_POINT('Ctrl Pts',(13.9997490364697,2.31041119111617,2.2001294707858));
#85339=CARTESIAN_POINT('Ctrl Pts',(13.9756003579974,2.29980588345927,2.20176985699335));
#85340=CARTESIAN_POINT('Ctrl Pts',(13.9330227528557,2.28030357624855,2.20472239058758));
#85341=CARTESIAN_POINT('Ctrl Pts',(13.9145281735862,2.27155798263263,2.20602597528365));
#85342=CARTESIAN_POINT('Ctrl Pts',(13.8702549237056,2.24995821636688,2.20919716297465));
#85343=CARTESIAN_POINT('Ctrl Pts',(13.8445875979461,2.23688576417375,2.21107683855228));
#85344=CARTESIAN_POINT('Ctrl Pts',(13.7395842249338,2.1811178516321,2.21892096953529));
#85345=CARTESIAN_POINT('Ctrl Pts',(13.6623493878982,2.13462197723981,2.22505812695252));
#85346=CARTESIAN_POINT('Ctrl Pts',(13.4856177280682,2.01486526181441,2.23973865984903));
#85347=CARTESIAN_POINT('Ctrl Pts',(13.3886793635801,1.9382166314849,2.24830699285757));
#85348=CARTESIAN_POINT('Ctrl Pts',(13.2230053353671,1.78616609995838,2.26362234613225));
#85349=CARTESIAN_POINT('Ctrl Pts',(13.1524667552495,1.71310377161154,2.270410727781));
#85350=CARTESIAN_POINT('Ctrl Pts',(13.0582340114413,1.60288683694009,2.2798525055689));
#85351=CARTESIAN_POINT('Ctrl Pts',(13.0308061955652,1.56906899529796,2.28265296446426));
#85352=CARTESIAN_POINT('Ctrl Pts',(12.9825291142042,1.5062832854388,2.28768436759806));
#85353=CARTESIAN_POINT('Ctrl Pts',(12.9613928204058,1.4775517207062,2.28992617231733));
#85354=CARTESIAN_POINT('Ctrl Pts',(12.9156291945434,1.4124906611709,2.29487491189316));
#85355=CARTESIAN_POINT('Ctrl Pts',(12.8913266425681,1.37594642151091,2.29756915648175));
#85356=CARTESIAN_POINT('Ctrl Pts',(12.8175004395359,1.25837840057791,2.3059926533752));
#85357=CARTESIAN_POINT('Ctrl Pts',(12.7715964034195,1.17517678895927,2.31159524001484));
#85358=CARTESIAN_POINT('Ctrl Pts',(12.6964686834177,1.01869138548658,2.32169059877296));
#85359=CARTESIAN_POINT('Ctrl Pts',(12.6657962272505,0.946291839447466,2.32620136657629));
#85360=CARTESIAN_POINT('Ctrl Pts',(12.6385710877721,0.872616606817863,2.33071866803842));
#85361=CARTESIAN_POINT('Origin',(15.,0.,3.));
#85362=CARTESIAN_POINT('',(12.6385710144774,0.87261640847139,3.32953357812844));
#85363=CARTESIAN_POINT('',(12.6408521577454,0.871797393741481,3.05636274128509));
#85364=CARTESIAN_POINT('',(12.6385710119932,0.872616401748847,3.));
#85365=CARTESIAN_POINT('',(12.4849790795627,0.00159552663997447,2.11258330249198));
#85366=CARTESIAN_POINT('Ctrl Pts',(12.6408521577454,0.87179739374149,3.05636274128509));
#85367=CARTESIAN_POINT('Ctrl Pts',(12.7375264301118,1.13962417266692,3.03840122955439));
#85368=CARTESIAN_POINT('Ctrl Pts',(13.2888950829206,2.12729580985852,2.96776466157644));
#85369=CARTESIAN_POINT('Ctrl Pts',(15.3377008476539,2.95164299596017,2.84445303735124));
#85370=CARTESIAN_POINT('Ctrl Pts',(17.6568119242111,1.32950708964651,2.6864278686095));
#85371=CARTESIAN_POINT('Ctrl Pts',(17.5649293736244,-1.49912516962393,2.52840269986778));
#85372=CARTESIAN_POINT('Ctrl Pts',(15.1454344282297,-2.96733641764902,2.37037753112603));
#85373=CARTESIAN_POINT('Ctrl Pts',(12.9074954366079,-1.89324175649192,2.23177106533412));
#85374=CARTESIAN_POINT('Ctrl Pts',(12.4885048299379,-0.525856856019931,
2.14583965578942));
#85375=CARTESIAN_POINT('Ctrl Pts',(12.4854125712649,0.00159525163329232,
2.11258330249198));
#85376=CARTESIAN_POINT('Ctrl Pts',(12.4825005065989,0.00159709904406843,
2.11258330249198));
#85377=CARTESIAN_POINT('Ctrl Pts',(12.4825600916737,0.0955207640184819,
2.10666815249281));
#85378=CARTESIAN_POINT('Ctrl Pts',(12.4878799426804,0.189246299602191,2.10075300249363));
#85379=CARTESIAN_POINT('Ctrl Pts',(12.498369487036,0.282225134612964,2.09483785249446));
#85380=CARTESIAN_POINT('Ctrl Pts',(12.5089078977187,0.375637118482618,2.08889514632649));
#85381=CARTESIAN_POINT('Ctrl Pts',(12.5246641526241,0.468295217851566,2.08295244015852));
#85382=CARTESIAN_POINT('Ctrl Pts',(12.5454968432786,0.559661061397646,2.07700973399055));
#85383=CARTESIAN_POINT('Ctrl Pts',(12.5664420987786,0.651520580111855,2.07103491772155));
#85384=CARTESIAN_POINT('Ctrl Pts',(12.592518678278,0.742073636519814,2.06506010145255));
#85385=CARTESIAN_POINT('Ctrl Pts',(12.6235347394388,0.83079426776169,2.05908528518355));
#85386=CARTESIAN_POINT('Ctrl Pts',(12.6284244458395,0.844781144954579,2.05814335070637));
#85387=CARTESIAN_POINT('Ctrl Pts',(12.6334368223796,0.858722525631891,2.05720141622918));
#85388=CARTESIAN_POINT('Ctrl Pts',(12.6385710119932,0.872616401748851,2.05625948175199));
#85389=CARTESIAN_POINT('Ctrl Pts',(12.6385710877721,0.872616606817863,2.33071866803842));
#85390=CARTESIAN_POINT('Ctrl Pts',(12.6130828119274,0.803641582697994,2.33494778230365));
#85391=CARTESIAN_POINT('Ctrl Pts',(12.5906160635846,0.733548458146182,2.33918298169588));
#85392=CARTESIAN_POINT('Ctrl Pts',(12.5524234413054,0.593540129543784,2.34768324219969));
#85393=CARTESIAN_POINT('Ctrl Pts',(12.5365523828507,0.523779504389352,2.35193820193661));
#85394=CARTESIAN_POINT('Ctrl Pts',(12.5188442919751,0.427073034483106,2.35797802765619));
#85395=CARTESIAN_POINT('Ctrl Pts',(12.5144371661924,0.400627362594168,2.35964408622218));
#85396=CARTESIAN_POINT('Ctrl Pts',(12.507416771345,0.353910509147975,2.36262047332756));
#85397=CARTESIAN_POINT('Ctrl Pts',(12.5046265882995,0.333669376866167,2.36392147830763));
#85398=CARTESIAN_POINT('Ctrl Pts',(12.4985634376397,0.285343195659269,2.36705479121824));
#85399=CARTESIAN_POINT('Ctrl Pts',(12.4955168157114,0.257234194162914,2.36889828846849));
#85400=CARTESIAN_POINT('Ctrl Pts',(12.4860363282071,0.153480172861711,2.37576578528259));
#85401=CARTESIAN_POINT('Ctrl Pts',(12.4825520719847,0.0776112608302906,
2.38090946543098));
#85402=CARTESIAN_POINT('Ctrl Pts',(12.4823712472628,-0.188935106255942,
2.39917119488424));
#85403=CARTESIAN_POINT('Ctrl Pts',(12.5038986407159,-0.379004630001638,
2.41247744373233));
#85404=CARTESIAN_POINT('Ctrl Pts',(12.561621777294,-0.62972438427405,2.4296525467515));
#85405=CARTESIAN_POINT('Ctrl Pts',(12.5791332370533,-0.69400762931579,2.43402857148568));
#85406=CARTESIAN_POINT('Ctrl Pts',(12.6108458804789,-0.794514453660138,
2.44082697973957));
#85407=CARTESIAN_POINT('Ctrl Pts',(12.6233705584292,-0.831230048995139,
2.44330128017505));
#85408=CARTESIAN_POINT('Ctrl Pts',(12.6493220850701,-0.901916037334384,
2.44805104517824));
#85409=CARTESIAN_POINT('Ctrl Pts',(12.6626494599651,-0.935912320495879,
2.45032908331539));
#85410=CARTESIAN_POINT('Ctrl Pts',(12.6969570928146,-1.01811718436349,2.45582918360601));
#85411=CARTESIAN_POINT('Ctrl Pts',(12.7187172560145,-1.06598258021218,2.45902438756089));
#85412=CARTESIAN_POINT('Ctrl Pts',(12.7697381517989,-1.1694805662318,2.46594578407214));
#85413=CARTESIAN_POINT('Ctrl Pts',(12.7996153607669,-1.22476972659078,2.46965127771572));
#85414=CARTESIAN_POINT('Ctrl Pts',(12.9115164949221,-1.41450838567484,2.48250609407803));
#85415=CARTESIAN_POINT('Ctrl Pts',(13.0040449393849,-1.54232234967238,2.49139891274401));
#85416=CARTESIAN_POINT('Ctrl Pts',(13.1569229405479,-1.71650687108799,2.50494199649724));
#85417=CARTESIAN_POINT('Ctrl Pts',(13.208388994884,-1.77015733273108,2.50935071471145));
#85418=CARTESIAN_POINT('Ctrl Pts',(13.2803226749894,-1.83878960470903,2.51544573372024));
#85419=CARTESIAN_POINT('Ctrl Pts',(13.2987557962732,-1.85585704180918,2.51700216684152));
#85420=CARTESIAN_POINT('Ctrl Pts',(13.3327264208623,-1.88637943135215,2.5198675830547));
#85421=CARTESIAN_POINT('Ctrl Pts',(13.3481784054611,-1.89992471664867,2.52117017057166));
#85422=CARTESIAN_POINT('Ctrl Pts',(13.3832170828368,-1.92988919622541,2.52412446271687));
#85423=CARTESIAN_POINT('Ctrl Pts',(13.4028895777065,-1.9462007821441,2.52578271121433));
#85424=CARTESIAN_POINT('Ctrl Pts',(13.4703418359251,-2.0004178826431,2.53145717917954));
#85425=CARTESIAN_POINT('Ctrl Pts',(13.5192468228761,-2.03688356324417,2.53555225558514));
#85426=CARTESIAN_POINT('Ctrl Pts',(13.6589586137463,-2.13336683449742,2.54709888821033));
#85427=CARTESIAN_POINT('Ctrl Pts',(13.7524063522685,-2.18932756366017,2.55464758714719));
#85428=CARTESIAN_POINT('Ctrl Pts',(13.968793545032,-2.30054489448085,2.57141144763015));
#85429=CARTESIAN_POINT('Ctrl Pts',(14.0931555196742,-2.35234673683755,2.58056594074289));
#85430=CARTESIAN_POINT('Ctrl Pts',(14.2693340079656,-2.40966987317855,2.59274870356547));
#85431=CARTESIAN_POINT('Ctrl Pts',(14.3180589205194,-2.42390978730885,2.59604124906964));
#85432=CARTESIAN_POINT('Ctrl Pts',(14.4022742725217,-2.44578097548938,2.60160536773693));
#85433=CARTESIAN_POINT('Ctrl Pts',(14.4375586730536,-2.45413540800816,2.60389931376189));
#85434=CARTESIAN_POINT('Ctrl Pts',(14.5115320331716,-2.46997105733845,2.60863569393038));
#85435=CARTESIAN_POINT('Ctrl Pts',(14.5502410776344,-2.47731208371283,2.61107312739481));
#85436=CARTESIAN_POINT('Ctrl Pts',(14.6584923043308,-2.49522036063281,2.61778778958015));
#85437=CARTESIAN_POINT('Ctrl Pts',(14.728330640856,-2.50378696515588,2.62200299266667));
#85438=CARTESIAN_POINT('Ctrl Pts',(14.896343800069,-2.51728195899517,2.63195379493515));
#85439=CARTESIAN_POINT('Ctrl Pts',(14.9946267218981,-2.51940978863386,2.63761894385376));
#85440=CARTESIAN_POINT('Ctrl Pts',(15.2478670917557,-2.51006993620561,2.65219537605792));
#85441=CARTESIAN_POINT('Ctrl Pts',(15.4020694883506,-2.49002372021481,2.66104420567355));
#85442=CARTESIAN_POINT('Ctrl Pts',(15.5840392331565,-2.44901801812302,2.67240481473275));
#85443=CARTESIAN_POINT('Ctrl Pts',(15.6145202497099,-2.4415478145329,2.6743402209903));
#85444=CARTESIAN_POINT('Ctrl Pts',(15.6648707888756,-2.42820550531402,2.67760334491258));
#85445=CARTESIAN_POINT('Ctrl Pts',(15.6848213586035,-2.42265449900531,2.67891393963998));
#85446=CARTESIAN_POINT('Ctrl Pts',(15.7284563377012,-2.40993149874373,2.68182229987095));
#85447=CARTESIAN_POINT('Ctrl Pts',(15.7521056541362,-2.40265591258142,2.6834251502501));
#85448=CARTESIAN_POINT('Ctrl Pts',(15.8281476360055,-2.37802936055742,2.68865666441717));
#85449=CARTESIAN_POINT('Ctrl Pts',(15.8800753365586,-2.35930469086154,2.69234920354004));
#85450=CARTESIAN_POINT('Ctrl Pts',(16.015735118432,-2.30528523044506,2.70224519428313));
#85451=CARTESIAN_POINT('Ctrl Pts',(16.0982447167614,-2.2671380950189,2.70852057197804));
#85452=CARTESIAN_POINT('Ctrl Pts',(16.320671280704,-2.149305839092,2.72589844658641));
#85453=CARTESIAN_POINT('Ctrl Pts',(16.4553064853032,-2.06053028658965,2.73692750398818));
#85454=CARTESIAN_POINT('Ctrl Pts',(16.619939130365,-1.92773522883161,2.75083350506466));
#85455=CARTESIAN_POINT('Ctrl Pts',(16.658353873918,-1.89478994227332,2.7541154273558));
#85456=CARTESIAN_POINT('Ctrl Pts',(16.7225325009139,-1.83630087459142,2.75966760613806));
#85457=CARTESIAN_POINT('Ctrl Pts',(16.7487840597598,-1.81131820848578,2.76195997955683));
#85458=CARTESIAN_POINT('Ctrl Pts',(16.802472068631,-1.75796956885561,2.76669819636012));
#85459=CARTESIAN_POINT('Ctrl Pts',(16.8297994785494,-1.72950764734889,2.76913892611866));
#85460=CARTESIAN_POINT('Ctrl Pts',(16.9041951128387,-1.64828529421477,2.77587849233801));
#85461=CARTESIAN_POINT('Ctrl Pts',(16.9497281181776,-1.59416591792567,2.78011447275607));
#85462=CARTESIAN_POINT('Ctrl Pts',(17.0534578394276,-1.45977122291452,2.79013440968192));
#85463=CARTESIAN_POINT('Ctrl Pts',(17.1093099128012,-1.37783682148057,2.79584638422875));
#85464=CARTESIAN_POINT('Ctrl Pts',(17.2389235182868,-1.16126401172449,2.81036317370143));
#85465=CARTESIAN_POINT('Ctrl Pts',(17.3054659665301,-1.02280423164037,2.81911118867626));
#85466=CARTESIAN_POINT('Ctrl Pts',(17.3700250243665,-0.849579321335824,
2.83036641633348));
#85467=CARTESIAN_POINT('Ctrl Pts',(17.3804956210495,-0.819782912112732,
2.83231355926413));
#85468=CARTESIAN_POINT('Ctrl Pts',(17.3969076442725,-0.770110354874441,
2.83559011838298));
#85469=CARTESIAN_POINT('Ctrl Pts',(17.4031687656677,-0.750343968663925,
2.83690207018901));
#85470=CARTESIAN_POINT('Ctrl Pts',(17.4163358327527,-0.706919114294123,
2.83980509790709));
#85471=CARTESIAN_POINT('Ctrl Pts',(17.4231392968821,-0.683234458002295,
2.84140107421867));
#85472=CARTESIAN_POINT('Ctrl Pts',(17.4438732357607,-0.606845538499601,
2.84658048117067));
#85473=CARTESIAN_POINT('Ctrl Pts',(17.4564392045818,-0.553790066614681,
2.85022612797859));
#85474=CARTESIAN_POINT('Ctrl Pts',(17.4849478752528,-0.413217588018961,
2.85994264232883));
#85475=CARTESIAN_POINT('Ctrl Pts',(17.4979921456865,-0.325190309535636,
2.86608279581412));
#85476=CARTESIAN_POINT('Ctrl Pts',(17.5218021037186,-0.0730320571787507,
2.88356974141117));
#85477=CARTESIAN_POINT('Ctrl Pts',(17.5211937633259,0.0917399181762342,
2.89484575169084));
#85478=CARTESIAN_POINT('Ctrl Pts',(17.4994180485582,0.3053669965451,2.90895903658735));
#85479=CARTESIAN_POINT('Ctrl Pts',(17.4928131991141,0.35527809862235,2.91222318375574));
#85480=CARTESIAN_POINT('Ctrl Pts',(17.4788929623976,0.440688453307653,2.91775540713375));
#85481=CARTESIAN_POINT('Ctrl Pts',(17.472299877668,0.476287903941779,2.92004517318884));
#85482=CARTESIAN_POINT('Ctrl Pts',(17.4569016892818,0.550458471127815,2.92478662970764));
#85483=CARTESIAN_POINT('Ctrl Pts',(17.4479506260041,0.588989341534187,2.92723301440188));
#85484=CARTESIAN_POINT('Ctrl Pts',(17.4203246556744,0.696362639868777,2.93401544195895));
#85485=CARTESIAN_POINT('Ctrl Pts',(17.3996265525521,0.76464767828463,2.93828718784357));
#85486=CARTESIAN_POINT('Ctrl Pts',(17.342825289282,0.926869305729871,2.94842705298447));
#85487=CARTESIAN_POINT('Ctrl Pts',(17.3039381821449,1.01969966267607,2.95422048736621));
#85488=CARTESIAN_POINT('Ctrl Pts',(17.1934216397223,1.24468417293609,2.96863602741457));
#85489=CARTESIAN_POINT('Ctrl Pts',(17.1153323408748,1.37320649594988,2.97721026736162));
#85490=CARTESIAN_POINT('Ctrl Pts',(17.0073312115788,1.51968636251021,2.98828432077836));
#85491=CARTESIAN_POINT('Ctrl Pts',(16.9879016592406,1.54501521219778,2.99025146605093));
#85492=CARTESIAN_POINT('Ctrl Pts',(16.9550372473264,1.58621167316143,2.99355103380811));
#85493=CARTESIAN_POINT('Ctrl Pts',(16.9418782426142,1.60229428519577,2.9948654084667));
#85494=CARTESIAN_POINT('Ctrl Pts',(16.9127871596869,1.63696385526219,2.99775989330806));
#85495=CARTESIAN_POINT('Ctrl Pts',(16.8967816829363,1.65548316719344,2.99934459960838));
#85496=CARTESIAN_POINT('Ctrl Pts',(16.844992187807,1.71366972343203,3.0044397920781));
#85497=CARTESIAN_POINT('Ctrl Pts',(16.8082162523907,1.75243066238104,3.00800985827858));
#85498=CARTESIAN_POINT('Ctrl Pts',(16.7091447474894,1.8504089865478,3.01744199859366));
#85499=CARTESIAN_POINT('Ctrl Pts',(16.6450004613352,1.90765863392137,3.02336923184861));
#85500=CARTESIAN_POINT('Ctrl Pts',(16.4454745230108,2.06817925568255,3.04104935564278));
#85501=CARTESIAN_POINT('Ctrl Pts',(16.3023985038526,2.16114238104892,3.05273767550511));
#85502=CARTESIAN_POINT('Ctrl Pts',(16.1067230811676,2.26173627178208,3.06718909568718));
#85503=CARTESIAN_POINT('Ctrl Pts',(16.061758768532,2.28318983665751,3.07041740641836));
#85504=CARTESIAN_POINT('Ctrl Pts',(15.9831272891693,2.31788103496291,3.07590949396312));
#85505=CARTESIAN_POINT('Ctrl Pts',(15.9497583212086,2.33175279769755,3.07819410377899));
#85506=CARTESIAN_POINT('Ctrl Pts',(15.8790662600272,2.35937060683458,3.08294276886838));
#85507=CARTESIAN_POINT('Ctrl Pts',(15.8416926153348,2.37296038055608,3.08540111823881));
#85508=CARTESIAN_POINT('Ctrl Pts',(15.7351636844384,2.4088625810652,3.09227483770303));
#85509=CARTESIAN_POINT('Ctrl Pts',(15.6653404518237,2.42907554873721,3.09662279191374));
#85510=CARTESIAN_POINT('Ctrl Pts',(15.493891193051,2.47075868189329,3.10702225593738));
#85511=CARTESIAN_POINT('Ctrl Pts',(15.391623489351,2.48901778442396,3.11299302852617));
#85512=CARTESIAN_POINT('Ctrl Pts',(15.146065686656,2.51734657695677,3.12720674622698));
#85513=CARTESIAN_POINT('Ctrl Pts',(15.0024850399308,2.52157764254631,3.13541741038279));
#85514=CARTESIAN_POINT('Ctrl Pts',(14.8268331670838,2.51174833795092,3.14611140176326));
#85515=CARTESIAN_POINT('Ctrl Pts',(14.7943632052678,2.50929865528764,3.14811614536501));
#85516=CARTESIAN_POINT('Ctrl Pts',(14.7413773863779,2.50426590346203,3.15144647134996));
#85517=CARTESIAN_POINT('Ctrl Pts',(14.7208286087857,2.50205848914436,3.15275271131997));
#85518=CARTESIAN_POINT('Ctrl Pts',(14.6763964592994,2.49673127055157,3.15561252389852));
#85519=CARTESIAN_POINT('Ctrl Pts',(14.6525271857858,2.49352137043495,3.15717037702822));
#85520=CARTESIAN_POINT('Ctrl Pts',(14.5783602095451,2.48246197961092,3.16207056797737));
#85521=CARTESIAN_POINT('Ctrl Pts',(14.5282544826983,2.47342940167856,3.16546659467556));
#85522=CARTESIAN_POINT('Ctrl Pts',(14.4008692382386,2.44645437464517,3.17426536022568));
#85523=CARTESIAN_POINT('Ctrl Pts',(14.3241008378071,2.42636680393794,3.17972434738033));
#85524=CARTESIAN_POINT('Ctrl Pts',(14.0724453984637,2.34764626657905,3.19792228713017));
#85525=CARTESIAN_POINT('Ctrl Pts',(13.9030286189375,2.27342801338589,3.21062075383624));
#85526=CARTESIAN_POINT('Ctrl Pts',(13.7014713474306,2.15730188918366,3.22586865793446));
#85527=CARTESIAN_POINT('Ctrl Pts',(13.660416700625,2.13205187680984,3.22898647946852));
#85528=CARTESIAN_POINT('Ctrl Pts',(13.5900472659546,2.08593657995908,3.2343558114026));
#85529=CARTESIAN_POINT('Ctrl Pts',(13.5604089664217,2.06559337708123,3.23662554462106));
#85530=CARTESIAN_POINT('Ctrl Pts',(13.4983193755591,2.02099038091255,3.24140302932744));
#85531=CARTESIAN_POINT('Ctrl Pts',(13.4659973156161,1.99656777307702,3.24390371683415));
#85532=CARTESIAN_POINT('Ctrl Pts',(13.3735808157404,1.92316791501497,3.25110849738315));
#85533=CARTESIAN_POINT('Ctrl Pts',(13.3151397883925,1.87218104358476,3.25573327928046));
#85534=CARTESIAN_POINT('Ctrl Pts',(13.1750323971919,1.73806103147935,3.26712843159783));
#85535=CARTESIAN_POINT('Ctrl Pts',(13.09660867849,1.6518068151793,3.27379219278394));
#85536=CARTESIAN_POINT('Ctrl Pts',(12.9494462482203,1.46549394149441,3.28745594219608));
#85537=CARTESIAN_POINT('Ctrl Pts',(12.8814051859582,1.36528142804665,3.29444293075157));
#85538=CARTESIAN_POINT('Ctrl Pts',(12.8040119871058,1.23149179491109,3.30382294321753));
#85539=CARTESIAN_POINT('Ctrl Pts',(12.7877711928948,1.20207272920697,3.30588890254683));
#85540=CARTESIAN_POINT('Ctrl Pts',(12.7624275389304,1.15391047610687,3.30929091677925));
#85541=CARTESIAN_POINT('Ctrl Pts',(12.7529594182019,1.13536271968924,3.31060581369784));
#85542=CARTESIAN_POINT('Ctrl Pts',(12.7332240052087,1.09548756703211,3.31344662332477));
#85543=CARTESIAN_POINT('Ctrl Pts',(12.7230256448046,1.07412946294541,3.3149760349355));
#85544=CARTESIAN_POINT('Ctrl Pts',(12.6929105177186,1.00870357358768,3.31967760203572));
#85545=CARTESIAN_POINT('Ctrl Pts',(12.6739619501597,0.964204908918892,3.32289774862161));
#85546=CARTESIAN_POINT('Ctrl Pts',(12.6502414493595,0.903723990875261,3.32727933563373));
#85547=CARTESIAN_POINT('Ctrl Pts',(12.6443289208352,0.888198154170151,3.32840455789558));
#85548=CARTESIAN_POINT('Ctrl Pts',(12.6385710144774,0.872616408471391,3.32953357812844));
#85549=CARTESIAN_POINT('Origin',(15.,0.,3.));
#85550=CARTESIAN_POINT('',(12.6421214752944,0.871321765791503,4.3311309048973));
#85551=CARTESIAN_POINT('',(12.6385710119932,0.872616401748849,4.05617650648277));
#85552=CARTESIAN_POINT('',(12.6385710119932,0.872616401748847,3.));
#85553=CARTESIAN_POINT('',(12.4825008631916,-0.00208474671008541,3.11258330249198));
#85554=CARTESIAN_POINT('Ctrl Pts',(12.6385710119932,0.872616401748848,4.05617650648277));
#85555=CARTESIAN_POINT('Ctrl Pts',(12.6673543993352,0.950508503142112,4.05093727502692));
#85556=CARTESIAN_POINT('Ctrl Pts',(12.7000132622957,1.02702225238975,4.04569804357108));
#85557=CARTESIAN_POINT('Ctrl Pts',(12.7363857616833,1.10175170981944,4.04045881211524));
#85558=CARTESIAN_POINT('Ctrl Pts',(12.7727499931487,1.1764641803124,4.03522077160199));
#85559=CARTESIAN_POINT('Ctrl Pts',(12.8128259822694,1.24939275031694,4.02998273108873));
#85560=CARTESIAN_POINT('Ctrl Pts',(12.8564046387866,1.32015346736063,4.02474469057549));
#85561=CARTESIAN_POINT('Ctrl Pts',(12.8999865129388,1.3909194090299,4.01950626331092));
#85562=CARTESIAN_POINT('Ctrl Pts',(12.9470713250003,1.45951678803023,4.01426783604636));
#85563=CARTESIAN_POINT('Ctrl Pts',(12.99740584606,1.52558936303496,4.00902940878179));
#85564=CARTESIAN_POINT('Ctrl Pts',(13.0477923412206,1.59173016284064,4.00378557245519));
#85565=CARTESIAN_POINT('Ctrl Pts',(13.1014349655593,1.65534058553694,3.99854173612859));
#85566=CARTESIAN_POINT('Ctrl Pts',(13.1580395801034,1.71609675179873,3.99329789980198));
#85567=CARTESIAN_POINT('Ctrl Pts',(13.2146748413793,1.77688581251547,3.98805122437034));
#85568=CARTESIAN_POINT('Ctrl Pts',(13.2742749555559,1.83481721791559,3.9828045489387));
#85569=CARTESIAN_POINT('Ctrl Pts',(13.3365099735538,1.88960503331095,3.97755787350706));
#85570=CARTESIAN_POINT('Ctrl Pts',(13.3988511407322,1.94448629580235,3.97230224925022));
#85571=CARTESIAN_POINT('Ctrl Pts',(13.4638358265541,1.99621297218007,3.96704662499338));
#85572=CARTESIAN_POINT('Ctrl Pts',(13.5311024033621,2.04454055978144,3.96179100073653));
#85573=CARTESIAN_POINT('Ctrl Pts',(13.5787221749002,2.07875292481873,3.95807040667218));
#85574=CARTESIAN_POINT('Ctrl Pts',(13.6274848972943,2.11126270130169,3.95434981260783));
#85575=CARTESIAN_POINT('Ctrl Pts',(13.6772548532223,2.14199708839114,3.95062921854348));
#85576=CARTESIAN_POINT('Ctrl Pts',(13.7475729445644,2.18542054333301,3.94537253168521));
#85577=CARTESIAN_POINT('Ctrl Pts',(13.8201605534495,2.22545734514497,3.94011584482692));
#85578=CARTESIAN_POINT('Ctrl Pts',(13.8946580326627,2.26186325520417,3.93485915796864));
#85579=CARTESIAN_POINT('Ctrl Pts',(13.9690503549056,2.29821777647488,3.92960989119047));
#85580=CARTESIAN_POINT('Ctrl Pts',(14.0453467816793,2.33095138554809,3.9243606244123));
#85581=CARTESIAN_POINT('Ctrl Pts',(14.1231602579543,2.35986404624701,3.91911135763412));
#85582=CARTESIAN_POINT('Ctrl Pts',(14.2012979437543,2.38889717142634,3.91384021980777));
#85583=CARTESIAN_POINT('Ctrl Pts',(14.2809649492097,2.41407718758061,3.90856908198142));
#85584=CARTESIAN_POINT('Ctrl Pts',(14.3617459691189,2.43524907187419,3.90329794415507));
#85585=CARTESIAN_POINT('Ctrl Pts',(14.4420491594968,2.45629572190405,3.89805798574834));
#85586=CARTESIAN_POINT('Ctrl Pts',(14.5234527709189,2.47338140800351,3.89281802734161));
#85587=CARTESIAN_POINT('Ctrl Pts',(14.6055321909212,2.48640330549984,3.88757806893488));
#85588=CARTESIAN_POINT('Ctrl Pts',(14.687584861771,2.49942095924395,3.88233981819673));
#85589=CARTESIAN_POINT('Ctrl Pts',(14.7703124487109,2.50837738253097,3.87710156745857));
#85590=CARTESIAN_POINT('Ctrl Pts',(14.8532808396168,2.51322098868692,3.87186331672041));
#85591=CARTESIAN_POINT('Ctrl Pts',(14.9362471777384,2.5180644750035,3.86662519558582));
#85592=CARTESIAN_POINT('Ctrl Pts',(15.0194538475891,2.51879532071958,3.86138707445122));
#85593=CARTESIAN_POINT('Ctrl Pts',(15.102463704417,2.51541396976266,3.85614895331663));
#85594=CARTESIAN_POINT('Ctrl Pts',(15.1863814109029,2.51199563815757,3.85085354469038));
#85595=CARTESIAN_POINT('Ctrl Pts',(15.2700974917501,2.5043746142835,3.84555813606413));
#85596=CARTESIAN_POINT('Ctrl Pts',(15.3531643149952,2.49260530702595,3.84026272743787));
#85597=CARTESIAN_POINT('Ctrl Pts',(15.435450056159,2.48094666723647,3.83501711184125));
#85598=CARTESIAN_POINT('Ctrl Pts',(15.517098252225,2.46521757867526,3.82977149624463));
#85599=CARTESIAN_POINT('Ctrl Pts',(15.5976845977134,2.44552231060283,3.82452588064801));
#85600=CARTESIAN_POINT('Ctrl Pts',(15.6794183695281,2.42554661203124,3.81920557550695));
#85601=CARTESIAN_POINT('Ctrl Pts',(15.7600593435452,2.40149104209609,3.81388527036588));
#85602=CARTESIAN_POINT('Ctrl Pts',(15.8391831363984,2.37351593918905,3.80856496522481));
#85603=CARTESIAN_POINT('Ctrl Pts',(15.9183069292517,2.34554083628201,3.80324466008374));
#85604=CARTESIAN_POINT('Ctrl Pts',(15.9959131139442,2.31364644507584,3.79792435494268));
#85605=CARTESIAN_POINT('Ctrl Pts',(16.0716023793666,2.27804183248152,3.79260404980161));
#85606=CARTESIAN_POINT('Ctrl Pts',(16.1463865469486,2.24286298248101,3.78734736526337));
#85607=CARTESIAN_POINT('Ctrl Pts',(16.2195737593306,2.2039331554168,3.78209068072513));
#85608=CARTESIAN_POINT('Ctrl Pts',(16.2907629773018,2.16142017812991,3.7768339961869));
#85609=CARTESIAN_POINT('Ctrl Pts',(16.3618517072413,2.11896721056818,3.77158473178751));
#85610=CARTESIAN_POINT('Ctrl Pts',(16.4309476521906,2.07294137382628,3.76633546738813));
#85611=CARTESIAN_POINT('Ctrl Pts',(16.4976718256376,2.02355759806615,3.76108620298875));
#85612=CARTESIAN_POINT('Ctrl Pts',(16.5646740429046,1.97396803701193,3.75581506457504));
#85613=CARTESIAN_POINT('Ctrl Pts',(16.6292842504876,1.92099268733259,3.75054392616134));
#85614=CARTESIAN_POINT('Ctrl Pts',(16.6911457330465,1.86489473150598,3.74527278774764));
#85615=CARTESIAN_POINT('Ctrl Pts',(16.7526412611842,1.80912863476358,3.74003283184569));
#85616=CARTESIAN_POINT('Ctrl Pts',(16.8114201504743,1.75027708761682,3.73479287594374));
#85617=CARTESIAN_POINT('Ctrl Pts',(16.8671643238952,1.68863958190404,3.72955292004179));
#85618=CARTESIAN_POINT('Ctrl Pts',(16.9228903301959,1.62702216395834,3.72431467185031));
#85619=CARTESIAN_POINT('Ctrl Pts',(16.9755832758802,1.56262093247153,3.71907642365883));
#85620=CARTESIAN_POINT('Ctrl Pts',(17.0249628122788,1.49577132573392,3.71383817546735));
#85621=CARTESIAN_POINT('Ctrl Pts',(17.0743411265767,1.42892337346617,3.70860005691797));
#85622=CARTESIAN_POINT('Ctrl Pts',(17.1204059215362,1.35962753796808,3.70336193836859));
#85623=CARTESIAN_POINT('Ctrl Pts',(17.1629187734376,1.28825022007032,3.69812381981922));
#85624=CARTESIAN_POINT('Ctrl Pts',(17.2058966185215,1.21609219787433,3.69282840825595));
#85625=CARTESIAN_POINT('Ctrl Pts',(17.2452440836424,1.14180728564829,3.68753299669267));
#85626=CARTESIAN_POINT('Ctrl Pts',(17.2807622175225,1.06580014877178,3.6822375851294));
#85627=CARTESIAN_POINT('Ctrl Pts',(17.315946335045,0.990507791199236,3.67699197218698));
#85628=CARTESIAN_POINT('Ctrl Pts',(17.3473727228792,0.913525920142375,3.67174635924456));
#85629=CARTESIAN_POINT('Ctrl Pts',(17.3748969365347,0.835266897966168,3.66650074630214));
#85630=CARTESIAN_POINT('Ctrl Pts',(17.4028130971071,0.755893461302154,3.66118043542845));
#85631=CARTESIAN_POINT('Ctrl Pts',(17.4267149356507,0.675206685676165,3.65586012455475));
#85632=CARTESIAN_POINT('Ctrl Pts',(17.446504929017,0.593649629239103,3.65053981368105));
#85633=CARTESIAN_POINT('Ctrl Pts',(17.4662949223832,0.512092572802039,3.64521950280735));
#85634=CARTESIAN_POINT('Ctrl Pts',(17.4819730422611,0.42966572687241,3.63989919193365));
#85635=CARTESIAN_POINT('Ctrl Pts',(17.4934962775776,0.346817767288341,3.63457888105995));
#85636=CARTESIAN_POINT('Ctrl Pts',(17.5048817109381,0.26496055470899,3.62932219374546));
#85637=CARTESIAN_POINT('Ctrl Pts',(17.5122529109554,0.182391959997753,3.62406550643097));
#85638=CARTESIAN_POINT('Ctrl Pts',(17.5155313797586,0.0995395773032683,
3.61880881911649));
#85639=CARTESIAN_POINT('Ctrl Pts',(17.5188052208284,0.0168041451609522,
3.61355955189619));
#85640=CARTESIAN_POINT('Ctrl Pts',(17.51799778788,-0.0662138223184987,3.6083102846759));
#85641=CARTESIAN_POINT('Ctrl Pts',(17.5130820840236,-0.149079471959533,
3.60306101745561));
#85642=CARTESIAN_POINT('Ctrl Pts',(17.5081458994284,-0.232290372203708,
3.59778987974155));
#85643=CARTESIAN_POINT('Ctrl Pts',(17.4990670668675,-0.315347216186424,
3.59251874202749));
#85644=CARTESIAN_POINT('Ctrl Pts',(17.4858711721179,-0.397807447936076,
3.58724760431343));
#85645=CARTESIAN_POINT('Ctrl Pts',(17.4727533313952,-0.479779925480137,
3.58200764550263));
#85646=CARTESIAN_POINT('Ctrl Pts',(17.4555670725052,-0.561162369073261,
3.57676768669183));
#85647=CARTESIAN_POINT('Ctrl Pts',(17.4343895011345,-0.641524751483474,
3.57152772788102));
#85648=CARTESIAN_POINT('Ctrl Pts',(17.4132188314588,-0.721860944079876,
3.56628947675411));
#85649=CARTESIAN_POINT('Ctrl Pts',(17.3880595501687,-0.801177290203249,
3.56105122562719));
#85650=CARTESIAN_POINT('Ctrl Pts',(17.3590394817709,-0.879055728293861,
3.55581297450028));
#85651=CARTESIAN_POINT('Ctrl Pts',(17.3300201314689,-0.956932239297852,
3.55057485299286));
#85652=CARTESIAN_POINT('Ctrl Pts',(17.2971403460322,-1.03337048130383,3.54533673148544));
#85653=CARTESIAN_POINT('Ctrl Pts',(17.2605767866301,-1.10797059606703,3.54009860997801));
#85654=CARTESIAN_POINT('Ctrl Pts',(17.2236133504537,-1.18338657377524,3.53480320183969));
#85655=CARTESIAN_POINT('Ctrl Pts',(17.1828852681956,-1.25692353330891,3.52950779370137));
#85656=CARTESIAN_POINT('Ctrl Pts',(17.1386228133881,-1.328193778052,3.52421238556305));
#85657=CARTESIAN_POINT('Ctrl Pts',(17.0947765541762,-1.39879387555417,3.51896676963698));
#85658=CARTESIAN_POINT('Ctrl Pts',(17.0474624264169,-1.46716935843424,3.51372115371091));
#85659=CARTESIAN_POINT('Ctrl Pts',(16.9969469265273,-1.53297397976387,3.50847553778484));
#85660=CARTESIAN_POINT('Ctrl Pts',(16.9457121750204,-1.59971554283263,3.5031552335404));
#85661=CARTESIAN_POINT('Ctrl Pts',(16.8911844897076,-1.66381208525609,3.49783492929595));
#85662=CARTESIAN_POINT('Ctrl Pts',(16.8336817078274,-1.72493989587443,3.49251462505151));
#85663=CARTESIAN_POINT('Ctrl Pts',(16.7761789259471,-1.78606770649277,3.48719432080706));
#85664=CARTESIAN_POINT('Ctrl Pts',(16.7157014435654,-1.84422649320658,3.48187401656262));
#85665=CARTESIAN_POINT('Ctrl Pts',(16.6526015810124,-1.89913513590667,3.47655371231817));
#85666=CARTESIAN_POINT('Ctrl Pts',(16.5902562391359,-1.95338720497005,3.47129702595489));
#85667=CARTESIAN_POINT('Ctrl Pts',(16.5251222113034,-2.00466549670962,3.46604033959161));
#85668=CARTESIAN_POINT('Ctrl Pts',(16.4575147759546,-2.05267068178846,3.46078365322833));
#85669=CARTESIAN_POINT('Ctrl Pts',(16.3900027722482,-2.10060810488778,3.45553438696921));
#85670=CARTESIAN_POINT('Ctrl Pts',(16.3200246688988,-2.14528133377571,3.4502851207101));
#85671=CARTESIAN_POINT('Ctrl Pts',(16.2479299576488,-2.18643021173846,3.44503585445098));
#85672=CARTESIAN_POINT('Ctrl Pts',(16.1755348551851,-2.22775054140939,3.43976471649788));
#85673=CARTESIAN_POINT('Ctrl Pts',(16.1010058210992,-2.26551677418808,3.43449357854477));
#85674=CARTESIAN_POINT('Ctrl Pts',(16.0247275232926,-2.29950858946136,3.42922244059167));
#85675=CARTESIAN_POINT('Ctrl Pts',(15.9489004310018,-2.33329933450914,3.42398248275908));
#85676=CARTESIAN_POINT('Ctrl Pts',(15.8713451381114,-2.36336000218641,3.41874252492649));
#85677=CARTESIAN_POINT('Ctrl Pts',(15.7924639613833,-2.38952026982586,3.41350256709391));
#85678=CARTESIAN_POINT('Ctrl Pts',(15.7136084918173,-2.41567201190487,3.4082643169494));
#85679=CARTESIAN_POINT('Ctrl Pts',(15.633428433952,-2.43792573352404,3.4030260668049));
#85680=CARTESIAN_POINT('Ctrl Pts',(15.5523437876966,-2.45616013121965,3.39778781666039));
#85681=CARTESIAN_POINT('Ctrl Pts',(15.4712611479092,-2.4743940776987,3.39254969613822));
#85682=CARTESIAN_POINT('Ctrl Pts',(15.3892744143518,-2.48860879789434,3.38731157561605));
#85683=CARTESIAN_POINT('Ctrl Pts',(15.3068150171882,-2.49873383841253,3.38207345509388));
#85684=CARTESIAN_POINT('Ctrl Pts',(15.2234537703064,-2.50896961542955,3.37677804580076));
#85685=CARTESIAN_POINT('Ctrl Pts',(15.1396099329018,-2.51502563259169,3.37148263650765));
#85686=CARTESIAN_POINT('Ctrl Pts',(15.0557340353218,-2.51688298641529,3.36618722721453));
#85687=CARTESIAN_POINT('Ctrl Pts',(14.9726468483965,-2.51872287497422,3.36094161227058));
#85688=CARTESIAN_POINT('Ctrl Pts',(14.889528666218,-2.51644280600452,3.35569599732663));
#85689=CARTESIAN_POINT('Ctrl Pts',(14.806815086913,-2.51007685925263,3.35045038238268));
#85690=CARTESIAN_POINT('Ctrl Pts',(14.7229237613685,-2.50362026874055,3.34513007591498));
#85691=CARTESIAN_POINT('Ctrl Pts',(14.63944913927,-2.49296059172656,3.33980976944728));
#85692=CARTESIAN_POINT('Ctrl Pts',(14.5568359887859,-2.47818722237942,3.33448946297957));
#85693=CARTESIAN_POINT('Ctrl Pts',(14.4742228383017,-2.46341385303227,3.32916915651187));
#85694=CARTESIAN_POINT('Ctrl Pts',(14.392471620456,-2.44452696354054,3.32384885004417));
#85695=CARTESIAN_POINT('Ctrl Pts',(14.3120102652849,-2.42166809759857,3.31852854357646));
#85696=CARTESIAN_POINT('Ctrl Pts',(14.2325110658525,-2.39908257764982,3.31327185725769));
#85697=CARTESIAN_POINT('Ctrl Pts',(14.1539793922194,-2.37253675295542,3.30801517093892));
#85698=CARTESIAN_POINT('Ctrl Pts',(14.0768381915538,-2.3421311930433,3.30275848462015));
#85699=CARTESIAN_POINT('Ctrl Pts',(13.9998058800514,-2.31176855229686,3.29750921841111));
#85700=CARTESIAN_POINT('Ctrl Pts',(13.9241605683303,-2.27755716605228,3.29225995220207));
#85701=CARTESIAN_POINT('Ctrl Pts',(13.8503110814322,-2.239647659906,3.28701068599304));
#85702=CARTESIAN_POINT('Ctrl Pts',(13.7761538909645,-2.20158019883205,3.28173954802811));
#85703=CARTESIAN_POINT('Ctrl Pts',(13.7038079777237,-2.15978385808111,3.27646841006318));
#85704=CARTESIAN_POINT('Ctrl Pts',(13.6336680148729,-2.11446048826138,3.27119727209825));
#85705=CARTESIAN_POINT('Ctrl Pts',(13.563942948726,-2.06940521833771,3.26595731432901));
#85706=CARTESIAN_POINT('Ctrl Pts',(13.4963981989511,-2.02086478354645,3.26071735655978));
#85707=CARTESIAN_POINT('Ctrl Pts',(13.4313962005976,-1.96908312940322,3.25547739879054));
#85708=CARTESIAN_POINT('Ctrl Pts',(13.3664153862802,-1.9173183508093,3.25023914871426));
#85709=CARTESIAN_POINT('Ctrl Pts',(13.3039760379141,-1.862314737904,3.24500089863797));
#85710=CARTESIAN_POINT('Ctrl Pts',(13.2444091909891,-1.80435782518783,3.23976264856169));
#85711=CARTESIAN_POINT('Ctrl Pts',(13.1848438181212,-1.74640234668875,3.23452452811252));
#85712=CARTESIAN_POINT('Ctrl Pts',(13.1281511350965,-1.68549403602229,3.22928640766336));
#85713=CARTESIAN_POINT('Ctrl Pts',(13.0746258285682,-1.6219557792934,3.22404828721419));
#85714=CARTESIAN_POINT('Ctrl Pts',(13.020515119927,-1.55772260959435,3.21875287784924));
#85715=CARTESIAN_POINT('Ctrl Pts',(12.9696418177184,-1.49080197138715,3.21345746848428));
#85716=CARTESIAN_POINT('Ctrl Pts',(12.9222678633734,-1.42156090915204,3.20816205911932));
#85717=CARTESIAN_POINT('Ctrl Pts',(12.8753393821638,-1.35297094378045,3.2029164442595));
#85718=CARTESIAN_POINT('Ctrl Pts',(12.8318449052164,-1.28210444049809,3.19767082939967));
#85719=CARTESIAN_POINT('Ctrl Pts',(12.7919938375189,-1.20934487903391,3.19242521453984));
#85720=CARTESIAN_POINT('Ctrl Pts',(12.7515753346643,-1.1355493018347,3.18710490792232));
#85721=CARTESIAN_POINT('Ctrl Pts',(12.7149050271858,-1.05980677523672,3.1817846013048));
#85722=CARTESIAN_POINT('Ctrl Pts',(12.6821509971805,-0.982538676149113,
3.17646429468728));
#85723=CARTESIAN_POINT('Ctrl Pts',(12.6493969671752,-0.905270577061505,
3.17114398806976));
#85724=CARTESIAN_POINT('Ctrl Pts',(12.6205593222554,-0.826477385704819,
3.16582368145224));
#85725=CARTESIAN_POINT('Ctrl Pts',(12.5957532652842,-0.746594862430913,
3.16050337483472));
#85726=CARTESIAN_POINT('Ctrl Pts',(12.5660861567849,-0.651058377615517,
3.15414048879223));
#85727=CARTESIAN_POINT('Ctrl Pts',(12.542095602325,-0.553681574571601,3.14777760274975));
#85728=CARTESIAN_POINT('Ctrl Pts',(12.5239729173674,-0.455078164791567,
3.14141471670727));
#85729=CARTESIAN_POINT('Ctrl Pts',(12.5060754715587,-0.357700254883325,
3.13513091227105));
#85730=CARTESIAN_POINT('Ctrl Pts',(12.4939009850906,-0.25912605532082,3.12884710783484));
#85731=CARTESIAN_POINT('Ctrl Pts',(12.4875874665127,-0.159967220317441,
3.12256330339863));
#85732=CARTESIAN_POINT('Ctrl Pts',(12.4842450687784,-0.107472203257753,
3.11923663642975));
#85733=CARTESIAN_POINT('Ctrl Pts',(12.4825445281381,-0.0548136775673956,
3.11590996946086));
#85734=CARTESIAN_POINT('Ctrl Pts',(12.4825008631916,-0.00208474671008541,
3.11258330249198));
#85735=CARTESIAN_POINT('Ctrl Pts',(12.4841498434241,-0.00208338118583777,
3.11258330249198));
#85736=CARTESIAN_POINT('Ctrl Pts',(12.4865054906647,0.294763270002047,3.09384311542301));
#85737=CARTESIAN_POINT('Ctrl Pts',(12.5399868199015,0.592359670770662,3.07510292835405));
#85738=CARTESIAN_POINT('Ctrl Pts',(12.6408521577454,0.87179739374149,3.05636274128509));
#85739=CARTESIAN_POINT('',(12.4862285524092,0.000445657771908455,3.38754588178119));
#85740=CARTESIAN_POINT('Ctrl Pts',(12.6385710144774,0.872616408471391,3.32953357812844));
#85741=CARTESIAN_POINT('Ctrl Pts',(12.619021003094,0.819711187918733,3.33336697815837));
#85742=CARTESIAN_POINT('Ctrl Pts',(12.6012535156701,0.766161406554403,3.33724378078027));
#85743=CARTESIAN_POINT('Ctrl Pts',(12.5333054375905,0.535738690251715,3.35380928062876));
#85744=CARTESIAN_POINT('Ctrl Pts',(12.5007720780434,0.354226854504134,3.36651667217454));
#85745=CARTESIAN_POINT('Ctrl Pts',(12.4860719888631,0.138021323217801,3.38079977453777));
#85746=CARTESIAN_POINT('Ctrl Pts',(12.4844858769325,0.105227315747329,3.38294529035555));
#85747=CARTESIAN_POINT('Ctrl Pts',(12.4828528391001,0.0484748116459329,
3.38662256013421));
#85748=CARTESIAN_POINT('Ctrl Pts',(12.4825056181578,0.0245301016561651,
3.38816309378582));
#85749=CARTESIAN_POINT('Ctrl Pts',(12.4825000676272,0.000583526462428343,
3.38969315734209));
#85750=CARTESIAN_POINT('Ctrl Pts',(12.4864528653038,0.000437363323397832,
3.38741669750802));
#85751=CARTESIAN_POINT('Ctrl Pts',(12.4871507384439,-0.445065060869901,
3.41547689838276));
#85752=CARTESIAN_POINT('Ctrl Pts',(12.811943456554,-1.72782232442595,3.49621215550473));
#85753=CARTESIAN_POINT('Ctrl Pts',(14.8545655179616,-2.96733750069494,3.62962246887397));
#85754=CARTESIAN_POINT('Ctrl Pts',(17.4060396764084,-1.74276220584388,3.78764763761569));
#85755=CARTESIAN_POINT('Ctrl Pts',(17.7740900564321,1.06333051391069,3.94567280635744));
#85756=CARTESIAN_POINT('Ctrl Pts',(15.6247197032598,2.9044718341732,4.10369797509916));
#85757=CARTESIAN_POINT('Ctrl Pts',(13.4161781540431,2.25841240405204,4.23218400794579));
#85758=CARTESIAN_POINT('Ctrl Pts',(12.7683211668134,1.21621823547935,4.30799498454517));
#85759=CARTESIAN_POINT('Ctrl Pts',(12.6421214752944,0.871321765791516,4.3311309048973));
#85760=CARTESIAN_POINT('Origin',(15.,0.,3.));
#85761=CARTESIAN_POINT('',(12.6385710119932,0.872616401748846,5.33098034507765));
#85762=CARTESIAN_POINT('',(12.6385710119932,0.872616401748849,5.05624489442998));
#85763=CARTESIAN_POINT('',(12.6385710119932,0.872616401748847,3.));
#85764=CARTESIAN_POINT('',(12.4825004940191,0.00157714490144886,5.38741669754798));
#85765=CARTESIAN_POINT('Ctrl Pts',(12.6385710119932,0.872616401748844,5.33098034507765));
#85766=CARTESIAN_POINT('Ctrl Pts',(12.6098178284995,0.794806036434478,5.33622205618864));
#85767=CARTESIAN_POINT('Ctrl Pts',(12.5849432520214,0.715650777905113,5.34146376729964));
#85768=CARTESIAN_POINT('Ctrl Pts',(12.5640499918729,0.635573605419081,5.34670547841063));
#85769=CARTESIAN_POINT('Ctrl Pts',(12.543122884809,0.555366708550572,5.35195568105193));
#85770=CARTESIAN_POINT('Ctrl Pts',(12.5261900580931,0.47423536920686,5.35720588369323));
#85771=CARTESIAN_POINT('Ctrl Pts',(12.5133028738199,0.392611325164924,5.36245608633453));
#85772=CARTESIAN_POINT('Ctrl Pts',(12.508849203175,0.364402943786497,5.36427049923404));
#85773=CARTESIAN_POINT('Ctrl Pts',(12.5048782541387,0.336135744403197,5.36608491213355));
#85774=CARTESIAN_POINT('Ctrl Pts',(12.5013907003247,0.307827577673285,5.36789932503306));
#85775=CARTESIAN_POINT('Ctrl Pts',(12.4888856659904,0.206325316840848,5.37440511585805));
#85776=CARTESIAN_POINT('Ctrl Pts',(12.4825646917813,0.104052047516512,5.38091090668304));
#85777=CARTESIAN_POINT('Ctrl Pts',(12.4825004940195,0.00157714553074645,
5.38741669750803));
#85778=CARTESIAN_POINT('',(16.9134659966651,1.63598720337493,6.));
#85779=CARTESIAN_POINT('Ctrl Pts',(12.4825004940191,0.00157714490144911,
5.38741669754798));
#85780=CARTESIAN_POINT('Ctrl Pts',(12.4824492998181,-0.0801410127544445,
5.39260471168613));
#85781=CARTESIAN_POINT('Ctrl Pts',(12.4863811899288,-0.162011329145106,
5.39779272582428));
#85782=CARTESIAN_POINT('Ctrl Pts',(12.49431418367,-0.243607963422187,5.40298073996243));
#85783=CARTESIAN_POINT('Ctrl Pts',(12.5022364492358,-0.32509425058011,5.40816173809533));
#85784=CARTESIAN_POINT('Ctrl Pts',(12.5141490234632,-0.40630712270579,5.41334273622823));
#85785=CARTESIAN_POINT('Ctrl Pts',(12.5300179018197,-0.48682099859071,5.41852373436114));
#85786=CARTESIAN_POINT('Ctrl Pts',(12.5458749086248,-0.567274641824679,
5.42370085657515));
#85787=CARTESIAN_POINT('Ctrl Pts',(12.5656822570989,-0.647029863143335,
5.42887797878917));
#85788=CARTESIAN_POINT('Ctrl Pts',(12.5893542961562,-0.725667651572945,
5.43405510100318));
#85789=CARTESIAN_POINT('Ctrl Pts',(12.6130161888524,-0.804271734101949,
5.43923000418777));
#85790=CARTESIAN_POINT('Ctrl Pts',(12.6405393482842,-0.881758881203542,
5.44440490737236));
#85791=CARTESIAN_POINT('Ctrl Pts',(12.671787708573,-0.957723225179621,5.44957981055694));
#85792=CARTESIAN_POINT('Ctrl Pts',(12.7030326574948,-1.03367927616822,5.45475414880007));
#85793=CARTESIAN_POINT('Ctrl Pts',(12.7380018182631,-1.1081124165419,5.4599284870432));
#85794=CARTESIAN_POINT('Ctrl Pts',(12.7765107980518,-1.18063627710643,5.46510282528633));
#85795=CARTESIAN_POINT('Ctrl Pts',(12.815052983583,-1.25322267395869,5.47028162528732));
#85796=CARTESIAN_POINT('Ctrl Pts',(12.8571408635482,-1.32389608247715,5.47546042528831));
#85797=CARTESIAN_POINT('Ctrl Pts',(12.9025441613878,-1.39229495979536,5.48063922528931));
#85798=CARTESIAN_POINT('Ctrl Pts',(12.9479661610744,-1.46072201095558,5.4858201584641));
#85799=CARTESIAN_POINT('Ctrl Pts',(12.9967060167826,-1.5268722833105,5.49100109163889));
#85800=CARTESIAN_POINT('Ctrl Pts',(13.0484916987446,-1.59041554322488,5.49618202481368));
#85801=CARTESIAN_POINT('Ctrl Pts',(13.1003655936019,-1.65406704415733,5.50137178330657));
#85802=CARTESIAN_POINT('Ctrl Pts',(13.1552953616705,-1.71510230855825,5.50656154179945));
#85803=CARTESIAN_POINT('Ctrl Pts',(13.2129707216408,-1.77322660940077,5.51175130029234));
#85804=CARTESIAN_POINT('Ctrl Pts',(13.2654743874119,-1.82613895994677,5.51647569811982));
#85805=CARTESIAN_POINT('Ctrl Pts',(13.3202526773605,-1.87663928457784,5.52120009594731));
#85806=CARTESIAN_POINT('Ctrl Pts',(13.3770488316674,-1.9245352049801,5.5259244937748));
#85807=CARTESIAN_POINT('Ctrl Pts',(13.4403118562222,-1.97788460557705,5.53118681653968));
#85808=CARTESIAN_POINT('Ctrl Pts',(13.506321281188,-2.02820671259872,5.53644913930457));
#85809=CARTESIAN_POINT('Ctrl Pts',(13.5747557907899,-2.07520726533838,5.54171146206945));
#85810=CARTESIAN_POINT('Ctrl Pts',(13.6430952773156,-2.12214255660204,5.54696647796387));
#85811=CARTESIAN_POINT('Ctrl Pts',(13.7138527833007,-2.1657651971615,5.55222149385829));
#85812=CARTESIAN_POINT('Ctrl Pts',(13.7866735024611,-2.20582072262684,5.55747650975271));
#85813=CARTESIAN_POINT('Ctrl Pts',(13.8596979084428,-2.24598828739571,5.5627462244512));
#85814=CARTESIAN_POINT('Ctrl Pts',(13.9347967246319,-2.28256845733183,5.56801593914969));
#85815=CARTESIAN_POINT('Ctrl Pts',(14.0115823135293,-2.31534807903085,5.57328565384819));
#85816=CARTESIAN_POINT('Ctrl Pts',(14.0880214188612,-2.34797978755551,5.57853158974178));
#85817=CARTESIAN_POINT('Ctrl Pts',(14.1661316832303,-2.37684498621441,5.58377752563537));
#85818=CARTESIAN_POINT('Ctrl Pts',(14.2455071070187,-2.40177990757704,5.58902346152897));
#85819=CARTESIAN_POINT('Ctrl Pts',(14.3248577730842,-2.42670705157173,5.59426776118024));
#85820=CARTESIAN_POINT('Ctrl Pts',(14.4054723763626,-2.44770621550424,5.59951206083151));
#85821=CARTESIAN_POINT('Ctrl Pts',(14.4869280811847,-2.46466294980128,5.60475636048278));
#85822=CARTESIAN_POINT('Ctrl Pts',(14.5683827415137,-2.48161946666491,5.61000059288727));
#85823=CARTESIAN_POINT('Ctrl Pts',(14.6506780315082,-2.49453356438589,5.61524482529175));
#85824=CARTESIAN_POINT('Ctrl Pts',(14.7333805464554,-2.50334182983299,5.62048905769623));
#85825=CARTESIAN_POINT('Ctrl Pts',(14.8167793360512,-2.51222425229856,5.62577744143126));
#85826=CARTESIAN_POINT('Ctrl Pts',(14.9005917694087,-2.51693131427674,5.63106582516628));
#85827=CARTESIAN_POINT('Ctrl Pts',(14.9843695500362,-2.51745147699691,5.63635420890131));
#85828=CARTESIAN_POINT('Ctrl Pts',(15.0675679975995,-2.51796804273158,5.64160602284979));
#85829=CARTESIAN_POINT('Ctrl Pts',(15.1507318088343,-2.51435551447981,5.64685783679827));
#85830=CARTESIAN_POINT('Ctrl Pts',(15.2334251125323,-2.50665493573393,5.65210965074675));
#85831=CARTESIAN_POINT('Ctrl Pts',(15.3169821396488,-2.49887392520094,5.65741631937505));
#85832=CARTESIAN_POINT('Ctrl Pts',(15.4000582965981,-2.48691903614563,5.66272298800334));
#85833=CARTESIAN_POINT('Ctrl Pts',(15.4822143167678,-2.47088559077594,5.66802965663164));
#85834=CARTESIAN_POINT('Ctrl Pts',(15.5643703369375,-2.45485214540624,5.67333632525993));
#85835=CARTESIAN_POINT('Ctrl Pts',(15.6456057716764,-2.43474031903382,5.67864299388823));
#85836=CARTESIAN_POINT('Ctrl Pts',(15.7254987058856,-2.41069655447515,5.68394966251653));
#85837=CARTESIAN_POINT('Ctrl Pts',(15.8038445324732,-2.38711839168426,5.68915356877214));
#85838=CARTESIAN_POINT('Ctrl Pts',(15.8811999880898,-2.35966860286573,5.69435747502775));
#85839=CARTESIAN_POINT('Ctrl Pts',(15.9571497439144,-2.3284481135994,5.69956138128336));
#85840=CARTESIAN_POINT('Ctrl Pts',(16.0329908326933,-2.29727229384249,5.70475784191768));
#85841=CARTESIAN_POINT('Ctrl Pts',(16.1074297825892,-2.26233666105182,5.70995430255201));
#85842=CARTESIAN_POINT('Ctrl Pts',(16.180065591005,-2.22379213302998,5.71515076318633));
#85843=CARTESIAN_POINT('Ctrl Pts',(16.2539297182706,-2.18459579192366,5.72043509935599));
#85844=CARTESIAN_POINT('Ctrl Pts',(16.3259286754122,-2.14166749400403,5.72571943552566));
#85845=CARTESIAN_POINT('Ctrl Pts',(16.3956613162591,-2.09521734917831,5.73100377169532));
#85846=CARTESIAN_POINT('Ctrl Pts',(16.4641153205206,-2.04961892678639,5.73619121284603));
#85847=CARTESIAN_POINT('Ctrl Pts',(16.5303850131159,-2.00062700045551,5.74137865399674));
#85848=CARTESIAN_POINT('Ctrl Pts',(16.5941168644065,-1.94848599497531,5.74656609514745));
#85849=CARTESIAN_POINT('Ctrl Pts',(16.6578303083121,-1.89636004914801,5.75175203803278));
#85850=CARTESIAN_POINT('Ctrl Pts',(16.7190070011472,-1.84108712751668,5.75693798091811));
#85851=CARTESIAN_POINT('Ctrl Pts',(16.77732537827,-1.78295281759144,5.76212392380345));
#85852=CARTESIAN_POINT('Ctrl Pts',(16.8356453429613,-1.72481692510858,5.76731000786278));
#85853=CARTESIAN_POINT('Ctrl Pts',(16.8911065044959,-1.66381982325704,5.77249609192212));
#85854=CARTESIAN_POINT('Ctrl Pts',(16.9434242521823,-1.60028385795444,5.77768217598146));
#85855=CARTESIAN_POINT('Ctrl Pts',(16.9974734936777,-1.53464512379362,5.78303989725453));
#85856=CARTESIAN_POINT('Ctrl Pts',(17.0481672504167,-1.46629693281038,5.7883976185276));
#85857=CARTESIAN_POINT('Ctrl Pts',(17.0952383407115,-1.39562980249503,5.79375533980066));
#85858=CARTESIAN_POINT('Ctrl Pts',(17.1408776398397,-1.32711219904057,5.79895009187237));
#85859=CARTESIAN_POINT('Ctrl Pts',(17.1831113188493,-1.25641515828611,5.80414484394408));
#85860=CARTESIAN_POINT('Ctrl Pts',(17.2217422455258,-1.18392045528663,5.80933959601579));
#85861=CARTESIAN_POINT('Ctrl Pts',(17.262191060096,-1.10801430828925,5.81477880188954));
#85862=CARTESIAN_POINT('Ctrl Pts',(17.2986894609775,-1.03013768849094,5.82021800776328));
#85863=CARTESIAN_POINT('Ctrl Pts',(17.3310682049762,-0.950750899946465,
5.82565721363703));
#85864=CARTESIAN_POINT('Ctrl Pts',(17.3634469489749,-0.871364111401987,
5.83109641951078));
#85865=CARTESIAN_POINT('Ctrl Pts',(17.3917059305147,-0.790467733661366,
5.83653562538452));
#85866=CARTESIAN_POINT('Ctrl Pts',(17.415736476975,-0.708536183841481,5.84197483125827));
#85867=CARTESIAN_POINT('Ctrl Pts',(17.4395912944092,-0.627203777760307,
5.84737426165907));
#85868=CARTESIAN_POINT('Ctrl Pts',(17.4593704891542,-0.54454292061888,5.85277369205987));
#85869=CARTESIAN_POINT('Ctrl Pts',(17.4749339320301,-0.46098620596046,5.85817312246068));
#85870=CARTESIAN_POINT('Ctrl Pts',(17.4904730039907,-0.377560333406624,
5.86356409785173));
#85871=CARTESIAN_POINT('Ctrl Pts',(17.501809375636,-0.293241813948646,5.86895507324279));
#85872=CARTESIAN_POINT('Ctrl Pts',(17.5088530313989,-0.208477137452827,
5.87434604863384));
#85873=CARTESIAN_POINT('Ctrl Pts',(17.5158856497004,-0.123845287840876,
5.87972857632602));
#85874=CARTESIAN_POINT('Ctrl Pts',(17.518638909606,-0.0387691001167128,
5.8851111040182));
#85875=CARTESIAN_POINT('Ctrl Pts',(17.5170742549287,0.0462973560269238,
5.89049363171038));
#85876=CARTESIAN_POINT('Ctrl Pts',(17.5155110459009,0.131285215735854,5.89587118626149));
#85877=CARTESIAN_POINT('Ctrl Pts',(17.5096378635764,0.216262932944203,5.90124874081261));
#85878=CARTESIAN_POINT('Ctrl Pts',(17.4994681446226,0.30077440718398,5.90662629536372));
#85879=CARTESIAN_POINT('Ctrl Pts',(17.4893053914714,0.3852279948445,5.91200016653053));
#85880=CARTESIAN_POINT('Ctrl Pts',(17.4748520068441,0.46921554822398,5.91737403769734));
#85881=CARTESIAN_POINT('Ctrl Pts',(17.4561733372392,0.552285059942274,5.92274790886415));
#85882=CARTESIAN_POINT('Ctrl Pts',(17.4375030019987,0.635317506301934,5.92811938222631));
#85883=CARTESIAN_POINT('Ctrl Pts',(17.4146112278296,0.717432306497981,5.93349085558846));
#85884=CARTESIAN_POINT('Ctrl Pts',(17.3876144534637,0.798187616798997,5.93886232895061));
#85885=CARTESIAN_POINT('Ctrl Pts',(17.3606154325272,0.878949647254824,5.94423424930668));
#85886=CARTESIAN_POINT('Ctrl Pts',(17.3295108558663,0.958351550047946,5.94960616966276));
#85887=CARTESIAN_POINT('Ctrl Pts',(17.2944668662793,1.03596720486042,5.95497809001883));
#85888=CARTESIAN_POINT('Ctrl Pts',(17.2594234455537,1.11358159975507,5.9603499231737));
#85889=CARTESIAN_POINT('Ctrl Pts',(17.2204409219351,1.18940941409572,5.96572175632857));
#85890=CARTESIAN_POINT('Ctrl Pts',(17.1777327734932,1.26304640344432,5.97109358948344));
#85891=CARTESIAN_POINT('Ctrl Pts',(17.1349938295841,1.33673649004879,5.97646929609379));
#85892=CARTESIAN_POINT('Ctrl Pts',(17.0885241134416,1.40823222428896,5.98184500270414));
#85893=CARTESIAN_POINT('Ctrl Pts',(17.038581909391,1.47715606782208,5.98722070931449));
#85894=CARTESIAN_POINT('Ctrl Pts',(16.9990072085316,1.53177200922393,5.99148047287632));
#85895=CARTESIAN_POINT('Ctrl Pts',(16.9572530041006,1.58477350827339,5.99574023643816));
#85896=CARTESIAN_POINT('Ctrl Pts',(16.9134659966651,1.63598720337492,6.));
#85897=CARTESIAN_POINT('',(13.0863257750576,1.63574362624191,5.99999801595942));
#85898=CARTESIAN_POINT('Origin',(15.,0.,6.));
#85899=CARTESIAN_POINT('',(12.4825005975625,0.00173456822324663,5.11258330243344));
#85900=CARTESIAN_POINT('Ctrl Pts',(13.0863257750576,1.63574362624191,5.99999801595942));
#85901=CARTESIAN_POINT('Ctrl Pts',(13.1398047889163,1.6983093050897,5.99476345326225));
#85902=CARTESIAN_POINT('Ctrl Pts',(13.1964569730435,1.75836839630831,5.98952889056507));
#85903=CARTESIAN_POINT('Ctrl Pts',(13.2560173944066,1.81558005094452,5.9842943278679));
#85904=CARTESIAN_POINT('Ctrl Pts',(13.3154940880969,1.87271127971086,5.97906712371088));
#85905=CARTESIAN_POINT('Ctrl Pts',(13.377870567159,1.92700270143622,5.97383991955386));
#85906=CARTESIAN_POINT('Ctrl Pts',(13.4428421932686,1.97814706605332,5.96861271539685));
#85907=CARTESIAN_POINT('Ctrl Pts',(13.5077407467043,2.0292339093231,5.96339139020281));
#85908=CARTESIAN_POINT('Ctrl Pts',(13.5752282830167,2.07718044289211,5.95817006500876));
#85909=CARTESIAN_POINT('Ctrl Pts',(13.644965012631,2.12171780239641,5.95294873981472));
#85910=CARTESIAN_POINT('Ctrl Pts',(13.7146592101118,2.16622799875545,5.94773059908461));
#85911=CARTESIAN_POINT('Ctrl Pts',(13.7865994867435,2.20733289832195,5.94251245835449));
#85912=CARTESIAN_POINT('Ctrl Pts',(13.8604157788461,2.2448060167634,5.93729431762437));
#85913=CARTESIAN_POINT('Ctrl Pts',(13.9342097789858,2.28226781860593,5.93207775273337));
#85914=CARTESIAN_POINT('Ctrl Pts',(14.0098782547165,2.31609980690116,5.92686118784237));
#85915=CARTESIAN_POINT('Ctrl Pts',(14.0870264325652,2.34612137690389,5.92164462295136));
#85916=CARTESIAN_POINT('Ctrl Pts',(14.16417506616,2.37614312425642,5.91642802724396));
#85917=CARTESIAN_POINT('Ctrl Pts',(14.242802984838,2.40235424144356,5.91121143153655));
#85918=CARTESIAN_POINT('Ctrl Pts',(14.3224966766949,2.42462275352488,5.90599483582915));
#85919=CARTESIAN_POINT('Ctrl Pts',(14.4022672076388,2.44691273646664,5.90077321038298));
#85920=CARTESIAN_POINT('Ctrl Pts',(14.4831051146794,2.46525239736934,5.89555158493682));
#85921=CARTESIAN_POINT('Ctrl Pts',(14.5645835897953,2.47956020288366,5.89032995949065));
#85922=CARTESIAN_POINT('Ctrl Pts',(14.6461022933234,2.49387507259865,5.88510575596849));
#85923=CARTESIAN_POINT('Ctrl Pts',(14.7282617325478,2.50415406503659,5.87988155244634));
#85924=CARTESIAN_POINT('Ctrl Pts',(14.810629266729,2.51036749807282,5.87465734892418));
#85925=CARTESIAN_POINT('Ctrl Pts',(14.8931361053126,2.51659143960108,5.86942430994813));
#85926=CARTESIAN_POINT('Ctrl Pts',(14.9758512759986,2.51873607618652,5.86419127097209));
#85927=CARTESIAN_POINT('Ctrl Pts',(15.0583417354306,2.51682388972827,5.85895823199605));
#85928=CARTESIAN_POINT('Ctrl Pts',(15.1215371250673,2.51535897646292,5.85494923581211));
#85929=CARTESIAN_POINT('Ctrl Pts',(15.1846006139742,2.51151419625709,5.85094023962817));
#85930=CARTESIAN_POINT('Ctrl Pts',(15.2473407751248,2.50532009750464,5.84693124344423));
#85931=CARTESIAN_POINT('Ctrl Pts',(15.3297418431585,2.49718495179657,5.84166594668308));
#85932=CARTESIAN_POINT('Ctrl Pts',(15.4118865717943,2.48496584586104,5.83640064992194));
#85933=CARTESIAN_POINT('Ctrl Pts',(15.493339607283,2.4686883727773,5.83113535316079));
#85934=CARTESIAN_POINT('Ctrl Pts',(15.5746805746141,2.4524332952545,5.82587730072276));
#85935=CARTESIAN_POINT('Ctrl Pts',(15.6553312924422,2.43213103240371,5.82061924828473));
#85936=CARTESIAN_POINT('Ctrl Pts',(15.7348616424701,2.40785892784982,5.81536119584669));
#85937=CARTESIAN_POINT('Ctrl Pts',(15.8145570252977,2.38353645644398,5.81009223246568));
#85938=CARTESIAN_POINT('Ctrl Pts',(15.8931269243526,2.35522770936555,5.80482326908468));
#85939=CARTESIAN_POINT('Ctrl Pts',(15.9701489144374,2.32306205982879,5.79955430570367));
#85940=CARTESIAN_POINT('Ctrl Pts',(16.0468806290134,2.29101763411754,5.79430519965204));
#85941=CARTESIAN_POINT('Ctrl Pts',(16.1220756512209,2.25514549385421,5.78905609360041));
#85942=CARTESIAN_POINT('Ctrl Pts',(16.1953332573609,2.21562285911819,5.78380698754878));
#85943=CARTESIAN_POINT('Ctrl Pts',(16.2685686428395,2.17611221247635,5.77855947366777));
#85944=CARTESIAN_POINT('Ctrl Pts',(16.3398673755929,2.13295348875128,5.77331195978675));
#85945=CARTESIAN_POINT('Ctrl Pts',(16.4088523767563,2.08637034835815,5.76806444590574));
#85946=CARTESIAN_POINT('Ctrl Pts',(16.4778370250932,2.03978744621633,5.76281695886335));
#85947=CARTESIAN_POINT('Ctrl Pts',(16.544507585392,1.98978042028937,5.75756947182095));
#85948=CARTESIAN_POINT('Ctrl Pts',(16.6085162169142,1.93661607705915,5.75232198477855));
#85949=CARTESIAN_POINT('Ctrl Pts',(16.6729782725596,1.88307512843776,5.74703732560555));
#85950=CARTESIAN_POINT('Ctrl Pts',(16.7347401635969,1.82633224283836,5.74175266643254));
#85951=CARTESIAN_POINT('Ctrl Pts',(16.793482116325,1.76669979012352,5.73646800725954));
#85952=CARTESIAN_POINT('Ctrl Pts',(16.8518959264495,1.70740045449759,5.73121286909732));
#85953=CARTESIAN_POINT('Ctrl Pts',(16.9073231858939,1.64524413625105,5.72595773093509));
#85954=CARTESIAN_POINT('Ctrl Pts',(16.9594891797343,1.58057217630327,5.72070259277287));
#85955=CARTESIAN_POINT('Ctrl Pts',(17.0120947413328,1.51535526922907,5.71540317309448));
#85956=CARTESIAN_POINT('Ctrl Pts',(17.0613835376696,1.44758051073455,5.71010375341608));
#85957=CARTESIAN_POINT('Ctrl Pts',(17.1071187672171,1.37762721766134,5.70480433373768));
#85958=CARTESIAN_POINT('Ctrl Pts',(17.1528539967647,1.30767392458814,5.69950491405929));
#85959=CARTESIAN_POINT('Ctrl Pts',(17.1950354743649,1.23554253582845,5.69420549438089));
#85960=CARTESIAN_POINT('Ctrl Pts',(17.2334747450077,1.16163540468297,5.68890607470249));
#85961=CARTESIAN_POINT('Ctrl Pts',(17.2715585648948,1.08841169820112,5.68365565914663));
#85962=CARTESIAN_POINT('Ctrl Pts',(17.3061091309926,1.01317570439733,5.67840524359078));
#85963=CARTESIAN_POINT('Ctrl Pts',(17.3369089490488,0.936302736221347,5.67315482803492));
#85964=CARTESIAN_POINT('Ctrl Pts',(17.3676647212905,0.859539701567974,5.66791192092697));
#85965=CARTESIAN_POINT('Ctrl Pts',(17.3946802284794,0.781144767706604,5.66266901381902));
#85966=CARTESIAN_POINT('Ctrl Pts',(17.4177840102534,0.701517447938976,5.65742610671107));
#85967=CARTESIAN_POINT('Ctrl Pts',(17.4410191531688,0.621437391225072,5.65215339001314));
#85968=CARTESIAN_POINT('Ctrl Pts',(17.4602977226381,0.540111307931608,5.64688067331521));
#85969=CARTESIAN_POINT('Ctrl Pts',(17.4754946440225,0.457965629077161,5.64160795661728));
#85970=CARTESIAN_POINT('Ctrl Pts',(17.4905783331584,0.376432017606484,5.63637452692701));
#85971=CARTESIAN_POINT('Ctrl Pts',(17.5016409083356,0.294091444263798,5.63114109723675));
#85972=CARTESIAN_POINT('Ctrl Pts',(17.5086106325315,0.211373944349393,5.62590766754648));
#85973=CARTESIAN_POINT('Ctrl Pts',(17.5155780170051,0.128684212532012,5.62067599470795));
#85974=CARTESIAN_POINT('Ctrl Pts',(17.5184552403201,0.04561826581733,5.61544432186942));
#85975=CARTESIAN_POINT('Ctrl Pts',(17.5172223543771,-0.0373880813133137,
5.61021264903089));
#85976=CARTESIAN_POINT('Ctrl Pts',(17.5159895085048,-0.12039173061044,5.60498114622975));
#85977=CARTESIAN_POINT('Ctrl Pts',(17.5106468268508,-0.203335321846842,
5.5997496434286));
#85978=CARTESIAN_POINT('Ctrl Pts',(17.5012264746769,-0.285783786060985,
5.59451814062746));
#85979=CARTESIAN_POINT('Ctrl Pts',(17.4916771924292,-0.369360667385267,
5.58921503773857));
#85980=CARTESIAN_POINT('Ctrl Pts',(17.4779378138276,-0.452428279455892,
5.58391193484967));
#85981=CARTESIAN_POINT('Ctrl Pts',(17.4600958703531,-0.534541447103558,
5.57860883196078));
#85982=CARTESIAN_POINT('Ctrl Pts',(17.4424697166931,-0.615661495070169,
5.57336986757732));
#85983=CARTESIAN_POINT('Ctrl Pts',(17.4208398793822,-0.69584962456979,5.56813090319387));
#85984=CARTESIAN_POINT('Ctrl Pts',(17.3953412717723,-0.774691191213783,
5.56289193881041));
#85985=CARTESIAN_POINT('Ctrl Pts',(17.3693744105736,-0.854980595602245,
5.5575567666688));
#85986=CARTESIAN_POINT('Ctrl Pts',(17.3393954443895,-0.933873015488072,
5.55222159452719));
#85987=CARTESIAN_POINT('Ctrl Pts',(17.3055976313624,-1.01095292286836,5.54688642238558));
#85988=CARTESIAN_POINT('Ctrl Pts',(17.2717998183353,-1.08803283024865,5.54155125024397));
#85989=CARTESIAN_POINT('Ctrl Pts',(17.2341834407507,-1.16329980809554,5.53621607810236));
#85990=CARTESIAN_POINT('Ctrl Pts',(17.1929892410661,-1.23636743671465,5.53088090596074));
#85991=CARTESIAN_POINT('Ctrl Pts',(17.1523913371662,-1.30837739412583,5.52562296169788));
#85992=CARTESIAN_POINT('Ctrl Pts',(17.1081686274721,-1.37851725625535,5.52036501743502));
#85993=CARTESIAN_POINT('Ctrl Pts',(17.0605182013148,-1.44639931970747,5.51510707317216));
#85994=CARTESIAN_POINT('Ctrl Pts',(17.0129349748039,-1.51418565157814,5.50985654399502));
#85995=CARTESIAN_POINT('Ctrl Pts',(16.9619338964915,-1.57972013542936,5.50460601481788));
#85996=CARTESIAN_POINT('Ctrl Pts',(16.9077573997971,-1.64264054300363,5.49935548564074));
#85997=CARTESIAN_POINT('Ctrl Pts',(16.8533715070376,-1.70580414248893,5.49408466278983));
#85998=CARTESIAN_POINT('Ctrl Pts',(16.7957858292548,-1.76633300679217,5.48881383993893));
#85999=CARTESIAN_POINT('Ctrl Pts',(16.7352890092242,-1.82389097932569,5.48354301708802));
#86000=CARTESIAN_POINT('Ctrl Pts',(16.6751319233483,-1.88112572149542,5.47830179378541));
#86001=CARTESIAN_POINT('Ctrl Pts',(16.6120966418765,-1.93542252986321,5.4730605704828));
#86002=CARTESIAN_POINT('Ctrl Pts',(16.5465054206629,-1.98648615244613,5.46781934718018));
#86003=CARTESIAN_POINT('Ctrl Pts',(16.4809355946334,-2.03753311859876,5.46257983351089));
#86004=CARTESIAN_POINT('Ctrl Pts',(16.4128118481274,-2.08534871074164,5.45734031984159));
#86005=CARTESIAN_POINT('Ctrl Pts',(16.3424895048318,-2.12967795204261,5.4521008061723));
#86006=CARTESIAN_POINT('Ctrl Pts',(16.2721689511846,-2.17400606519929,5.4468614258445));
#86007=CARTESIAN_POINT('Ctrl Pts',(16.1996503024337,-2.21484775908183,5.4416220455167));
#86008=CARTESIAN_POINT('Ctrl Pts',(16.125316673362,-2.25199214799997,5.4363826651889));
#86009=CARTESIAN_POINT('Ctrl Pts',(16.0502093959688,-2.28952312767786,5.43108875452475));
#86010=CARTESIAN_POINT('Ctrl Pts',(15.9732495593644,-2.32327916190359,5.42579484386059));
#86011=CARTESIAN_POINT('Ctrl Pts',(15.8948548793404,-2.35309179483517,5.42050093319643));
#86012=CARTESIAN_POINT('Ctrl Pts',(15.8171570581821,-2.3826394200193,5.41525408068187));
#86013=CARTESIAN_POINT('Ctrl Pts',(15.7380502635238,-2.40831338687226,5.41000722816731));
#86014=CARTESIAN_POINT('Ctrl Pts',(15.6579565276493,-2.4299998884205,5.40476037565274));
#86015=CARTESIAN_POINT('Ctrl Pts',(15.5767852706341,-2.45197814391967,5.39944293591379));
#86016=CARTESIAN_POINT('Ctrl Pts',(15.4946007979303,-2.46986074220205,5.39412549617483));
#86017=CARTESIAN_POINT('Ctrl Pts',(15.4118512759015,-2.48358305207181,5.38880805643588));
#86018=CARTESIAN_POINT('Ctrl Pts',(15.3291017538727,-2.49730536194156,5.38349061669692));
#86019=CARTESIAN_POINT('Ctrl Pts',(15.2457876724258,-2.50686739103449,5.37817317695797));
#86020=CARTESIAN_POINT('Ctrl Pts',(15.1623588078343,-2.51225911631715,5.37285573721902));
#86021=CARTESIAN_POINT('Ctrl Pts',(15.0798682633806,-2.5175902011436,5.3675981024506));
#86022=CARTESIAN_POINT('Ctrl Pts',(14.9969642259103,-2.51886382988772,5.36234046768219));
#86023=CARTESIAN_POINT('Ctrl Pts',(14.9140790773331,-2.5160333553131,5.35708283291378));
#86024=CARTESIAN_POINT('Ctrl Pts',(14.8313105765977,-2.51320686418733,5.35183259744137));
#86025=CARTESIAN_POINT('Ctrl Pts',(14.7485613688306,-2.50628775833595,5.34658236196896));
#86026=CARTESIAN_POINT('Ctrl Pts',(14.6662672594009,-2.49528128832246,5.34133212649656));
#86027=CARTESIAN_POINT('Ctrl Pts',(14.5836492740316,-2.4842315013469,5.33606122824575));
#86028=CARTESIAN_POINT('Ctrl Pts',(14.5014904461928,-2.46906207896666,5.33079032999495));
#86029=CARTESIAN_POINT('Ctrl Pts',(14.4202300646622,-2.44983123338698,5.32551943174415));
#86030=CARTESIAN_POINT('Ctrl Pts',(14.3394310705388,-2.43070957840935,5.3202784610673));
#86031=CARTESIAN_POINT('Ctrl Pts',(14.2595208004982,-2.40757260462149,5.31503749039045));
#86032=CARTESIAN_POINT('Ctrl Pts',(14.1809225467008,-2.3805290116898,5.3097965197136));
#86033=CARTESIAN_POINT('Ctrl Pts',(14.1023496903866,-2.35349415736448,5.30455724255358));
#86034=CARTESIAN_POINT('Ctrl Pts',(14.0250884437906,-2.32255534094759,5.29931796539356));
#86035=CARTESIAN_POINT('Ctrl Pts',(13.9495464172445,-2.28787095800358,5.29407868823354));
#86036=CARTESIAN_POINT('Ctrl Pts',(13.8740060750566,-2.25318734841612,5.28883952789351));
#86037=CARTESIAN_POINT('Ctrl Pts',(13.8001852951159,-2.21475853167456,5.28360036755348));
#86038=CARTESIAN_POINT('Ctrl Pts',(13.7284699269289,-2.17279026214585,5.27836120721345));
#86039=CARTESIAN_POINT('Ctrl Pts',(13.6560008852565,-2.13038093831074,5.27306698731877));
#86040=CARTESIAN_POINT('Ctrl Pts',(13.5856821914247,-2.08435755731284,5.26777276742409));
#86041=CARTESIAN_POINT('Ctrl Pts',(13.5178831491532,-2.03497810564045,5.26247854752941));
#86042=CARTESIAN_POINT('Ctrl Pts',(13.4506929680101,-1.98604210018288,5.25723187173846));
#86043=CARTESIAN_POINT('Ctrl Pts',(13.385977688935,-1.93381040068355,5.25198519594752));
#86044=CARTESIAN_POINT('Ctrl Pts',(13.3240630831332,-1.87857437986441,5.24673852015657));
#86045=CARTESIAN_POINT('Ctrl Pts',(13.2613068946155,-1.82258755590581,5.24142052821002));
#86046=CARTESIAN_POINT('Ctrl Pts',(13.2014284377852,-1.76351446736911,5.23610253626347));
#86047=CARTESIAN_POINT('Ctrl Pts',(13.1447266726257,-1.70169536954578,5.23078454431692));
#86048=CARTESIAN_POINT('Ctrl Pts',(13.0880249074662,-1.63987627172245,5.22546655237037));
#86049=CARTESIAN_POINT('Ctrl Pts',(13.034500095191,-1.57531157960346,5.22014856042382));
#86050=CARTESIAN_POINT('Ctrl Pts',(12.9844062983381,-1.50837272576141,5.21483056847728));
#86051=CARTESIAN_POINT('Ctrl Pts',(12.9347409969261,-1.44200645765842,5.20955806590161));
#86052=CARTESIAN_POINT('Ctrl Pts',(12.8882642141893,-1.37306074742762,5.20428556332595));
#86053=CARTESIAN_POINT('Ctrl Pts',(12.8452534888802,-1.30187315926588,5.19901306075028));
#86054=CARTESIAN_POINT('Ctrl Pts',(12.8023036373243,-1.23078632401286,5.19374802043011));
#86055=CARTESIAN_POINT('Ctrl Pts',(12.7628103357478,-1.15746429922706,5.18848298010994));
#86056=CARTESIAN_POINT('Ctrl Pts',(12.7270097454968,-1.08227609829163,5.18321793978977));
#86057=CARTESIAN_POINT('Ctrl Pts',(12.6912492744183,-1.00717215541974,5.17795879962542));
#86058=CARTESIAN_POINT('Ctrl Pts',(12.659173489575,-0.930206601019301,5.17269965946107));
#86059=CARTESIAN_POINT('Ctrl Pts',(12.6309735430406,-0.851774557160795,
5.16744051929673));
#86060=CARTESIAN_POINT('Ctrl Pts',(12.6027972054207,-0.77340817638473,5.16218578206946));
#86061=CARTESIAN_POINT('Ctrl Pts',(12.5784904108169,-0.69357817516063,5.1569310448422));
#86062=CARTESIAN_POINT('Ctrl Pts',(12.5581963739879,-0.612700009788105,
5.15167630761493));
#86063=CARTESIAN_POINT('Ctrl Pts',(12.5379122956235,-0.531861532051385,
5.14642414893401));
#86064=CARTESIAN_POINT('Ctrl Pts',(12.5216371714886,-0.449976355376292,
5.14117199025308));
#86065=CARTESIAN_POINT('Ctrl Pts',(12.5094641290169,-0.367474251270026,
5.13591983157216));
#86066=CARTESIAN_POINT('Ctrl Pts',(12.4972912357025,-0.284973158068802,
5.13066773724636));
#86067=CARTESIAN_POINT('Ctrl Pts',(12.4892203979113,-0.201855603551131,
5.12541564292057));
#86068=CARTESIAN_POINT('Ctrl Pts',(12.4852932836739,-0.118559608908535,
5.12016354859477));
#86069=CARTESIAN_POINT('Ctrl Pts',(12.4834039743466,-0.0784864431958992,
5.11763679989384));
#86070=CARTESIAN_POINT('Ctrl Pts',(12.4824729639348,-0.038372057539079,
5.11511005119291));
#86071=CARTESIAN_POINT('Ctrl Pts',(12.4825005975619,0.00173456729401744,
5.11258330249198));
#86072=CARTESIAN_POINT('Ctrl Pts',(12.4825005975625,0.00173456822324807,
5.11258330243344));
#86073=CARTESIAN_POINT('Ctrl Pts',(12.4825660917933,0.0967908966663681,
5.10659467947122));
#86074=CARTESIAN_POINT('Ctrl Pts',(12.4880193463078,0.191635955587718,5.10060605650901));
#86075=CARTESIAN_POINT('Ctrl Pts',(12.4987647943891,0.285707361144845,5.09461743354679));
#86076=CARTESIAN_POINT('Ctrl Pts',(12.5100725482397,0.384701492462413,5.08831542791158));
#86077=CARTESIAN_POINT('Ctrl Pts',(12.5272411438782,0.482838514846412,5.08201342227637));
#86078=CARTESIAN_POINT('Ctrl Pts',(12.5501013634223,0.579485047688556,5.07571141664117));
#86079=CARTESIAN_POINT('Ctrl Pts',(12.5729615829664,0.676131580530701,5.06940941100596));
#86080=CARTESIAN_POINT('Ctrl Pts',(12.6015132358442,0.771287443638239,5.06310740537075));
#86081=CARTESIAN_POINT('Ctrl Pts',(12.6355307871045,0.864344602151889,5.05680539973555));
#86082=CARTESIAN_POINT('Ctrl Pts',(12.6365393029679,0.867103460949512,5.05661856463369));
#86083=CARTESIAN_POINT('Ctrl Pts',(12.6375527128651,0.86986073376603,5.05643172953183));
#86084=CARTESIAN_POINT('Ctrl Pts',(12.6385710119932,0.872616401748855,5.05624489442998));
#86085=CARTESIAN_POINT('Origin',(15.,0.,3.));
#86086=CARTESIAN_POINT('',(12.4825000279491,0.000375131315902114,4.11258330252632));
#86087=CARTESIAN_POINT('Ctrl Pts',(12.6385710119932,0.872616401748855,5.05624489442998));
#86088=CARTESIAN_POINT('Ctrl Pts',(12.6672209705858,0.950147425220547,5.05098826817542));
#86089=CARTESIAN_POINT('Ctrl Pts',(12.6997453794103,1.02640706388388,5.04573164192086));
#86090=CARTESIAN_POINT('Ctrl Pts',(12.7360110065744,1.10098142021001,5.0404750156663));
#86091=CARTESIAN_POINT('Ctrl Pts',(12.7722258857873,1.17545142163892,5.03522574522036));
#86092=CARTESIAN_POINT('Ctrl Pts',(12.8121713842627,1.24824041385453,5.02997647477441));
#86093=CARTESIAN_POINT('Ctrl Pts',(12.8556654677086,1.31895248724981,5.02472720432846));
#86094=CARTESIAN_POINT('Ctrl Pts',(12.8991472891697,1.38964462528165,5.01947941377285));
#86095=CARTESIAN_POINT('Ctrl Pts',(12.9461755055359,1.45826059395244,5.01423162321724));
#86096=CARTESIAN_POINT('Ctrl Pts',(12.9965212968207,1.52442754367236,5.00898383266163));
#86097=CARTESIAN_POINT('Ctrl Pts',(13.0467934877305,1.59049776410885,5.00374371383673));
#86098=CARTESIAN_POINT('Ctrl Pts',(13.1003733045611,1.65412573716825,4.99850359501183));
#86099=CARTESIAN_POINT('Ctrl Pts',(13.1569894777469,1.71496893991238,4.99326347618692));
#86100=CARTESIAN_POINT('Ctrl Pts',(13.2135877355353,1.77579288967475,4.98802501552444));
#86101=CARTESIAN_POINT('Ctrl Pts',(13.27322012749,1.83383348204527,4.98278655486195));
#86102=CARTESIAN_POINT('Ctrl Pts',(13.3355763533395,1.88878272292961,4.97754809419947));
#86103=CARTESIAN_POINT('Ctrl Pts',(13.3979316213402,1.94373111974321,4.97230971400454));
#86104=CARTESIAN_POINT('Ctrl Pts',(13.463010293335,1.99558795555208,4.96707133380962));
#86105=CARTESIAN_POINT('Ctrl Pts',(13.5304676465996,2.04408437015443,4.9618329536147));
#86106=CARTESIAN_POINT('Ctrl Pts',(13.59813121221,2.09272903485747,4.95657856006296));
#86107=CARTESIAN_POINT('Ctrl Pts',(13.6681876489952,2.137992425348,4.95132416651121));
#86108=CARTESIAN_POINT('Ctrl Pts',(13.7402598195989,2.17964697322364,4.94606977295947));
#86109=CARTESIAN_POINT('Ctrl Pts',(13.8122158132601,2.22123437593118,4.94082384924251));
#86110=CARTESIAN_POINT('Ctrl Pts',(13.8861806201403,2.25922437893871,4.93557792552555));
#86111=CARTESIAN_POINT('Ctrl Pts',(13.9617558816988,2.29343746389843,4.93033200180859));
#86112=CARTESIAN_POINT('Ctrl Pts',(14.037514173934,2.32773340724282,4.92507337333946));
#86113=CARTESIAN_POINT('Ctrl Pts',(14.114890291854,2.35823396355735,4.91981474487033));
#86114=CARTESIAN_POINT('Ctrl Pts',(14.1934662938004,2.38480809097165,4.91455611640119));
#86115=CARTESIAN_POINT('Ctrl Pts',(14.2720422957467,2.41138221838595,4.90929748793206));
#86116=CARTESIAN_POINT('Ctrl Pts',(14.3518177225178,2.43402984975802,4.90403885946293));
#86117=CARTESIAN_POINT('Ctrl Pts',(14.4323647341015,2.45267128961635,4.8987802309938));
#86118=CARTESIAN_POINT('Ctrl Pts',(14.5128834668174,2.47130618474009,4.89352344875157));
#86119=CARTESIAN_POINT('Ctrl Pts',(14.5944684357902,2.48600602173817,4.88826666650934));
#86120=CARTESIAN_POINT('Ctrl Pts',(14.6767007227819,2.49665452703218,4.88300988426711));
#86121=CARTESIAN_POINT('Ctrl Pts',(14.7588169739909,2.50728800650491,4.87776051972983));
#86122=CARTESIAN_POINT('Ctrl Pts',(14.8415782753605,2.51388145090071,4.87251115519255));
#86123=CARTESIAN_POINT('Ctrl Pts',(14.9245538919164,2.51636923657381,4.86726179065528));
#86124=CARTESIAN_POINT('Ctrl Pts',(15.0078732927155,2.51886732963057,4.86199067697181));
#86125=CARTESIAN_POINT('Ctrl Pts',(15.0914083300651,2.51722555892271,4.85671956328834));
#86126=CARTESIAN_POINT('Ctrl Pts',(15.1747159447591,2.51142998880059,4.85144844960487));
#86127=CARTESIAN_POINT('Ctrl Pts',(15.2575327894807,2.50566856071698,4.84620838835673));
#86128=CARTESIAN_POINT('Ctrl Pts',(15.3401244188441,2.49580217124105,4.84096832710858));
#86129=CARTESIAN_POINT('Ctrl Pts',(15.4220556324454,2.48186931427122,4.83572826586043));
#86130=CARTESIAN_POINT('Ctrl Pts',(15.5039601720778,2.46794099335766,4.83048991059496));
#86131=CARTESIAN_POINT('Ctrl Pts',(15.5852042687661,2.44994891162134,4.82525155532949));
#86132=CARTESIAN_POINT('Ctrl Pts',(15.6653601224456,2.42798314604101,4.82001320006402));
#86133=CARTESIAN_POINT('Ctrl Pts',(15.7455140166557,2.40601791743013,4.81477497285404));
#86134=CARTESIAN_POINT('Ctrl Pts',(15.8245792763412,2.38007932102533,4.80953674564406));
#86135=CARTESIAN_POINT('Ctrl Pts',(15.9021418820164,2.35030769787955,4.80429851843407));
#86136=CARTESIAN_POINT('Ctrl Pts',(15.9805493889443,2.3202117679177,4.79900323041891));
#86137=CARTESIAN_POINT('Ctrl Pts',(16.0574208498021,2.2861989507252,4.79370794240374));
#86138=CARTESIAN_POINT('Ctrl Pts',(16.1323496339631,2.24846404384497,4.78841265438857));
#86139=CARTESIAN_POINT('Ctrl Pts',(16.2065770889589,2.21108233355049,4.78316692996856));
#86140=CARTESIAN_POINT('Ctrl Pts',(16.2788977069171,2.17004820348001,4.77792120554854));
#86141=CARTESIAN_POINT('Ctrl Pts',(16.3489428619747,2.12559624696874,4.77267548112852));
#86142=CARTESIAN_POINT('Ctrl Pts',(16.4199807368444,2.08051429202457,4.76735541131578));
#86143=CARTESIAN_POINT('Ctrl Pts',(16.4886777444177,2.03191715767091,4.76203534150304));
#86144=CARTESIAN_POINT('Ctrl Pts',(16.5546831971137,1.9800925247605,4.7567152716903));
#86145=CARTESIAN_POINT('Ctrl Pts',(16.6206886498097,1.92826789185008,4.75139520187756));
#86146=CARTESIAN_POINT('Ctrl Pts',(16.6840022215195,1.87321612871151,4.74607513206482));
#86147=CARTESIAN_POINT('Ctrl Pts',(16.7443125632853,1.81526304748511,4.74075506225207));
#86148=CARTESIAN_POINT('Ctrl Pts',(16.8039030619099,1.75800167396285,4.73549849093153));
#86149=CARTESIAN_POINT('Ctrl Pts',(16.8607803053939,1.69769780895363,4.73024191961099));
#86150=CARTESIAN_POINT('Ctrl Pts',(16.9146180609925,1.63463877677032,4.72498534829044));
#86151=CARTESIAN_POINT('Ctrl Pts',(16.968379801339,1.571668779655,4.71973619889137));
#86152=CARTESIAN_POINT('Ctrl Pts',(17.0191102812959,1.50595169023062,4.71448704949229));
#86153=CARTESIAN_POINT('Ctrl Pts',(17.0665192341682,1.4378124025104,4.70923790009322));
#86154=CARTESIAN_POINT('Ctrl Pts',(17.1141270437554,1.36938730474612,4.70396673315227));
#86155=CARTESIAN_POINT('Ctrl Pts',(17.1583850577259,1.29851996784166,4.69869556621131));
#86156=CARTESIAN_POINT('Ctrl Pts',(17.1990395300914,1.22557390437916,4.69342439927036));
#86157=CARTESIAN_POINT('Ctrl Pts',(17.2394523698836,1.15306140071972,4.68818456186238));
#86158=CARTESIAN_POINT('Ctrl Pts',(17.2763041580762,1.0784952191346,4.68294472445441));
#86159=CARTESIAN_POINT('Ctrl Pts',(17.309389396096,1.00226087781539,4.67770488704643));
#86160=CARTESIAN_POINT('Ctrl Pts',(17.3424638447102,0.926051397227946,4.67246675839844));
#86161=CARTESIAN_POINT('Ctrl Pts',(17.3717739992685,0.848175260046755,4.66722862975046));
#86162=CARTESIAN_POINT('Ctrl Pts',(17.3971616089557,0.769039966808437,4.66199050110247));
#86163=CARTESIAN_POINT('Ctrl Pts',(17.4225485860033,0.689906645560786,4.65675250298462));
#86164=CARTESIAN_POINT('Ctrl Pts',(17.4440130726898,0.609514670065358,4.65151450486677));
#86165=CARTESIAN_POINT('Ctrl Pts',(17.4614464470319,0.528287458108025,4.64627650674893));
#86166=CARTESIAN_POINT('Ctrl Pts',(17.4790713721756,0.446167754699549,4.64098095564571));
#86167=CARTESIAN_POINT('Ctrl Pts',(17.4925759379711,0.363194814282982,4.6356854045425));
#86168=CARTESIAN_POINT('Ctrl Pts',(17.5019011574019,0.279815740427992,4.63038985343928));
#86169=CARTESIAN_POINT('Ctrl Pts',(17.5111382242823,0.197224860143897,4.62514436189107));
#86170=CARTESIAN_POINT('Ctrl Pts',(17.5162746601712,0.114235961838988,4.61989887034286));
#86171=CARTESIAN_POINT('Ctrl Pts',(17.5173055914026,0.0312859312310394,
4.61465337879465));
#86172=CARTESIAN_POINT('Ctrl Pts',(17.5183512804384,-0.0528515309784231,
4.60933279791393));
#86173=CARTESIAN_POINT('Ctrl Pts',(17.5151730139759,-0.136948512252474,
4.60401221703321));
#86174=CARTESIAN_POINT('Ctrl Pts',(17.507820208695,-0.220553963602515,4.59869163615249));
#86175=CARTESIAN_POINT('Ctrl Pts',(17.5004674034141,-0.304159414952556,
4.59337105527178));
#86176=CARTESIAN_POINT('Ctrl Pts',(17.4889401897988,-0.387272861644603,
4.58805047439106));
#86177=CARTESIAN_POINT('Ctrl Pts',(17.4733414428944,-0.469455383248395,
4.58272989351034));
#86178=CARTESIAN_POINT('Ctrl Pts',(17.4579299050636,-0.55065158756479,4.57747316782412));
#86179=CARTESIAN_POINT('Ctrl Pts',(17.4384875391269,-0.631236991974626,
4.57221644213791));
#86180=CARTESIAN_POINT('Ctrl Pts',(17.4150768313274,-0.710781364967923,
4.56695971645169));
#86181=CARTESIAN_POINT('Ctrl Pts',(17.3916991670801,-0.790213463327384,
4.56171041048518));
#86182=CARTESIAN_POINT('Ctrl Pts',(17.364364415959,-0.868607010265535,4.55646110451866));
#86183=CARTESIAN_POINT('Ctrl Pts',(17.333186179455,-0.945541380374444,4.55121179855215));
#86184=CARTESIAN_POINT('Ctrl Pts',(17.3018783306093,-1.0227955775479,4.54594067047784));
#86185=CARTESIAN_POINT('Ctrl Pts',(17.2666950549121,-1.09857797552401,4.54066954240352));
#86186=CARTESIAN_POINT('Ctrl Pts',(17.2278022311034,-1.17247749193354,4.53539841432921));
#86187=CARTESIAN_POINT('Ctrl Pts',(17.1891390980827,-1.24594057723586,4.53015841615091));
#86188=CARTESIAN_POINT('Ctrl Pts',(17.146810328221,-1.3175425467998,4.52491841797262));
#86189=CARTESIAN_POINT('Ctrl Pts',(17.1010266047129,-1.38690066561695,4.51967841979432));
#86190=CARTESIAN_POINT('Ctrl Pts',(17.0552578005805,-1.45623618295573,4.51444012915521));
#86191=CARTESIAN_POINT('Ctrl Pts',(17.0060365327093,-1.52332891726462,4.50920183851609));
#86192=CARTESIAN_POINT('Ctrl Pts',(16.9536177056951,-1.58782370242873,4.50396354787698));
#86193=CARTESIAN_POINT('Ctrl Pts',(16.9012001748603,-1.65231689280697,4.49872538676698));
#86194=CARTESIAN_POINT('Ctrl Pts',(16.8455855337545,-1.7142119046275,4.49348722565697));
#86195=CARTESIAN_POINT('Ctrl Pts',(16.7870691289199,-1.77318644774361,4.48824906454696));
#86196=CARTESIAN_POINT('Ctrl Pts',(16.7279137269679,-1.83280499083126,4.48295370289877));
#86197=CARTESIAN_POINT('Ctrl Pts',(16.6657931261,-1.8894385389231,4.47765834125057));
#86198=CARTESIAN_POINT('Ctrl Pts',(16.6010495560704,-1.94279349623342,4.47236297960237));
#86199=CARTESIAN_POINT('Ctrl Pts',(16.5369137185718,-1.99564762321825,4.46711732425761));
#86200=CARTESIAN_POINT('Ctrl Pts',(16.4702043590405,-2.04528422344915,4.46187166891285));
#86201=CARTESIAN_POINT('Ctrl Pts',(16.4012847755172,-2.09146054897142,4.45662601356809));
#86202=CARTESIAN_POINT('Ctrl Pts',(16.3313855991194,-2.13829320462705,4.45130579876818));
#86203=CARTESIAN_POINT('Ctrl Pts',(16.2592132971079,-2.18156619514584,4.44598558396826));
#86204=CARTESIAN_POINT('Ctrl Pts',(16.1851725660572,-2.22107456846127,4.44066536916835));
#86205=CARTESIAN_POINT('Ctrl Pts',(16.1111318350065,-2.26058294177669,4.43534515436843));
#86206=CARTESIAN_POINT('Ctrl Pts',(16.035223143569,-2.29632654792773,4.43002493956852));
#86207=CARTESIAN_POINT('Ctrl Pts',(15.9578702252833,-2.32815181668116,4.4247047247686));
#86208=CARTESIAN_POINT('Ctrl Pts',(15.8814408538521,-2.35959711105865,4.41944803010151));
#86209=CARTESIAN_POINT('Ctrl Pts',(15.803321217137,-2.38733251975011,4.41419133543442));
#86210=CARTESIAN_POINT('Ctrl Pts',(15.7239058116032,-2.4111753619194,4.40893464076733));
#86211=CARTESIAN_POINT('Ctrl Pts',(15.6446025012189,-2.43498454982552,4.40368536594493));
#86212=CARTESIAN_POINT('Ctrl Pts',(15.5640074929885,-2.45491195338061,4.39843609112252));
#86213=CARTESIAN_POINT('Ctrl Pts',(15.4825351598875,-2.47082295389054,4.39318681630012));
#86214=CARTESIAN_POINT('Ctrl Pts',(15.4007235287782,-2.48680021702702,4.3879156804554));
#86215=CARTESIAN_POINT('Ctrl Pts',(15.318027683937,-2.49872736769975,4.38264454461068));
#86216=CARTESIAN_POINT('Ctrl Pts',(15.2348825720286,-2.50651878655582,4.37737340876596));
#86217=CARTESIAN_POINT('Ctrl Pts',(15.1522291074359,-2.51426413378989,4.37213344179851));
#86218=CARTESIAN_POINT('Ctrl Pts',(15.0691321382078,-2.5179224807289,4.36689347483107));
#86219=CARTESIAN_POINT('Ctrl Pts',(14.9860273324777,-2.51746122404344,4.36165350786362));
#86220=CARTESIAN_POINT('Ctrl Pts',(14.9029496072365,-2.51700011766285,4.35641524838908));
#86221=CARTESIAN_POINT('Ctrl Pts',(14.8198645113117,-2.51242207640567,4.35117698891454));
#86222=CARTESIAN_POINT('Ctrl Pts',(14.7372087773475,-2.50374659726116,4.34593872944));
#86223=CARTESIAN_POINT('Ctrl Pts',(14.654555085836,-2.49507133249082,4.34070059940472));
#86224=CARTESIAN_POINT('Ctrl Pts',(14.5723311936678,-2.48229888035421,4.33546246936944));
#86225=CARTESIAN_POINT('Ctrl Pts',(14.4909683880573,-2.46550057149518,4.33022433933416));
#86226=CARTESIAN_POINT('Ctrl Pts',(14.4087160413711,-2.44851860641116,4.32492894072522));
#86227=CARTESIAN_POINT('Ctrl Pts',(14.3273441995726,-2.42742229671369,4.31963354211628));
#86228=CARTESIAN_POINT('Ctrl Pts',(14.2472857420408,-2.40233792291278,4.31433814350734));
#86229=CARTESIAN_POINT('Ctrl Pts',(14.1679797893908,-2.37748932824535,4.30909251869404));
#86230=CARTESIAN_POINT('Ctrl Pts',(14.0899630506313,-2.34872754544044,4.30384689388075));
#86231=CARTESIAN_POINT('Ctrl Pts',(14.0136373062393,-2.31622427376046,4.29860126906745));
#86232=CARTESIAN_POINT('Ctrl Pts',(13.9362252216669,-2.28325838477748,4.29328098356069));
#86233=CARTESIAN_POINT('Ctrl Pts',(13.8605530875749,-2.24644388040261,4.28796069805392));
#86234=CARTESIAN_POINT('Ctrl Pts',(13.7870136622207,-2.20600779562559,4.28264041254716));
#86235=CARTESIAN_POINT('Ctrl Pts',(13.7134742368666,-2.16557171084856,4.2773201270404));
#86236=CARTESIAN_POINT('Ctrl Pts',(13.6420679019044,-2.12151435634008,4.27199984153363));
#86237=CARTESIAN_POINT('Ctrl Pts',(13.573154773638,-2.07410678365602,4.26667955602687));
#86238=CARTESIAN_POINT('Ctrl Pts',(13.505345422078,-2.02745853471412,4.26144448515717));
#86239=CARTESIAN_POINT('Ctrl Pts',(13.4396966081709,-1.97739226415211,4.25620941428747));
#86240=CARTESIAN_POINT('Ctrl Pts',(13.3765751239122,-1.9241356297567,4.25097434341777));
#86241=CARTESIAN_POINT('Ctrl Pts',(13.3135429179877,-1.87095432096019,4.24574667697483));
#86242=CARTESIAN_POINT('Ctrl Pts',(13.2530312955316,-1.81459190711496,4.24051901053188));
#86243=CARTESIAN_POINT('Ctrl Pts',(13.1953778145324,-1.75531906436353,4.23529134408894));
#86244=CARTESIAN_POINT('Ctrl Pts',(13.1377897754579,-1.69611350165912,4.23006961152107));
#86245=CARTESIAN_POINT('Ctrl Pts',(13.0830537535038,-1.63400440705708,4.2248478789532));
#86246=CARTESIAN_POINT('Ctrl Pts',(13.0314728318686,-1.56930144915777,4.21962614638532));
#86247=CARTESIAN_POINT('Ctrl Pts',(12.9799237606473,-1.50463844432485,4.21440763815579));
#86248=CARTESIAN_POINT('Ctrl Pts',(12.9315262120739,-1.43738511830809,4.20918912992626));
#86249=CARTESIAN_POINT('Ctrl Pts',(12.8865443118865,-1.36788570589086,4.20397062169673));
#86250=CARTESIAN_POINT('Ctrl Pts',(12.8415763400671,-1.29840781353819,4.1987537293461));
#86251=CARTESIAN_POINT('Ctrl Pts',(12.8000221690277,-1.22668560636456,4.19353683699547));
#86252=CARTESIAN_POINT('Ctrl Pts',(12.7621029009024,-1.15309272127195,4.18831994464484));
#86253=CARTESIAN_POINT('Ctrl Pts',(12.7241837012758,-1.07949996912034,4.18310306171821));
#86254=CARTESIAN_POINT('Ctrl Pts',(12.6898996032389,-1.00403696023441,4.17788617879157));
#86255=CARTESIAN_POINT('Ctrl Pts',(12.6594253212799,-0.927101085823097,
4.17266929586493));
#86256=CARTESIAN_POINT('Ctrl Pts',(12.628921471219,-0.850090563294519,4.16744735118406));
#86257=CARTESIAN_POINT('Ctrl Pts',(12.602234991766,-0.771604754724609,4.16222540650318));
#86258=CARTESIAN_POINT('Ctrl Pts',(12.5794918391932,-0.692059602539742,
4.15700346182231));
#86259=CARTESIAN_POINT('Ctrl Pts',(12.5567376281915,-0.612475773025612,
4.15177897806937));
#86260=CARTESIAN_POINT('Ctrl Pts',(12.53793066827,-0.531832027762312,4.14655449431642));
#86261=CARTESIAN_POINT('Ctrl Pts',(12.5231459615928,-0.45055557085201,4.14133001056348));
#86262=CARTESIAN_POINT('Ctrl Pts',(12.5083357132044,-0.369138702648425,
4.13609650111542));
#86263=CARTESIAN_POINT('Ctrl Pts',(12.4975616595679,-0.287087401455886,
4.13086299166736));
#86264=CARTESIAN_POINT('Ctrl Pts',(12.4908469665597,-0.204834823155961,
4.1256294822193));
#86265=CARTESIAN_POINT('Ctrl Pts',(12.4852674669627,-0.136487956529057,
4.12128075565497));
#86266=CARTESIAN_POINT('Ctrl Pts',(12.4824898390633,-0.0680023103452117,
4.11693202909065));
#86267=CARTESIAN_POINT('Ctrl Pts',(12.4825000279491,0.000375131315901805,
4.11258330252632));
#86268=CARTESIAN_POINT('Ctrl Pts',(12.4825000279491,0.000375131855856907,
4.11258330249198));
#86269=CARTESIAN_POINT('Ctrl Pts',(12.482503096382,0.0209673034085757,4.1112736640897));
#86270=CARTESIAN_POINT('Ctrl Pts',(12.4827588140224,0.041557321852414,4.10996402568741));
#86271=CARTESIAN_POINT('Ctrl Pts',(12.4832670510668,0.062141079441871,4.10865438728512));
#86272=CARTESIAN_POINT('Ctrl Pts',(12.4853066576079,0.144745775577443,4.10339867623244));
#86273=CARTESIAN_POINT('Ctrl Pts',(12.4914212102481,0.227401430820226,4.09814296517976));
#86274=CARTESIAN_POINT('Ctrl Pts',(12.501618824813,0.309673624112754,4.09288725412709));
#86275=CARTESIAN_POINT('Ctrl Pts',(12.5118038118859,0.391843941476571,4.08763805111102));
#86276=CARTESIAN_POINT('Ctrl Pts',(12.5260617710905,0.473631285663338,4.08238884809495));
#86277=CARTESIAN_POINT('Ctrl Pts',(12.5443488333121,0.554602197565569,4.07713964507888));
#86278=CARTESIAN_POINT('Ctrl Pts',(12.5626153556443,0.635482163553971,4.07189633792781));
#86279=CARTESIAN_POINT('Ctrl Pts',(12.5849018858058,0.715547072294699,4.06665303077675));
#86280=CARTESIAN_POINT('Ctrl Pts',(12.6111130818692,0.794371161601245,4.06140972362568));
#86281=CARTESIAN_POINT('Ctrl Pts',(12.6198333339686,0.820595296073974,4.05966531791138));
#86282=CARTESIAN_POINT('Ctrl Pts',(12.628987563394,0.846682173052394,4.05792091219707));
#86283=CARTESIAN_POINT('Ctrl Pts',(12.6385710119932,0.872616401748848,4.05617650648277));
#86284=CARTESIAN_POINT('',(12.4825009521567,-0.00218954522945693,4.38741669750802));
#86285=CARTESIAN_POINT('Ctrl Pts',(12.6421214752944,0.871321765791516,4.3311309048973));
#86286=CARTESIAN_POINT('Ctrl Pts',(12.5397813919921,0.591632227618603,4.34989269415061));
#86287=CARTESIAN_POINT('Ctrl Pts',(12.4844694673097,0.294291735004427,4.36865448340391));
#86288=CARTESIAN_POINT('Ctrl Pts',(12.4817777656426,-0.00218346073577532,
4.38741627265722));
#86289=CARTESIAN_POINT('Ctrl Pts',(12.4825009521567,-0.00218954522945693,
4.38741669750802));
#86290=CARTESIAN_POINT('Ctrl Pts',(12.4826026785113,-0.119152646681798,
4.39482064432068));
#86291=CARTESIAN_POINT('Ctrl Pts',(12.4908590803219,-0.235770821827561,
4.40222459113333));
#86292=CARTESIAN_POINT('Ctrl Pts',(12.5071061350226,-0.351121671159536,
4.40962853794598));
#86293=CARTESIAN_POINT('Ctrl Pts',(12.5145083371291,-0.403675830399398,
4.4130017961582));
#86294=CARTESIAN_POINT('Ctrl Pts',(12.5235685720467,-0.455967358934549,
4.41637505437042));
#86295=CARTESIAN_POINT('Ctrl Pts',(12.5342682792954,-0.507910751521386,
4.41974831258264));
#86296=CARTESIAN_POINT('Ctrl Pts',(12.5509424201429,-0.588857961006813,
4.42500510898262));
#86297=CARTESIAN_POINT('Ctrl Pts',(12.5716374708985,-0.669131665759261,
4.43026190538259));
#86298=CARTESIAN_POINT('Ctrl Pts',(12.5962842531434,-0.748302651547934,
4.43551870178256));
#86299=CARTESIAN_POINT('Ctrl Pts',(12.6208962422798,-0.827361874077981,
4.44076807732388));
#86300=CARTESIAN_POINT('Ctrl Pts',(12.6494487461163,-0.905321033100365,
4.44601745286519));
#86301=CARTESIAN_POINT('Ctrl Pts',(12.6818216267449,-0.981761315072212,
4.4512668284065));
#86302=CARTESIAN_POINT('Ctrl Pts',(12.7143285470236,-1.05851809741272,4.45653793894475));
#86303=CARTESIAN_POINT('Ctrl Pts',(12.7506874579344,-1.13374293511867,4.46180904948299));
#86304=CARTESIAN_POINT('Ctrl Pts',(12.7907261080111,-1.20702738998586,4.46708016002124));
#86305=CARTESIAN_POINT('Ctrl Pts',(12.8305289366073,-1.27988021070443,4.4723202245305));
#86306=CARTESIAN_POINT('Ctrl Pts',(12.8739680542269,-1.3508150337928,4.47756028903977));
#86307=CARTESIAN_POINT('Ctrl Pts',(12.9208268435731,-1.41945244217396,4.48280035354904));
#86308=CARTESIAN_POINT('Ctrl Pts',(12.9676703512691,-1.48806746643316,4.48803870916157));
#86309=CARTESIAN_POINT('Ctrl Pts',(13.017931055935,-1.55438618354357,4.4932770647741));
#86310=CARTESIAN_POINT('Ctrl Pts',(13.071348553121,-1.61805742989904,4.49851542038663));
#86311=CARTESIAN_POINT('Ctrl Pts',(13.1247647147894,-1.68172708437781,4.50375364503241));
#86312=CARTESIAN_POINT('Ctrl Pts',(13.1813372148716,-1.74274904716061,4.50899186967819));
#86313=CARTESIAN_POINT('Ctrl Pts',(13.2407657232065,-1.80080565563164,4.51423009432397));
#86314=CARTESIAN_POINT('Ctrl Pts',(13.3008415593174,-1.85949464839591,4.51952537657401));
#86315=CARTESIAN_POINT('Ctrl Pts',(13.3638356695576,-1.91515294399448,4.52482065882404));
#86316=CARTESIAN_POINT('Ctrl Pts',(13.4294013205346,-1.967492322237,4.53011594107407));
#86317=CARTESIAN_POINT('Ctrl Pts',(13.4943532315647,-2.01934176761457,4.53536165581126));
#86318=CARTESIAN_POINT('Ctrl Pts',(13.5618283271267,-2.067933948377,4.54060737054844));
#86319=CARTESIAN_POINT('Ctrl Pts',(13.6314595714653,-2.11303178997998,4.54585308528563));
#86320=CARTESIAN_POINT('Ctrl Pts',(13.7020777492643,-2.15876883556806,4.55117315129209));
#86321=CARTESIAN_POINT('Ctrl Pts',(13.7749132499518,-2.20091146499363,4.55649321729855));
#86322=CARTESIAN_POINT('Ctrl Pts',(13.8495582792929,-2.2392610605413,4.561813283305));
#86323=CARTESIAN_POINT('Ctrl Pts',(13.924203308634,-2.27761065608897,4.56713334931146));
#86324=CARTESIAN_POINT('Ctrl Pts',(14.0006573958101,-2.31216707511688,4.57245341531792));
#86325=CARTESIAN_POINT('Ctrl Pts',(14.0784945123771,-2.34278336307069,4.57777348132438));
#86326=CARTESIAN_POINT('Ctrl Pts',(14.1554076810325,-2.37303622729349,4.58303039668892));
#86327=CARTESIAN_POINT('Ctrl Pts',(14.2339531941902,-2.39955296223892,4.58828731205347));
#86328=CARTESIAN_POINT('Ctrl Pts',(14.3137337174689,-2.42215706333446,4.59354422741801));
#86329=CARTESIAN_POINT('Ctrl Pts',(14.393401662519,-2.44472926780212,4.59879372475374));
#86330=CARTESIAN_POINT('Ctrl Pts',(14.4743007160961,-2.4633996805871,4.60404322208948));
#86331=CARTESIAN_POINT('Ctrl Pts',(14.5560144214902,-2.4780401643386,4.60929271942521));
#86332=CARTESIAN_POINT('Ctrl Pts',(14.6380640896605,-2.49274084187942,4.61456379986858));
#86333=CARTESIAN_POINT('Ctrl Pts',(14.7209346856385,-2.50337820526777,4.61983488031195));
#86334=CARTESIAN_POINT('Ctrl Pts',(14.8041900168466,-2.50987344312367,4.62510596075533));
#86335=CARTESIAN_POINT('Ctrl Pts',(14.8869574766042,-2.51633061925946,4.63034615297058));
#86336=CARTESIAN_POINT('Ctrl Pts',(14.9701047104277,-2.51869404562131,4.63558634518584));
#86337=CARTESIAN_POINT('Ctrl Pts',(15.0531955631248,-2.51693791780088,4.6408265374011));
#86338=CARTESIAN_POINT('Ctrl Pts',(15.1362593492159,-2.51518236203403,4.64606502263883));
#86339=CARTESIAN_POINT('Ctrl Pts',(15.2192663300518,-2.50930992706722,4.65130350787656));
#86340=CARTESIAN_POINT('Ctrl Pts',(15.3017800988686,-2.49934691908243,4.65654199311428));
#86341=CARTESIAN_POINT('Ctrl Pts',(15.3842918320055,-2.48938415689293,4.66178034911444));
#86342=CARTESIAN_POINT('Ctrl Pts',(15.4663099197064,-2.47533107868237,4.66701870511459));
#86343=CARTESIAN_POINT('Ctrl Pts',(15.5474042080151,-2.4572657330959,4.67225706111475));
#86344=CARTESIAN_POINT('Ctrl Pts',(15.629377444368,-2.43900458456816,4.67755219352736));
#86345=CARTESIAN_POINT('Ctrl Pts',(15.7104062614077,-2.41664375387076,4.68284732593997));
#86346=CARTESIAN_POINT('Ctrl Pts',(15.7900598880583,-2.39031621826095,4.68814245835259));
#86347=CARTESIAN_POINT('Ctrl Pts',(15.8689721532152,-2.36423372135111,4.69338830729326));
#86348=CARTESIAN_POINT('Ctrl Pts',(15.9465343076132,-2.33425827725141,4.69863415623393));
#86349=CARTESIAN_POINT('Ctrl Pts',(16.0223472614685,-2.30056782707396,4.7038800051746));
#86350=CARTESIAN_POINT('Ctrl Pts',(16.0992285816531,-2.26640260654717,4.70919977932318));
#86351=CARTESIAN_POINT('Ctrl Pts',(16.1743105791559,-2.22841708208727,4.71451955347177));
#86352=CARTESIAN_POINT('Ctrl Pts',(16.2472042039599,-2.18684428426554,4.71983932762036));
#86353=CARTESIAN_POINT('Ctrl Pts',(16.3200978287638,-2.14527148644381,4.72515910176894));
#86354=CARTESIAN_POINT('Ctrl Pts',(16.390802704373,-2.10011173155922,4.73047887591753));
#86355=CARTESIAN_POINT('Ctrl Pts',(16.458963082923,-2.05164153122999,4.73579865006611));
#86356=CARTESIAN_POINT('Ctrl Pts',(16.5263035212876,-2.00375440666842,4.74105442960823));
#86357=CARTESIAN_POINT('Ctrl Pts',(16.5914075487985,-1.95246031526691,4.74631020915035));
#86358=CARTESIAN_POINT('Ctrl Pts',(16.6539103478986,-1.89799547183706,4.75156598869247));
#86359=CARTESIAN_POINT('Ctrl Pts',(16.7163248871285,-1.8436075379229,4.75681434657625));
#86360=CARTESIAN_POINT('Ctrl Pts',(16.7761451491439,-1.78605804606437,4.76206270446003));
#86361=CARTESIAN_POINT('Ctrl Pts',(16.8330363715109,-1.72562565775953,4.76731106234382));
#86362=CARTESIAN_POINT('Ctrl Pts',(16.8901769851375,-1.66492835495987,4.77258242719648));
#86363=CARTESIAN_POINT('Ctrl Pts',(16.9443624322927,-1.60132309141237,4.77785379204915));
#86364=CARTESIAN_POINT('Ctrl Pts',(16.9952882348807,-1.53513227760557,4.78312515690182));
#86365=CARTESIAN_POINT('Ctrl Pts',(17.0459018711517,-1.46934720198099,4.7883642092043));
#86366=CARTESIAN_POINT('Ctrl Pts',(17.0932954269318,-1.40100855361851,4.79360326150678));
#86367=CARTESIAN_POINT('Ctrl Pts',(17.1372090912285,-1.33046741800404,4.79884231380926));
#86368=CARTESIAN_POINT('Ctrl Pts',(17.181108467436,-1.25994923419866,4.80407966149319));
#86369=CARTESIAN_POINT('Ctrl Pts',(17.2215299573087,-1.18723037771864,4.80931700917712));
#86370=CARTESIAN_POINT('Ctrl Pts',(17.2582572587677,-1.1126906143322,4.81455435686105));
#86371=CARTESIAN_POINT('Ctrl Pts',(17.2949836812295,-1.03815263491123,4.81979157919916));
#86372=CARTESIAN_POINT('Ctrl Pts',(17.3280158881588,-0.961794249499344,
4.82502880153728));
#86373=CARTESIAN_POINT('Ctrl Pts',(17.3571843329208,-0.88401825243195,4.83026602387539));
#86374=CARTESIAN_POINT('Ctrl Pts',(17.3866828264446,-0.805362199134683,
4.83556250678643));
#86375=CARTESIAN_POINT('Ctrl Pts',(17.4122293803436,-0.725256695124534,
4.84085898969747));
#86376=CARTESIAN_POINT('Ctrl Pts',(17.4336999597987,-0.644135665582961,
4.8461554726085));
#86377=CARTESIAN_POINT('Ctrl Pts',(17.4549607719518,-0.563807187520034,
4.85140020894549));
#86378=CARTESIAN_POINT('Ctrl Pts',(17.4722248706125,-0.482483410093979,
4.85664494528247));
#86379=CARTESIAN_POINT('Ctrl Pts',(17.4854233756316,-0.400595673796245,
4.86188968161945));
#86380=CARTESIAN_POINT('Ctrl Pts',(17.4988172128962,-0.317496033923638,
4.86721203781751));
#86381=CARTESIAN_POINT('Ctrl Pts',(17.508024083252,-0.233816096765077,4.87253439401558));
#86382=CARTESIAN_POINT('Ctrl Pts',(17.513026721991,-0.150009814875842,4.87785675021365));
#86383=CARTESIAN_POINT('Ctrl Pts',(17.51802936073,-0.0662035329866071,4.88317910641171));
#86384=CARTESIAN_POINT('Ctrl Pts',(17.5188278275939,0.0177286035890774,
4.88850146260978));
#86385=CARTESIAN_POINT('Ctrl Pts',(17.5154596198684,0.101336818636153,4.89382381880785));
#86386=CARTESIAN_POINT('Ctrl Pts',(17.5121322980462,0.183930132684131,4.89908156814138));
#86387=CARTESIAN_POINT('Ctrl Pts',(17.5047267383458,0.266510655466996,4.90433931747492));
#86388=CARTESIAN_POINT('Ctrl Pts',(17.4932416552582,0.348643512036484,4.90959706680846));
#86389=CARTESIAN_POINT('Ctrl Pts',(17.4817727907503,0.430660385267855,4.91484739144811));
#86390=CARTESIAN_POINT('Ctrl Pts',(17.4662359093044,0.51223039527895,4.92009771608775));
#86391=CARTESIAN_POINT('Ctrl Pts',(17.4466816967508,0.592920673264535,4.9253480407274));
#86392=CARTESIAN_POINT('Ctrl Pts',(17.4270509550653,0.67392674800837,4.93061891351165));
#86393=CARTESIAN_POINT('Ctrl Pts',(17.4033713892679,0.754045720168594,4.93588978629591));
#86394=CARTESIAN_POINT('Ctrl Pts',(17.3757467156412,0.832846800510245,4.94116065908017));
#86395=CARTESIAN_POINT('Ctrl Pts',(17.3482786185898,0.911201236541949,4.94640165657176));
#86396=CARTESIAN_POINT('Ctrl Pts',(17.3169101696193,0.988252241036131,4.95164265406335));
#86397=CARTESIAN_POINT('Ctrl Pts',(17.2817936326646,1.06359017856083,4.95688365155495));
#86398=CARTESIAN_POINT('Ctrl Pts',(17.2466886001331,1.13890343485042,4.96212293205912));
#86399=CARTESIAN_POINT('Ctrl Pts',(17.2078381129796,1.21250432138666,4.96736221256328));
#86400=CARTESIAN_POINT('Ctrl Pts',(17.1654422248974,1.28400397999053,4.97260149306745));
#86401=CARTESIAN_POINT('Ctrl Pts',(17.1230474718603,1.3555017243676,4.97784063330282));
#86402=CARTESIAN_POINT('Ctrl Pts',(17.0771077426224,1.42489795675396,4.98307977353819));
#86403=CARTESIAN_POINT('Ctrl Pts',(17.0278679227338,1.49183039851959,4.98831891377356));
#86404=CARTESIAN_POINT('Ctrl Pts',(16.9781108816657,1.55946590696097,4.99361308658823));
#86405=CARTESIAN_POINT('Ctrl Pts',(16.9249842830702,1.62458516320357,4.9989072594029));
#86406=CARTESIAN_POINT('Ctrl Pts',(16.8687832353091,1.68684779082991,5.00420143221757));
#86407=CARTESIAN_POINT('Ctrl Pts',(16.8130872209956,1.7485509144836,5.0094480305749));
#86408=CARTESIAN_POINT('Ctrl Pts',(16.754372163587,1.80744825725024,5.01469462893223));
#86409=CARTESIAN_POINT('Ctrl Pts',(16.6929618352904,1.86324621943808,5.01994122728956));
#86410=CARTESIAN_POINT('Ctrl Pts',(16.6307162334952,1.91980311844294,5.0252591873329));
#86411=CARTESIAN_POINT('Ctrl Pts',(16.5657018681939,1.97317537879475,5.03057714737624));
#86412=CARTESIAN_POINT('Ctrl Pts',(16.4982883485331,2.02310115284677,5.03589510741957));
#86413=CARTESIAN_POINT('Ctrl Pts',(16.4308748288723,2.07302692689879,5.04121306746291));
#86414=CARTESIAN_POINT('Ctrl Pts',(16.3610625947837,2.11950599799578,5.04653102750625));
#86415=CARTESIAN_POINT('Ctrl Pts',(16.2892475889811,2.16232442161354,5.05184898754959));
#86416=CARTESIAN_POINT('Ctrl Pts',(16.2182439398869,2.20465908818283,5.05710686596364));
#86417=CARTESIAN_POINT('Ctrl Pts',(16.1450232189915,2.24357007403483,5.06236474437769));
#86418=CARTESIAN_POINT('Ctrl Pts',(16.0699490872646,2.27881881698867,5.06762262279174));
#86419=CARTESIAN_POINT('Ctrl Pts',(15.9949806778278,2.31401792130211,5.07287309685846));
#86420=CARTESIAN_POINT('Ctrl Pts',(15.9181644558188,2.34556483276518,5.07812357092518));
#86421=CARTESIAN_POINT('Ctrl Pts',(15.8398907776888,2.37326562600002,5.0833740449919));
#86422=CARTESIAN_POINT('Ctrl Pts',(15.7613135159864,2.40107385644709,5.08864488296271));
#86423=CARTESIAN_POINT('Ctrl Pts',(15.6812678730099,2.42500583125158,5.09391572093352));
#86424=CARTESIAN_POINT('Ctrl Pts',(15.6001713694366,2.44491320445299,5.09918655890433));
#86425=CARTESIAN_POINT('Ctrl Pts',(15.5195309540679,2.46470861822704,5.10442775358695));
#86426=CARTESIAN_POINT('Ctrl Pts',(15.4378519187879,2.48052446793078,5.10966894826957));
#86427=CARTESIAN_POINT('Ctrl Pts',(15.355560620274,2.492264611816,5.11491014295219));
#86428=CARTESIAN_POINT('Ctrl Pts',(15.2732960073148,2.50400094858847,5.12014963801177));
#86429=CARTESIAN_POINT('Ctrl Pts',(15.1904199813549,2.51166413955409,5.12538913307134));
#86430=CARTESIAN_POINT('Ctrl Pts',(15.1073675872123,2.51520942492195,5.13062862813092));
#86431=CARTESIAN_POINT('Ctrl Pts',(15.024317147798,2.51875462684768,5.1358679998733));
#86432=CARTESIAN_POINT('Ctrl Pts',(14.9410908089415,2.51818209731604,5.14110737161567));
#86433=CARTESIAN_POINT('Ctrl Pts',(14.8581258282308,2.51349914847505,5.14634674335805));
#86434=CARTESIAN_POINT('Ctrl Pts',(14.7742965886488,2.50876741664099,5.15164069443582));
#86435=CARTESIAN_POINT('Ctrl Pts',(14.690734664194,2.49983913751875,5.1569346455136));
#86436=CARTESIAN_POINT('Ctrl Pts',(14.6078862702578,2.48677563783862,5.16222859659137));
#86437=CARTESIAN_POINT('Ctrl Pts',(14.5257746996796,2.47382832015363,5.1674754652017));
#86438=CARTESIAN_POINT('Ctrl Pts',(14.444364461817,2.45681919966076,5.17272233381203));
#86439=CARTESIAN_POINT('Ctrl Pts',(14.3640783581804,2.4358591739806,5.17796920242236));
#86440=CARTESIAN_POINT('Ctrl Pts',(14.2827115905875,2.41461702296057,5.18328669473385));
#86441=CARTESIAN_POINT('Ctrl Pts',(14.2024999117225,2.38931696199221,5.18860418704535));
#86442=CARTESIAN_POINT('Ctrl Pts',(14.1238643774788,2.3601255519462,5.19392167935684));
#86443=CARTESIAN_POINT('Ctrl Pts',(14.0452288432351,2.3309341419002,5.19923917166833));
#86444=CARTESIAN_POINT('Ctrl Pts',(13.9681698749681,2.29785163286193,5.20455666397982));
#86445=CARTESIAN_POINT('Ctrl Pts',(13.8930827918329,2.26109277657146,5.20987415629132));
#86446=CARTESIAN_POINT('Ctrl Pts',(13.818967537694,2.22480967883919,5.21512282593718));
#86447=CARTESIAN_POINT('Ctrl Pts',(13.7465001655502,2.18481109152274,5.22037149558304));
#86448=CARTESIAN_POINT('Ctrl Pts',(13.6760781339948,2.14126998361096,5.22562016522891));
#86449=CARTESIAN_POINT('Ctrl Pts',(13.6057473964787,2.0977853217222,5.23086203058012));
#86450=CARTESIAN_POINT('Ctrl Pts',(13.5374571258062,2.05076749601277,5.23610389593133));
#86451=CARTESIAN_POINT('Ctrl Pts',(13.4715822306485,2.00043629549423,5.24134576128255));
#86452=CARTESIAN_POINT('Ctrl Pts',(13.4057727555764,1.95015507868241,5.246582420959));
#86453=CARTESIAN_POINT('Ctrl Pts',(13.3423742584481,1.89656729989107,5.25181908063545));
#86454=CARTESIAN_POINT('Ctrl Pts',(13.2817333769281,1.83993642880321,5.2570557403119));
#86455=CARTESIAN_POINT('Ctrl Pts',(13.2211343290392,1.78334462500638,5.26228878743386));
#86456=CARTESIAN_POINT('Ctrl Pts',(13.163289454592,1.72371421395633,5.26752183455582));
#86457=CARTESIAN_POINT('Ctrl Pts',(13.1085118484535,1.66134849521679,5.27275488167778));
#86458=CARTESIAN_POINT('Ctrl Pts',(13.0537414455995,1.59899097760267,5.27798724065124));
#86459=CARTESIAN_POINT('Ctrl Pts',(13.0020378243509,1.53389920553269,5.2832195996247));
#86460=CARTESIAN_POINT('Ctrl Pts',(12.9536760086717,1.46641207459365,5.28845195859816));
#86461=CARTESIAN_POINT('Ctrl Pts',(12.9053194971707,1.39893234543989,5.29368374370224));
#86462=CARTESIAN_POINT('Ctrl Pts',(12.8603043270388,1.32905815925125,5.29891552880632));
#86463=CARTESIAN_POINT('Ctrl Pts',(12.8188630687219,1.25715867614815,5.30414731391041));
#86464=CARTESIAN_POINT('Ctrl Pts',(12.7773933060078,1.18520973867258,5.30938269757513));
#86465=CARTESIAN_POINT('Ctrl Pts',(12.7395025915379,1.11123312576133,5.31461808123984));
#86466=CARTESIAN_POINT('Ctrl Pts',(12.7053778834278,1.03562328678803,5.31985346490456));
#86467=CARTESIAN_POINT('Ctrl Pts',(12.6812025435737,0.982058182360065,5.32356242496225));
#86468=CARTESIAN_POINT('Ctrl Pts',(12.6589163547355,0.927673907001395,5.32727138501995));
#86469=CARTESIAN_POINT('Ctrl Pts',(12.6385710119932,0.872616401748844,5.33098034507765));
#86470=CARTESIAN_POINT('Origin',(-15.,0.,3.));
#86471=CARTESIAN_POINT('',(-17.5174999720511,0.000375130022130284,4.11258330252632));
#86472=CARTESIAN_POINT('Ctrl Pts',(-17.3614291890287,0.872615857753804,
5.05624492860065));
#86473=CARTESIAN_POINT('Ctrl Pts',(-17.3327792589059,0.950146859115319,
5.05098830411758));
#86474=CARTESIAN_POINT('Ctrl Pts',(-17.3002548807785,1.02640647843984,5.04573167963452));
#86475=CARTESIAN_POINT('Ctrl Pts',(-17.2639892861135,1.10098081834484,5.04047505515146));
#86476=CARTESIAN_POINT('Ctrl Pts',(-17.2277744395237,1.17545080302707,5.0352257864991));
#86477=CARTESIAN_POINT('Ctrl Pts',(-17.1878289755028,1.24823978142076,5.02997651784674));
#86478=CARTESIAN_POINT('Ctrl Pts',(-17.1443349279334,1.3189518440204,5.02472724919438));
#86479=CARTESIAN_POINT('Ctrl Pts',(-17.1008531119921,1.38964402059651,5.01947945676935));
#86480=CARTESIAN_POINT('Ctrl Pts',(-17.0538248976113,1.45826002793457,5.01423166434433));
#86481=CARTESIAN_POINT('Ctrl Pts',(-17.0034791048836,1.52442701573245,5.00898387191931));
#86482=CARTESIAN_POINT('Ctrl Pts',(-16.9532069480364,1.59049722753091,5.00374375492842));
#86483=CARTESIAN_POINT('Ctrl Pts',(-16.8996271665276,1.65412519481614,4.99850363793753));
#86484=CARTESIAN_POINT('Ctrl Pts',(-16.8430110295824,1.71496839470516,4.99326352094664));
#86485=CARTESIAN_POINT('Ctrl Pts',(-16.7864128081436,1.7757923414837,4.98802506212875));
#86486=CARTESIAN_POINT('Ctrl Pts',(-16.7267804534695,1.83383293379899,4.98278660331086));
#86487=CARTESIAN_POINT('Ctrl Pts',(-16.6644242655098,1.88878217759019,4.97754814449297));
#86488=CARTESIAN_POINT('Ctrl Pts',(-16.6020690354947,1.94373057722563,4.97230976615072));
#86489=CARTESIAN_POINT('Ctrl Pts',(-16.5369904021032,1.99558741882749,4.96707138780846));
#86490=CARTESIAN_POINT('Ctrl Pts',(-16.4695330877559,2.04408384221165,4.9618330094662));
#86491=CARTESIAN_POINT('Ctrl Pts',(-16.4018694773153,2.09272857601661,4.95657861126017));
#86492=CARTESIAN_POINT('Ctrl Pts',(-16.331812990079,2.13799203022439,4.95132421305414));
#86493=CARTESIAN_POINT('Ctrl Pts',(-16.2597407645321,2.17964663562147,4.94606981484811));
#86494=CARTESIAN_POINT('Ctrl Pts',(-16.1877848051222,2.22123404425838,4.94082389298059));
#86495=CARTESIAN_POINT('Ctrl Pts',(-16.1138200329979,2.25922405593769,4.93557797111307));
#86496=CARTESIAN_POINT('Ctrl Pts',(-16.0382448064517,2.29343715237112,4.93033204924555));
#86497=CARTESIAN_POINT('Ctrl Pts',(-15.9624864087051,2.32773317087077,4.92507341287026));
#86498=CARTESIAN_POINT('Ctrl Pts',(-15.8851101795222,2.35823379105163,4.91981477649497));
#86499=CARTESIAN_POINT('Ctrl Pts',(-15.8065340626515,2.38480797042086,4.91455614011968));
#86500=CARTESIAN_POINT('Ctrl Pts',(-15.7279579457808,2.41138214979008,4.90929750374439));
#86501=CARTESIAN_POINT('Ctrl Pts',(-15.6481824004284,2.43402982120515,4.9040388673691));
#86502=CARTESIAN_POINT('Ctrl Pts',(-15.5676352687526,2.45267128895581,4.89878023099381));
#86503=CARTESIAN_POINT('Ctrl Pts',(-15.487116541093,2.47130618300806,4.89352344901594));
#86504=CARTESIAN_POINT('Ctrl Pts',(-15.4055315770578,2.48600601948482,4.88826666703806));
#86505=CARTESIAN_POINT('Ctrl Pts',(-15.3232992948241,2.49665452475232,4.88300988506018));
#86506=CARTESIAN_POINT('Ctrl Pts',(-15.2411830485188,2.50728800417886,4.87776052079662));
#86507=CARTESIAN_POINT('Ctrl Pts',(-15.158421751876,2.51388144903671,4.87251115653306));
#86508=CARTESIAN_POINT('Ctrl Pts',(-15.0754461398187,2.51636923562232,4.8672617922695));
#86509=CARTESIAN_POINT('Ctrl Pts',(-14.9921267381292,2.51886732975751,4.86199067851878));
#86510=CARTESIAN_POINT('Ctrl Pts',(-14.9085916996311,2.51722556004416,4.85671956476805));
#86511=CARTESIAN_POINT('Ctrl Pts',(-14.8252840835758,2.5114299907718,4.85144845101732));
#86512=CARTESIAN_POINT('Ctrl Pts',(-14.7424672432149,2.50566856393045,4.84620839006385));
#86513=CARTESIAN_POINT('Ctrl Pts',(-14.6598756179712,2.49580217612066,4.84096832911037));
#86514=CARTESIAN_POINT('Ctrl Pts',(-14.577944408213,2.48186932118541,4.8357282681569));
#86515=CARTESIAN_POINT('Ctrl Pts',(-14.4960398725376,2.46794100232533,4.83048991319336));
#86516=CARTESIAN_POINT('Ctrl Pts',(-14.4147957795282,2.44994892302203,4.82525155822983));
#86517=CARTESIAN_POINT('Ctrl Pts',(-14.3346399292213,2.4279831601997,4.8200132032663));
#86518=CARTESIAN_POINT('Ctrl Pts',(-14.2544860384891,2.40601793437565,4.81477497636513));
#86519=CARTESIAN_POINT('Ctrl Pts',(-14.1754207819724,2.38007934109304,4.80953674946397));
#86520=CARTESIAN_POINT('Ctrl Pts',(-14.0978581791351,2.35030772135193,4.80429852256281));
#86521=CARTESIAN_POINT('Ctrl Pts',(-14.0194506653589,2.32021179110205,4.79900323420358));
#86522=CARTESIAN_POINT('Ctrl Pts',(-13.9425791976959,2.28619897293829,4.79370794584435));
#86523=CARTESIAN_POINT('Ctrl Pts',(-13.8676504069068,2.24846406442746,4.78841265748512));
#86524=CARTESIAN_POINT('Ctrl Pts',(-13.793422954735,2.21108235724662,4.78316693338788));
#86525=CARTESIAN_POINT('Ctrl Pts',(-13.7211023392919,2.17004823056789,4.77792120929063));
#86526=CARTESIAN_POINT('Ctrl Pts',(-13.6510571864243,2.12559627768362,4.77267548519338));
#86527=CARTESIAN_POINT('Ctrl Pts',(-13.5800193003584,2.08051431790306,4.76735541470316));
#86528=CARTESIAN_POINT('Ctrl Pts',(-13.51132228214,2.03191717762586,4.76203534421294));
#86529=CARTESIAN_POINT('Ctrl Pts',(-13.4453168195322,1.9800925378301,4.75671527372273));
#86530=CARTESIAN_POINT('Ctrl Pts',(-13.3793113569244,1.92826789803434,4.75139520323251));
#86531=CARTESIAN_POINT('Ctrl Pts',(-13.3159977760365,1.87321612704899,4.74607513274229));
#86532=CARTESIAN_POINT('Ctrl Pts',(-13.2556874259808,1.81526303717081,4.74075506225207));
#86533=CARTESIAN_POINT('Ctrl Pts',(-13.1960969185787,1.75800165453635,4.73549849021039));
#86534=CARTESIAN_POINT('Ctrl Pts',(-13.1392196674876,1.6976977798114,4.73024191816871));
#86535=CARTESIAN_POINT('Ctrl Pts',(-13.085381905456,1.63463873747217,4.72498534612703));
#86536=CARTESIAN_POINT('Ctrl Pts',(-13.0316201585583,1.57166873006624,4.71973619599542));
#86537=CARTESIAN_POINT('Ctrl Pts',(-12.980889673235,1.50595162989935,4.71448704586381));
#86538=CARTESIAN_POINT('Ctrl Pts',(-12.9334807161726,1.43781233113695,4.70923789573219));
#86539=CARTESIAN_POINT('Ctrl Pts',(-12.8858729106628,1.36938723419194,4.70396672897295));
#86540=CARTESIAN_POINT('Ctrl Pts',(-12.8416149007883,1.29851989865549,4.6986955622137));
#86541=CARTESIAN_POINT('Ctrl Pts',(-12.8009604323891,1.22557383705823,4.69342439545446));
#86542=CARTESIAN_POINT('Ctrl Pts',(-12.7605475893236,1.15306132230515,4.68818455729149));
#86543=CARTESIAN_POINT('Ctrl Pts',(-12.7236957990021,1.07849512938316,4.68294471912852));
#86544=CARTESIAN_POINT('Ctrl Pts',(-12.6906105599817,1.00226077661048,4.67770488096555));
#86545=CARTESIAN_POINT('Ctrl Pts',(-12.6575361103228,0.926051284471185,
4.6724667515558));
#86546=CARTESIAN_POINT('Ctrl Pts',(-12.6282259558573,0.848175135617082,
4.66722862214605));
#86547=CARTESIAN_POINT('Ctrl Pts',(-12.6028383473798,0.769039830702783,
4.66199049273629));
#86548=CARTESIAN_POINT('Ctrl Pts',(-12.5774513715141,0.689906497692163,
4.65675249385092));
#86549=CARTESIAN_POINT('Ctrl Pts',(-12.5559868871348,0.609514510427808,
4.65151449496555));
#86550=CARTESIAN_POINT('Ctrl Pts',(-12.5385535162026,0.528287286806343,
4.64627649608018));
#86551=CARTESIAN_POINT('Ctrl Pts',(-12.5209286000478,0.446167597425535,
4.64098094586603));
#86552=CARTESIAN_POINT('Ctrl Pts',(-12.5074240417744,0.363194671680445,
4.63568539565187));
#86553=CARTESIAN_POINT('Ctrl Pts',(-12.4980988283269,0.27981561282562,4.63038984543772));
#86554=CARTESIAN_POINT('Ctrl Pts',(-12.4888617644595,0.197224721347708,
4.62514435311554));
#86555=CARTESIAN_POINT('Ctrl Pts',(-12.4837253326637,0.114235811919584,
4.61989886079337));
#86556=CARTESIAN_POINT('Ctrl Pts',(-12.482694406598,0.0312857703605018,
4.6146533684712));
#86557=CARTESIAN_POINT('Ctrl Pts',(-12.4816487232943,-0.0528516633340902,
4.60933278931105));
#86558=CARTESIAN_POINT('Ctrl Pts',(-12.4848269926099,-0.136948615955238,
4.60401221015091));
#86559=CARTESIAN_POINT('Ctrl Pts',(-12.4921797979398,-0.220554039043703,
4.59869163099077));
#86560=CARTESIAN_POINT('Ctrl Pts',(-12.4995326032696,-0.304159462132168,
4.59337105183062));
#86561=CARTESIAN_POINT('Ctrl Pts',(-12.5110598141303,-0.38727288095522,
4.58805047267048));
#86562=CARTESIAN_POINT('Ctrl Pts',(-12.5266585556508,-0.469455375583696,
4.58272989351034));
#86563=CARTESIAN_POINT('Ctrl Pts',(-12.5420700921414,-0.550651574212894,
4.57747316816679));
#86564=CARTESIAN_POINT('Ctrl Pts',(-12.5615124562054,-0.631236973215575,
4.57221644282324));
#86565=CARTESIAN_POINT('Ctrl Pts',(-12.5849231616556,-0.710781341125662,
4.56695971747969));
#86566=CARTESIAN_POINT('Ctrl Pts',(-12.6083008235378,-0.790213434344449,
4.56171041185964));
#86567=CARTESIAN_POINT('Ctrl Pts',(-12.6356355718122,-0.868606976466571,
4.55646110623958));
#86568=CARTESIAN_POINT('Ctrl Pts',(-12.6668138050427,-0.94554134212144,
4.55121180061953));
#86569=CARTESIAN_POINT('Ctrl Pts',(-12.6981216531792,-1.02279554118366,
4.54594067245907));
#86570=CARTESIAN_POINT('Ctrl Pts',(-12.7333049283758,-1.09857794117082,
4.54066954429862));
#86571=CARTESIAN_POINT('Ctrl Pts',(-12.7721977519031,-1.17247745964443,
4.53539841613816));
#86572=CARTESIAN_POINT('Ctrl Pts',(-12.8108608814067,-1.24594054084748,
4.53015841831299));
#86573=CARTESIAN_POINT('Ctrl Pts',(-12.8531896473533,-1.31754250667629,
4.52491842048781));
#86574=CARTESIAN_POINT('Ctrl Pts',(-12.8989733665958,-1.38690062215215,
4.51967842266263));
#86575=CARTESIAN_POINT('Ctrl Pts',(-12.9447421664479,-1.45623613612651,
4.51444013237836));
#86576=CARTESIAN_POINT('Ctrl Pts',(-12.993963429686,-1.52332886746602,4.50920184209408));
#86577=CARTESIAN_POINT('Ctrl Pts',(-13.04638225176,-1.58782365008259,4.5039635518098));
#86578=CARTESIAN_POINT('Ctrl Pts',(-13.0987997776424,-1.65231683789809,
4.49872539105586));
#86579=CARTESIAN_POINT('Ctrl Pts',(-13.154414413487,-1.71421184757884,4.49348723030191));
#86580=CARTESIAN_POINT('Ctrl Pts',(-13.2129308127959,-1.77318638900303,
4.48824906954797));
#86581=CARTESIAN_POINT('Ctrl Pts',(-13.2720862178385,-1.83280493912491,
4.48295370748302));
#86582=CARTESIAN_POINT('Ctrl Pts',(-13.3342068223973,-1.88943849383192,
4.47765834541808));
#86583=CARTESIAN_POINT('Ctrl Pts',(-13.3989503966091,-1.94279345723676,
4.47236298335313));
#86584=CARTESIAN_POINT('Ctrl Pts',(-13.463086228857,-1.99564758251758,4.46711732836384));
#86585=CARTESIAN_POINT('Ctrl Pts',(-13.5297955828649,-2.04528418147697,
4.46187167337454));
#86586=CARTESIAN_POINT('Ctrl Pts',(-13.5987151606304,-2.09146050619011,
4.45662601838525));
#86587=CARTESIAN_POINT('Ctrl Pts',(-13.6686143464734,-2.13829317126612,
4.45130580278248));
#86588=CARTESIAN_POINT('Ctrl Pts',(-13.7407866586839,-2.18156617012225,
4.4459855871797));
#86589=CARTESIAN_POINT('Ctrl Pts',(-13.8148274004604,-2.22107455059496,
4.44066537157692));
#86590=CARTESIAN_POINT('Ctrl Pts',(-13.888868142237,-2.26058293106766,4.43534515597415));
#86591=CARTESIAN_POINT('Ctrl Pts',(-13.9647768449265,-2.29632654319577,
4.43002494037137));
#86592=CARTESIAN_POINT('Ctrl Pts',(-14.0421297747511,-2.32815181669531,
4.42470472476859));
#86593=CARTESIAN_POINT('Ctrl Pts',(-14.1185591457568,-2.35959711089642,
4.41944803012165));
#86594=CARTESIAN_POINT('Ctrl Pts',(-14.1966787820551,-2.38733251946412,
4.4141913354747));
#86595=CARTESIAN_POINT('Ctrl Pts',(-14.2760941871876,-2.41117536155635,
4.40893464082776));
#86596=CARTESIAN_POINT('Ctrl Pts',(-14.3553974971509,-2.43498454937946,
4.4036853660268));
#86597=CARTESIAN_POINT('Ctrl Pts',(-14.4359925049753,-2.45491195290006,
4.39843609122585));
#86598=CARTESIAN_POINT('Ctrl Pts',(-14.517464837691,-2.47082295341763,4.3931868164249));
#86599=CARTESIAN_POINT('Ctrl Pts',(-14.5992764688284,-2.48680021664284,
4.38791568057498));
#86600=CARTESIAN_POINT('Ctrl Pts',(-14.6819723137276,-2.49872736740562,
4.38264454472506));
#86601=CARTESIAN_POINT('Ctrl Pts',(-14.7651174257217,-2.506518786345,4.37737340887515));
#86602=CARTESIAN_POINT('Ctrl Pts',(-14.8477708899315,-2.51426413361802,
4.37213344193221));
#86603=CARTESIAN_POINT('Ctrl Pts',(-14.930867858799,-2.51792248063566,4.36689347498927));
#86604=CARTESIAN_POINT('Ctrl Pts',(-15.0139726641947,-2.51746122406191,
4.36165350804633));
#86605=CARTESIAN_POINT('Ctrl Pts',(-15.0970503890841,-2.51700011779309,
4.35641524859741));
#86606=CARTESIAN_POINT('Ctrl Pts',(-15.1801354846832,-2.51242207668247,
4.35117698914848));
#86607=CARTESIAN_POINT('Ctrl Pts',(-15.2627912183508,-2.50374659771266,
4.34593872969956));
#86608=CARTESIAN_POINT('Ctrl Pts',(-15.3454449095488,-2.4950713331188,4.34070059969096));
#86609=CARTESIAN_POINT('Ctrl Pts',(-15.4276688014327,-2.48229888118847,
4.33546246968237));
#86610=CARTESIAN_POINT('Ctrl Pts',(-15.5090316067901,-2.46550057255899,
4.33022433967377));
#86611=CARTESIAN_POINT('Ctrl Pts',(-15.591283954079,-2.44851860752976,4.32492894103653));
#86612=CARTESIAN_POINT('Ctrl Pts',(-15.6726557964936,-2.42742229782486,
4.31963354239929));
#86613=CARTESIAN_POINT('Ctrl Pts',(-15.7527142546424,-2.40233792395204,
4.31433814376204));
#86614=CARTESIAN_POINT('Ctrl Pts',(-15.83202020704,-2.3774893294839,4.30909251897782));
#86615=CARTESIAN_POINT('Ctrl Pts',(-15.9100369455761,-2.3487275469003,4.3038468941936));
#86616=CARTESIAN_POINT('Ctrl Pts',(-15.9863626897743,-2.31622427545806,
4.29860126940938));
#86617=CARTESIAN_POINT('Ctrl Pts',(-16.0637747754083,-2.28325838618039,
4.29328098384563));
#86618=CARTESIAN_POINT('Ctrl Pts',(-16.1394469105356,-2.24644388140251,
4.28796069828187));
#86619=CARTESIAN_POINT('Ctrl Pts',(-16.2129863368797,-2.20600779612022,
4.28264041271812));
#86620=CARTESIAN_POINT('Ctrl Pts',(-16.2865257632238,-2.16557171083793,
4.27732012715437));
#86621=CARTESIAN_POINT('Ctrl Pts',(-16.3579320991304,-2.12151435572198,
4.27199984159062));
#86622=CARTESIAN_POINT('Ctrl Pts',(-16.4268452282784,-2.07410678233767,
4.26667955602687));
#86623=CARTESIAN_POINT('Ctrl Pts',(-16.4946545814488,-2.02745853219561,
4.26144448504373));
#86624=CARTESIAN_POINT('Ctrl Pts',(-16.5603033967977,-1.97739226031036,
4.2562094140606));
#86625=CARTESIAN_POINT('Ctrl Pts',(-16.6234248823249,-1.92413562449436,
4.25097434307746));
#86626=CARTESIAN_POINT('Ctrl Pts',(-16.6864570895403,-1.87095431425895,
4.24574667651925));
#86627=CARTESIAN_POINT('Ctrl Pts',(-16.7469687131128,-1.81459189887532,
4.24051900996103));
#86628=CARTESIAN_POINT('Ctrl Pts',(-16.8046221950517,-1.75531905451028,
4.23529134340281));
#86629=CARTESIAN_POINT('Ctrl Pts',(-16.8622102350915,-1.6961134901667,4.23006961071738));
#86630=CARTESIAN_POINT('Ctrl Pts',(-16.9169462578319,-1.63400439384777,
4.22484787803195));
#86631=CARTESIAN_POINT('Ctrl Pts',(-16.9685271800743,-1.56930143417665,
4.21962614534652));
#86632=CARTESIAN_POINT('Ctrl Pts',(-17.0200762519165,-1.50463842755525,
4.21440763699807));
#86633=CARTESIAN_POINT('Ctrl Pts',(-17.06847380093,-1.43738509969373,4.20918912864962));
#86634=CARTESIAN_POINT('Ctrl Pts',(-17.1134557013779,-1.36788568539674,
4.20397062030117));
#86635=CARTESIAN_POINT('Ctrl Pts',(-17.1584236734685,-1.2984077911481,4.1987537278304));
#86636=CARTESIAN_POINT('Ctrl Pts',(-17.1999778445977,-1.22668558204242,
4.19353683535962));
#86637=CARTESIAN_POINT('Ctrl Pts',(-17.2378971126337,-1.15309269500148,
4.18831994288885));
#86638=CARTESIAN_POINT('Ctrl Pts',(-17.2758163121788,-1.07949994088627,
4.18310305984098));
#86639=CARTESIAN_POINT('Ctrl Pts',(-17.3101004099534,-1.00403693001966,
4.17788617679312));
#86640=CARTESIAN_POINT('Ctrl Pts',(-17.3405746914721,-0.927101053629093,
4.17266929374526));
#86641=CARTESIAN_POINT('Ctrl Pts',(-17.371078541097,-0.850090529107456,
4.16744734894223));
#86642=CARTESIAN_POINT('Ctrl Pts',(-17.3977650199345,-0.771604718545424,
4.1622254041392));
#86643=CARTESIAN_POINT('Ctrl Pts',(-17.4205081717154,-0.692059564386758,
4.15700345933618));
#86644=CARTESIAN_POINT('Ctrl Pts',(-17.4432623819275,-0.612475732887851,
4.15177897546037));
#86645=CARTESIAN_POINT('Ctrl Pts',(-17.462069340882,-0.531831985657823,
4.14655449158456));
#86646=CARTESIAN_POINT('Ctrl Pts',(-17.4768540464178,-0.450555526815343,
4.14133000770875));
#86647=CARTESIAN_POINT('Ctrl Pts',(-17.4916642936618,-0.369138656681709,
4.13609649813797));
#86648=CARTESIAN_POINT('Ctrl Pts',(-17.5024383459796,-0.287087353593853,
4.13086298856718));
#86649=CARTESIAN_POINT('Ctrl Pts',(-17.5091530374981,-0.204834773449096,
4.12562947899639));
#86650=CARTESIAN_POINT('Ctrl Pts',(-17.514732534348,-0.136487923776358,
4.12128075350637));
#86651=CARTESIAN_POINT('Ctrl Pts',(-17.5175101608992,-0.0680022946564488,
4.11693202801635));
#86652=CARTESIAN_POINT('Ctrl Pts',(-17.5174999720511,0.000375130022128299,
4.11258330252632));
#86653=CARTESIAN_POINT('Ctrl Pts',(-17.5174999720511,0.000375130562157188,
4.11258330249198));
#86654=CARTESIAN_POINT('Ctrl Pts',(-17.5174969036288,0.0209673020875996,
4.1112736640897));
#86655=CARTESIAN_POINT('Ctrl Pts',(-17.5172411859996,0.0415573205068692,
4.10996402568741));
#86656=CARTESIAN_POINT('Ctrl Pts',(-17.5167329489669,0.0621410780745678,
4.10865438728513));
#86657=CARTESIAN_POINT('Ctrl Pts',(-17.5146933424961,0.144745773182198,
4.10339867629233));
#86658=CARTESIAN_POINT('Ctrl Pts',(-17.5085787900268,0.227401427432359,
4.09814296529952));
#86659=CARTESIAN_POINT('Ctrl Pts',(-17.4983811757245,0.309673619776567,
4.09288725430672));
#86660=CARTESIAN_POINT('Ctrl Pts',(-17.4881961889154,0.391843936179619,
4.08763805135131));
#86661=CARTESIAN_POINT('Ctrl Pts',(-17.4739382300675,0.473631279449932,
4.0823888483959));
#86662=CARTESIAN_POINT('Ctrl Pts',(-17.4556511682864,0.554602190487785,
4.07713964544048));
#86663=CARTESIAN_POINT('Ctrl Pts',(-17.4373846463994,0.635482155589933,
4.07189633835148));
#86664=CARTESIAN_POINT('Ctrl Pts',(-17.415098116769,0.715547063496811,4.06665303126248));
#86665=CARTESIAN_POINT('Ctrl Pts',(-17.3888869213139,0.794371152028817,
4.06140972417347));
#86666=CARTESIAN_POINT('Ctrl Pts',(-17.3801667292314,0.820595106365506,
4.05966533044516));
#86667=CARTESIAN_POINT('Ctrl Pts',(-17.3710125657857,0.846681805097609,
4.05792093671685));
#86668=CARTESIAN_POINT('Ctrl Pts',(-17.3614291890287,0.872615857753799,
4.05617654298853));
#86669=CARTESIAN_POINT('',(-17.5174990478294,-0.00218956111536468,4.38741669750802));
#86670=CARTESIAN_POINT('Ctrl Pts',(-17.3578782887762,0.871321062777582,
4.33113094084205));
#86671=CARTESIAN_POINT('Ctrl Pts',(-17.4602182294948,0.591631726374291,
4.3498927182036));
#86672=CARTESIAN_POINT('Ctrl Pts',(-17.515530076098,0.294291473546931,4.36865449556515));
#86673=CARTESIAN_POINT('Ctrl Pts',(-17.518221775146,-0.00218348048635318,
4.3874162729267));
#86674=CARTESIAN_POINT('Ctrl Pts',(-17.5174990478294,-0.00218956111536468,
4.38741669750802));
#86675=CARTESIAN_POINT('Ctrl Pts',(-17.5173973207564,-0.119152639980189,
4.39482064288431));
#86676=CARTESIAN_POINT('Ctrl Pts',(-17.5091409213801,-0.23577079206408,
4.40222458826058));
#86677=CARTESIAN_POINT('Ctrl Pts',(-17.4928938724097,-0.351121618392081,
4.40962853363686));
#86678=CARTESIAN_POINT('Ctrl Pts',(-17.4854916683259,-0.403675799725012,
4.41300179328546));
#86679=CARTESIAN_POINT('Ctrl Pts',(-17.4764314300592,-0.455967350040209,
4.41637505293405));
#86680=CARTESIAN_POINT('Ctrl Pts',(-17.4657317181364,-0.507910763989177,
4.41974831258264));
#86681=CARTESIAN_POINT('Ctrl Pts',(-17.4490575762057,-0.588857976661858,
4.42500510926611));
#86682=CARTESIAN_POINT('Ctrl Pts',(-17.4283625240479,-0.669131684515691,
4.43026190594957));
#86683=CARTESIAN_POINT('Ctrl Pts',(-17.4037157400883,-0.748302673289332,
4.43551870263304));
#86684=CARTESIAN_POINT('Ctrl Pts',(-17.3791037492572,-0.827361898743446,
4.44076807845367));
#86685=CARTESIAN_POINT('Ctrl Pts',(-17.3505512434199,-0.905321060575425,
4.44601745427432));
#86686=CARTESIAN_POINT('Ctrl Pts',(-17.3181783604909,-0.981761345211712,
4.45126683009496));
#86687=CARTESIAN_POINT('Ctrl Pts',(-17.2856714400657,-1.0585181251189,4.45653794056285));
#86688=CARTESIAN_POINT('Ctrl Pts',(-17.2493125292196,-1.13374296044936,
4.46180905103074));
#86689=CARTESIAN_POINT('Ctrl Pts',(-17.2092738793896,-1.20702741304689,
4.46708016149863));
#86690=CARTESIAN_POINT('Ctrl Pts',(-17.1694710484767,-1.27988023619848,
4.47232022627525));
#86691=CARTESIAN_POINT('Ctrl Pts',(-17.1260319282515,-1.35081506157744,
4.47756029105186));
#86692=CARTESIAN_POINT('Ctrl Pts',(-17.0791731360148,-1.41945247207302,
4.48280035582848));
#86693=CARTESIAN_POINT('Ctrl Pts',(-17.0323296254735,-1.48806749838096,
4.48803871170331));
#86694=CARTESIAN_POINT('Ctrl Pts',(-16.9820689176839,-1.55438621736842,
4.49327706757815));
#86695=CARTESIAN_POINT('Ctrl Pts',(-16.9286514171008,-1.61805746539338,
4.49851542345298));
#86696=CARTESIAN_POINT('Ctrl Pts',(-16.8752352520899,-1.68172712147643,
4.50375364835569));
#86697=CARTESIAN_POINT('Ctrl Pts',(-16.8186627483982,-1.7427490856614,4.50899187325841));
#86698=CARTESIAN_POINT('Ctrl Pts',(-16.7592342361937,-1.80080569529415,
4.51423009816112));
#86699=CARTESIAN_POINT('Ctrl Pts',(-16.6991584027456,-1.8594946828101,4.51952538009139));
#86700=CARTESIAN_POINT('Ctrl Pts',(-16.6361642955416,-1.91515297357877,
4.52482066202166));
#86701=CARTESIAN_POINT('Ctrl Pts',(-16.5705986478698,-1.96749234745897,
4.53011594395194));
#86702=CARTESIAN_POINT('Ctrl Pts',(-16.5056467332036,-2.01934179403145,
4.53536165893046));
#86703=CARTESIAN_POINT('Ctrl Pts',(-16.4381716337318,-2.06793397575382,
4.54060737390898));
#86704=CARTESIAN_POINT('Ctrl Pts',(-16.3685403852193,-2.11303181803396,
4.5458530888875));
#86705=CARTESIAN_POINT('Ctrl Pts',(-16.2979222144046,-2.15876885704368,
4.55117315429365));
#86706=CARTESIAN_POINT('Ctrl Pts',(-16.2250867211346,-2.20091148074323,
4.55649321969979));
#86707=CARTESIAN_POINT('Ctrl Pts',(-16.1504416994653,-2.23926107145446,
4.56181328510594));
#86708=CARTESIAN_POINT('Ctrl Pts',(-16.075796677796,-2.2776106621657,4.56713335051208));
#86709=CARTESIAN_POINT('Ctrl Pts',(-15.9993425985454,-2.31216707724679,
4.57245341591823));
#86710=CARTESIAN_POINT('Ctrl Pts',(-15.9215054899763,-2.34278336214503,
4.57777348132438));
#86711=CARTESIAN_POINT('Ctrl Pts',(-15.8445922977486,-2.37303623572891,
4.58303039824702));
#86712=CARTESIAN_POINT('Ctrl Pts',(-15.7660467606654,-2.39955297748993,
4.58828731516967));
#86713=CARTESIAN_POINT('Ctrl Pts',(-15.6862662133858,-2.42215708292529,
4.59354423209231));
#86714=CARTESIAN_POINT('Ctrl Pts',(-15.6065982441887,-2.44472929177766,
4.59879373099581));
#86715=CARTESIAN_POINT('Ctrl Pts',(-15.5256991663836,-2.46339970646124,
4.60404322989931));
#86716=CARTESIAN_POINT('Ctrl Pts',(-15.4439854369365,-2.47804018970401,
4.60929272880281));
#86717=CARTESIAN_POINT('Ctrl Pts',(-15.3619357752006,-2.49274086125392,
4.61456380885545));
#86718=CARTESIAN_POINT('Ctrl Pts',(-15.2790651864459,-2.50337821925715,
4.61983488890809));
#86719=CARTESIAN_POINT('Ctrl Pts',(-15.1958098629986,-2.50987345249765,
4.62510596896073));
#86720=CARTESIAN_POINT('Ctrl Pts',(-15.1130423798701,-2.51633062647031,
4.63034616275568));
#86721=CARTESIAN_POINT('Ctrl Pts',(-15.0298951229203,-2.51869404835166,
4.63558635655064));
#86722=CARTESIAN_POINT('Ctrl Pts',(-14.9468042475614,-2.51693791379972,
4.6408265503456));
#86723=CARTESIAN_POINT('Ctrl Pts',(-14.8637404387927,-2.51518235130307,
4.64606503716398));
#86724=CARTESIAN_POINT('Ctrl Pts',(-14.7807334357432,-2.5093099073547,4.65130352398236));
#86725=CARTESIAN_POINT('Ctrl Pts',(-14.6982196453878,-2.49934688820302,
4.65654201080074));
#86726=CARTESIAN_POINT('Ctrl Pts',(-14.615707890731,-2.4893841148491,4.66178036838036));
#86727=CARTESIAN_POINT('Ctrl Pts',(-14.5336897821847,-2.47533102329068,
4.66701872595997));
#86728=CARTESIAN_POINT('Ctrl Pts',(-14.4525954739112,-2.45726566223871,
4.67225708353958));
#86729=CARTESIAN_POINT('Ctrl Pts',(-14.3706222710231,-2.43900451002857,
4.67755221408346));
#86730=CARTESIAN_POINT('Ctrl Pts',(-14.2895934871098,-2.41664367885642,
4.68284734462734));
#86731=CARTESIAN_POINT('Ctrl Pts',(-14.2099398926202,-2.39031614576965,
4.68814247517121));
#86732=CARTESIAN_POINT('Ctrl Pts',(-14.131027608002,-2.36423363439584,4.69338832567233));
#86733=CARTESIAN_POINT('Ctrl Pts',(-14.0534654349526,-2.33425817370456,
4.69863417617345));
#86734=CARTESIAN_POINT('Ctrl Pts',(-13.9776524634773,-2.30056770484286,
4.70388002667457));
#86735=CARTESIAN_POINT('Ctrl Pts',(-13.9007712000801,-2.26640249854467,
4.70919979723983));
#86736=CARTESIAN_POINT('Ctrl Pts',(-13.8256892569259,-2.22841699358774,
4.71451956780508));
#86737=CARTESIAN_POINT('Ctrl Pts',(-13.7527956831576,-2.18684421988622,
4.71983933837034));
#86738=CARTESIAN_POINT('Ctrl Pts',(-13.6799021093894,-2.14527144618471,
4.7251591089356));
#86739=CARTESIAN_POINT('Ctrl Pts',(-13.6091972815012,-2.10011172003563,
4.73047887950086));
#86740=CARTESIAN_POINT('Ctrl Pts',(-13.5410369466336,-2.05164155224831,
4.73579865006611));
#86741=CARTESIAN_POINT('Ctrl Pts',(-13.473696553835,-2.00375446155025,4.74105442588));
#86742=CARTESIAN_POINT('Ctrl Pts',(-13.4085925676905,-1.9524604078873,4.74631020169388));
#86743=CARTESIAN_POINT('Ctrl Pts',(-13.34608980551,-1.8979956055171,4.75156597750776));
#86744=CARTESIAN_POINT('Ctrl Pts',(-13.2836753032737,-1.84360771271447,
4.75681433165797));
#86745=CARTESIAN_POINT('Ctrl Pts',(-13.2238550738078,-1.78605826529202,
4.76206268580818));
#86746=CARTESIAN_POINT('Ctrl Pts',(-13.1669638793344,-1.72562592421854,
4.76731103995839));
#86747=CARTESIAN_POINT('Ctrl Pts',(-13.1098232429645,-1.66492861493858,
4.77258240574378));
#86748=CARTESIAN_POINT('Ctrl Pts',(-13.0556377736257,-1.60132334255888,
4.77785377152917));
#86749=CARTESIAN_POINT('Ctrl Pts',(-13.0047119500196,-1.53513251792973,
4.78312513731457));
#86750=CARTESIAN_POINT('Ctrl Pts',(-12.9540983377516,-1.4693474898979,4.78836418589722));
#86751=CARTESIAN_POINT('Ctrl Pts',(-12.9067048014093,-1.4010088916989,4.79360323447988));
#86752=CARTESIAN_POINT('Ctrl Pts',(-12.8627911517787,-1.33046780836091,
4.79884228306254));
#86753=CARTESIAN_POINT('Ctrl Pts',(-12.8188917901316,-1.25994967665272,
4.80407962703991));
#86754=CARTESIAN_POINT('Ctrl Pts',(-12.7784703100671,-1.18723087437197,
4.80931697101728));
#86755=CARTESIAN_POINT('Ctrl Pts',(-12.7417430134631,-1.11269116683712,
4.81455431499465));
#86756=CARTESIAN_POINT('Ctrl Pts',(-12.7050165957296,-1.0381532430097,4.81979153364433));
#86757=CARTESIAN_POINT('Ctrl Pts',(-12.6719843886013,-0.961794914831745,
4.82502875229401));
#86758=CARTESIAN_POINT('Ctrl Pts',(-12.6428159385109,-0.884018976188743,
4.83026597094369));
#86759=CARTESIAN_POINT('Ctrl Pts',(-12.6133173942567,-0.805362861075901,
4.8355624582657));
#86760=CARTESIAN_POINT('Ctrl Pts',(-12.5877707965439,-0.725257292009281,
4.84085894558771));
#86761=CARTESIAN_POINT('Ctrl Pts',(-12.5663001805094,-0.644136195700586,
4.84615543290973));
#86762=CARTESIAN_POINT('Ctrl Pts',(-12.5450393644627,-0.563807773667335,
4.85140016563964));
#86763=CARTESIAN_POINT('Ctrl Pts',(-12.5277752568343,-0.482484053626239,
4.85664489836955));
#86764=CARTESIAN_POINT('Ctrl Pts',(-12.514576737485,-0.400596375607034,
4.86188963109946));
#86765=CARTESIAN_POINT('Ctrl Pts',(-12.5011828552773,-0.317496606259529,
4.86721199571752));
#86766=CARTESIAN_POINT('Ctrl Pts',(-12.4919759534833,-0.23381653791337,
4.87253436033559));
#86767=CARTESIAN_POINT('Ctrl Pts',(-12.4869732965618,-0.150010125680739,
4.87785672495365));
#86768=CARTESIAN_POINT('Ctrl Pts',(-12.4819706396403,-0.06620371344811,
4.88317908957172));
#86769=CARTESIAN_POINT('Ctrl Pts',(-12.4811721678482,0.0177285526205801,
4.88850145418978));
#86770=CARTESIAN_POINT('Ctrl Pts',(-12.4845403831624,0.10133689386932,4.89382381880785));
#86771=CARTESIAN_POINT('Ctrl Pts',(-12.4878677084383,0.183930232228006,
4.89908157007049));
#86772=CARTESIAN_POINT('Ctrl Pts',(-12.4952732739897,0.266510778938183,
4.90433932133313));
#86773=CARTESIAN_POINT('Ctrl Pts',(-12.5067583652682,0.348643658826417,
4.90959707259578));
#86774=CARTESIAN_POINT('Ctrl Pts',(-12.5182272379199,0.430660555089282,
4.91484739914552));
#86775=CARTESIAN_POINT('Ctrl Pts',(-12.5337641298177,0.512230587528115,
4.92009772569527));
#86776=CARTESIAN_POINT('Ctrl Pts',(-12.5533183550739,0.592920887118621,
4.92534805224501));
#86777=CARTESIAN_POINT('Ctrl Pts',(-12.5729491005826,0.673926946706005,
4.93061892454937));
#86778=CARTESIAN_POINT('Ctrl Pts',(-12.5966286687847,0.754045903688691,
4.93588979685373));
#86779=CARTESIAN_POINT('Ctrl Pts',(-12.6242533434921,0.832846969191615,
4.94116066915808));
#86780=CARTESIAN_POINT('Ctrl Pts',(-12.6517214538202,0.911201425275966,
4.9464016685007));
#86781=CARTESIAN_POINT('Ctrl Pts',(-12.6830899182278,0.988252448999663,
4.95164266784331));
#86782=CARTESIAN_POINT('Ctrl Pts',(-12.7182064727464,1.06359040470633,4.95688366718592));
#86783=CARTESIAN_POINT('Ctrl Pts',(-12.7533115226655,1.13890367880604,4.96212294951505));
#86784=CARTESIAN_POINT('Ctrl Pts',(-12.7921620292958,1.21250458212242,4.96736223184418));
#86785=CARTESIAN_POINT('Ctrl Pts',(-12.8345579389069,1.28400425624248,4.9726015141733));
#86786=CARTESIAN_POINT('Ctrl Pts',(-12.8769527132436,1.35550201574984,4.97784065620534));
#86787=CARTESIAN_POINT('Ctrl Pts',(-12.9228924657952,1.42489826202544,4.98307979823737));
#86788=CARTESIAN_POINT('Ctrl Pts',(-12.9721323109669,1.49183071619249,4.9883189402694));
#86789=CARTESIAN_POINT('Ctrl Pts',(-13.0218893397688,1.55946618576321,4.99361311087609));
#86790=CARTESIAN_POINT('Ctrl Pts',(-13.075015922983,1.62458540544535,4.99890728148277));
#86791=CARTESIAN_POINT('Ctrl Pts',(-13.1312169528721,1.68684799930738,5.00420145208945));
#86792=CARTESIAN_POINT('Ctrl Pts',(-13.1869129908552,1.74855113534443,5.00944805215676));
#86793=CARTESIAN_POINT('Ctrl Pts',(-13.2456280739797,1.8074484890672,5.01469465222407));
#86794=CARTESIAN_POINT('Ctrl Pts',(-13.3070384299949,1.86324646047852,5.01994125229138));
#86795=CARTESIAN_POINT('Ctrl Pts',(-13.3692839908249,1.91980330608318,5.02525920816775));
#86796=CARTESIAN_POINT('Ctrl Pts',(-13.4342983110701,1.97317551832977,5.03057716404411));
#86797=CARTESIAN_POINT('Ctrl Pts',(-13.5017117827493,2.0231012500732,5.03589511992048));
#86798=CARTESIAN_POINT('Ctrl Pts',(-13.5691252544285,2.07302698181663,5.04121307579685));
#86799=CARTESIAN_POINT('Ctrl Pts',(-13.638937437613,2.11950601640244,5.04653103167322));
#86800=CARTESIAN_POINT('Ctrl Pts',(-13.7107523908196,2.16232440957011,5.05184898754958));
#86801=CARTESIAN_POINT('Ctrl Pts',(-13.7817561485304,2.20465914179915,5.05710687373766));
#86802=CARTESIAN_POINT('Ctrl Pts',(-13.8549769818467,2.24357018102277,5.06236475992573));
#86803=CARTESIAN_POINT('Ctrl Pts',(-13.9300512283673,2.27881896518385,5.06762264611381));
#86804=CARTESIAN_POINT('Ctrl Pts',(-14.0050197533126,2.31401811105805,5.07287312800499));
#86805=CARTESIAN_POINT('Ctrl Pts',(-14.0818360932399,2.34556505186817,5.07812360989618));
#86806=CARTESIAN_POINT('Ctrl Pts',(-14.1601098903681,2.37326586242301,5.08337409178736));
#86807=CARTESIAN_POINT('Ctrl Pts',(-14.2386871253636,2.40107405852944,5.08864492780836));
#86808=CARTESIAN_POINT('Ctrl Pts',(-14.3187327372534,2.42500600131077,5.09391576382936));
#86809=CARTESIAN_POINT('Ctrl Pts',(-14.3998292064608,2.44491334582281,5.09918659985036));
#86810=CARTESIAN_POINT('Ctrl Pts',(-14.4804697388657,2.4647087681872,5.1044278024219));
#86811=CARTESIAN_POINT('Ctrl Pts',(-14.5621488918436,2.48052461483988,5.10966900499344));
#86812=CARTESIAN_POINT('Ctrl Pts',(-14.6444403075757,2.49226474418813,5.11491020756499));
#86813=CARTESIAN_POINT('Ctrl Pts',(-14.726705037857,2.5040010664486,5.12014971051996));
#86814=CARTESIAN_POINT('Ctrl Pts',(-14.8095811806631,2.5116642314104,5.12538921347494));
#86815=CARTESIAN_POINT('Ctrl Pts',(-14.8926336900799,2.51520947944583,5.13062871642992));
#86816=CARTESIAN_POINT('Ctrl Pts',(-14.9756842447002,2.51875464403719,5.13586809606337));
#86817=CARTESIAN_POINT('Ctrl Pts',(-15.0589106971921,2.51818206584989,5.14110747569682));
#86818=CARTESIAN_POINT('Ctrl Pts',(-15.141875788897,2.51349905719594,5.14634685533028));
#86819=CARTESIAN_POINT('Ctrl Pts',(-15.2257048666175,2.50876728039258,5.15164079707703));
#86820=CARTESIAN_POINT('Ctrl Pts',(-15.3092666282684,2.49983897237347,5.15693473882378));
#86821=CARTESIAN_POINT('Ctrl Pts',(-15.3921148617149,2.48677545934938,5.16222868057053));
#86822=CARTESIAN_POINT('Ctrl Pts',(-15.4742265400234,2.47382808637122,5.16747555698069));
#86823=CARTESIAN_POINT('Ctrl Pts',(-15.5556368833323,2.45681889943722,5.17272243339085));
#86824=CARTESIAN_POINT('Ctrl Pts',(-15.6359230890096,2.43585879616708,5.17796930980101));
#86825=CARTESIAN_POINT('Ctrl Pts',(-15.7172895652132,2.41461666958296,5.18328678421606));
#86826=CARTESIAN_POINT('Ctrl Pts',(-15.7975009604204,2.38931666101742,5.18860425863111));
#86827=CARTESIAN_POINT('Ctrl Pts',(-15.8761362235756,2.3601253288202,5.19392173304616));
#86828=CARTESIAN_POINT('Ctrl Pts',(-15.9547714867308,2.33093399662298,5.19923920746121));
#86829=CARTESIAN_POINT('Ctrl Pts',(-16.0318301964893,2.29785159087143,5.20455668187626));
#86830=CARTESIAN_POINT('Ctrl Pts',(-16.1069170379196,2.26109285991606,5.20987415629132));
#86831=CARTESIAN_POINT('Ctrl Pts',(-16.1810320417782,2.22480989162625,5.21512280744354));
#86832=CARTESIAN_POINT('Ctrl Pts',(-16.2534991811834,2.18481145602326,5.22037145859576));
#86833=CARTESIAN_POINT('Ctrl Pts',(-16.3239209991794,2.14127051955888,5.22562010974799));
#86834=CARTESIAN_POINT('Ctrl Pts',(-16.3942515227484,2.09778602930612,5.23086195658));
#86835=CARTESIAN_POINT('Ctrl Pts',(-16.4625415986379,2.05076839498171,5.23610380341202));
#86836=CARTESIAN_POINT('Ctrl Pts',(-16.5284163196141,2.00043740315396,5.24134565024404));
#86837=CARTESIAN_POINT('Ctrl Pts',(-16.59422562042,1.95015639502268,5.24658229139918));
#86838=CARTESIAN_POINT('Ctrl Pts',(-16.6576239638578,1.89656884220967,5.25181893255431));
#86839=CARTESIAN_POINT('Ctrl Pts',(-16.7182647135537,1.83993821204854,5.25705557370944));
#86840=CARTESIAN_POINT('Ctrl Pts',(-16.7788636298067,1.78334664892138,5.26228860233126));
#86841=CARTESIAN_POINT('Ctrl Pts',(-16.8367083944421,1.72371649346041,5.26752163095307));
#86842=CARTESIAN_POINT('Ctrl Pts',(-16.8914859137858,1.66135104296163,5.27275465957489));
#86843=CARTESIAN_POINT('Ctrl Pts',(-16.9462562311214,1.59899379211289,5.27798700017148));
#86844=CARTESIAN_POINT('Ctrl Pts',(-16.9979597897181,1.53390229933247,5.28321934076807));
#86845=CARTESIAN_POINT('Ctrl Pts',(-17.0463215667391,1.46641545801271,5.28845168136466));
#86846=CARTESIAN_POINT('Ctrl Pts',(-17.0946780400812,1.39893601775537,5.29368344814748));
#86847=CARTESIAN_POINT('Ctrl Pts',(-17.139693195972,1.32906213074443,5.29891521493029));
#86848=CARTESIAN_POINT('Ctrl Pts',(-17.1811344650775,1.25716295493104,5.3041469817131));
#86849=CARTESIAN_POINT('Ctrl Pts',(-17.2226042404479,1.18521432172907,5.30938234727879));
#86850=CARTESIAN_POINT('Ctrl Pts',(-17.2604949923158,1.11123802103591,5.31461771284448));
#86851=CARTESIAN_POINT('Ctrl Pts',(-17.2946197636733,1.03562850007135,5.31985307841017));
#86852=CARTESIAN_POINT('Ctrl Pts',(-17.3187960910826,0.982061532106858,
5.32356217028064));
#86853=CARTESIAN_POINT('Ctrl Pts',(-17.3410831330273,0.927675332202151,
5.32727126215111));
#86854=CARTESIAN_POINT('Ctrl Pts',(-17.3614291890287,0.872615857753799,
5.33098035402157));
#86855=CARTESIAN_POINT('Origin',(-15.,0.,8.20842344717746));
#86856=CARTESIAN_POINT('',(-18.0734988375387,-0.00267313449380446,4.70842344717746));
#86857=CARTESIAN_POINT('Ctrl Pts',(-13.1256826865589,2.43995710119902,5.35407232013781));
#86858=CARTESIAN_POINT('Ctrl Pts',(-12.4214282668293,1.88987704449842,5.30765840291763));
#86859=CARTESIAN_POINT('Ctrl Pts',(-11.4362126399874,0.0231526869172058,
5.20856942945022));
#86860=CARTESIAN_POINT('Ctrl Pts',(-12.8980243432311,-2.95589590321946,
5.05680539973554));
#86861=CARTESIAN_POINT('Ctrl Pts',(-16.3276370895773,-3.37529447323561,
4.89878023099381));
#86862=CARTESIAN_POINT('Ctrl Pts',(-17.9625769261592,-1.43265780425104,
4.78265291347444));
#86863=CARTESIAN_POINT('Ctrl Pts',(-18.0762683537743,-0.210587979812296,
4.71920065220233));
#86864=CARTESIAN_POINT('Ctrl Pts',(-18.0743812564454,-0.00267390196584321,
4.70842344717746));
#86865=CARTESIAN_POINT('Ctrl Pts',(-18.0734988375387,-0.00267313449380446,
4.70842344717746));
#86866=CARTESIAN_POINT('Ctrl Pts',(-18.0735813825829,0.0922349585720596,
4.70350244085089));
#86867=CARTESIAN_POINT('Ctrl Pts',(-18.0692636450065,0.187280803106169,
4.69858143452432));
#86868=CARTESIAN_POINT('Ctrl Pts',(-18.060534039328,0.282017098975876,4.69366042819775));
#86869=CARTESIAN_POINT('Ctrl Pts',(-18.0518123136726,0.376667878473905,
4.68874386395541));
#86870=CARTESIAN_POINT('Ctrl Pts',(-18.0386866748694,0.471009216033492,
4.68382729971307));
#86871=CARTESIAN_POINT('Ctrl Pts',(-18.0211975937825,0.564594854141415,
4.67891073547073));
#86872=CARTESIAN_POINT('Ctrl Pts',(-18.0037167736861,0.65813628694975,4.67399649357399));
#86873=CARTESIAN_POINT('Ctrl Pts',(-17.9818766860609,0.750922285092664,
4.66908225167725));
#86874=CARTESIAN_POINT('Ctrl Pts',(-17.9557693956204,0.842513815859346,
4.66416800978052));
#86875=CARTESIAN_POINT('Ctrl Pts',(-17.9296668378427,0.934088743147806,
4.65925465872497));
#86876=CARTESIAN_POINT('Ctrl Pts',(-17.8992987380668,1.02446919830555,4.65434130766943));
#86877=CARTESIAN_POINT('Ctrl Pts',(-17.8648075022904,1.11322963705626,4.64942795661389));
#86878=CARTESIAN_POINT('Ctrl Pts',(-17.8303124793768,1.20199982170196,4.64451406607246));
#86879=CARTESIAN_POINT('Ctrl Pts',(-17.7916935870412,1.28914921573111,4.63960017553104));
#86880=CARTESIAN_POINT('Ctrl Pts',(-17.7491415414118,1.37427182001377,4.63468628498961));
#86881=CARTESIAN_POINT('Ctrl Pts',(-17.7065467708575,1.45947989273455,4.62976746059362));
#86882=CARTESIAN_POINT('Ctrl Pts',(-17.6600111677927,1.54265670890348,4.62484863619764));
#86883=CARTESIAN_POINT('Ctrl Pts',(-17.609771422396,1.6234208859212,4.61992981180165));
#86884=CARTESIAN_POINT('Ctrl Pts',(-17.5595035797688,1.70423023135443,4.61500823648919));
#86885=CARTESIAN_POINT('Ctrl Pts',(-17.5055277299802,1.78262388120401,4.61008666117675));
#86886=CARTESIAN_POINT('Ctrl Pts',(-17.448122605106,1.85825131787087,4.60516508586429));
#86887=CARTESIAN_POINT('Ctrl Pts',(-17.390627285648,1.93399757990731,4.60023577780258));
#86888=CARTESIAN_POINT('Ctrl Pts',(-17.3296922277719,2.00696860864084,4.59530646974086));
#86889=CARTESIAN_POINT('Ctrl Pts',(-17.2656347354978,2.07684893415625,4.59037716167914));
#86890=CARTESIAN_POINT('Ctrl Pts',(-17.232508732449,2.1129860946021,4.58782807228954));
#86891=CARTESIAN_POINT('Ctrl Pts',(-17.1985482981898,2.14829736031872,4.58527898289994));
#86892=CARTESIAN_POINT('Ctrl Pts',(-17.1638007572219,2.18274335024668,4.58272989351033));
#86893=CARTESIAN_POINT('Ctrl Pts',(-17.0956315306495,2.25032098096535,4.57772897985392));
#86894=CARTESIAN_POINT('Ctrl Pts',(-17.0241745908414,2.31481993889649,4.5727280661975));
#86895=CARTESIAN_POINT('Ctrl Pts',(-16.949739211895,2.37590388180985,4.56772715254109));
#86896=CARTESIAN_POINT('Ctrl Pts',(-16.8754043569385,2.43690533167016,4.5627329925521));
#86897=CARTESIAN_POINT('Ctrl Pts',(-16.7980993933822,2.49450065668835,4.55773883256311));
#86898=CARTESIAN_POINT('Ctrl Pts',(-16.7181705057759,2.54839015126839,4.55274467257412));
#86899=CARTESIAN_POINT('Ctrl Pts',(-16.6383255019237,2.60222308991171,4.54775575385523));
#86900=CARTESIAN_POINT('Ctrl Pts',(-16.5558624102442,2.65235768582453,4.54276683513634));
#86901=CARTESIAN_POINT('Ctrl Pts',(-16.4711597656437,2.69853500884297,4.53777791641744));
#86902=CARTESIAN_POINT('Ctrl Pts',(-16.3865172554687,2.74467954838925,4.53279253956861));
#86903=CARTESIAN_POINT('Ctrl Pts',(-16.2996387372562,2.78687219081721,4.52780716271978));
#86904=CARTESIAN_POINT('Ctrl Pts',(-16.2109301182278,2.82489831653616,4.52282178587095));
#86905=CARTESIAN_POINT('Ctrl Pts',(-16.1222534637121,2.86291074024294,4.5178382054106));
#86906=CARTESIAN_POINT('Ctrl Pts',(-16.0317484214375,2.89675945764434,4.51285462495025));
#86907=CARTESIAN_POINT('Ctrl Pts',(-15.9398429224663,2.92627707695119,4.5078710444899));
#86908=CARTESIAN_POINT('Ctrl Pts',(-15.8479454918753,2.95579210490739,4.50288790153789));
#86909=CARTESIAN_POINT('Ctrl Pts',(-15.7546482667519,2.98097665682237,4.49790475858587));
#86910=CARTESIAN_POINT('Ctrl Pts',(-15.6603954428957,3.00171286251743,4.49292161563386));
#86911=CARTESIAN_POINT('Ctrl Pts',(-15.5661252060733,3.02245289917303,4.48793755205903));
#86912=CARTESIAN_POINT('Ctrl Pts',(-15.4708994483097,3.0387428632294,4.4829534884842));
#86913=CARTESIAN_POINT('Ctrl Pts',(-15.3751726340627,3.05051598006804,4.47796942490938));
#86914=CARTESIAN_POINT('Ctrl Pts',(-15.2793429939833,3.06230174310773,4.47298000765711));
#86915=CARTESIAN_POINT('Ctrl Pts',(-15.1830116590368,3.06956091934624,4.46799059040484));
#86916=CARTESIAN_POINT('Ctrl Pts',(-15.086638068938,3.07227864865977,4.46300117315258));
#86917=CARTESIAN_POINT('Ctrl Pts',(-14.9902073545031,3.07499798887606,4.45800879848067));
#86918=CARTESIAN_POINT('Ctrl Pts',(-14.8937347733996,3.07317053042643,4.45301642380876));
#86919=CARTESIAN_POINT('Ctrl Pts',(-14.7976774998649,3.06683352269716,4.44802404913685));
#86920=CARTESIAN_POINT('Ctrl Pts',(-14.7014664692317,3.06048637143701,4.44302368326329));
#86921=CARTESIAN_POINT('Ctrl Pts',(-14.6056725090362,3.04961530742927,4.43802331738972));
#86922=CARTESIAN_POINT('Ctrl Pts',(-14.5107453496793,3.03430916966936,4.43302295151615));
#86923=CARTESIAN_POINT('Ctrl Pts',(-14.4581074923707,3.02582179576277,4.43025020926697));
#86924=CARTESIAN_POINT('Ctrl Pts',(-14.4057359491156,3.01597163605999,4.42747746701779));
#86925=CARTESIAN_POINT('Ctrl Pts',(-14.3537053912016,3.00478044599569,4.42470472476861));
#86926=CARTESIAN_POINT('Ctrl Pts',(-14.259856853012,2.98459467689687,4.4197034751704));
#86927=CARTESIAN_POINT('Ctrl Pts',(-14.1667911929647,2.95997271228434,4.41470222557219));
#86928=CARTESIAN_POINT('Ctrl Pts',(-14.0749591752603,2.93098988783053,4.40970097597398));
#86929=CARTESIAN_POINT('Ctrl Pts',(-13.9832739652492,2.90205339690736,4.40470772164731));
#86930=CARTESIAN_POINT('Ctrl Pts',(-13.8928188892288,2.86877004520901,4.39971446732065));
#86931=CARTESIAN_POINT('Ctrl Pts',(-13.8040338573033,2.83126601285062,4.39472121299398));
#86932=CARTESIAN_POINT('Ctrl Pts',(-13.71533125354,2.79379679929444,4.38973259441242));
#86933=CARTESIAN_POINT('Ctrl Pts',(-13.6282960156907,2.75211485854518,4.38474397583087));
#86934=CARTESIAN_POINT('Ctrl Pts',(-13.5433517367207,2.70639577428827,4.37975535724932));
#86935=CARTESIAN_POINT('Ctrl Pts',(-13.4584655126854,2.66070793661422,4.37477014812546));
#86936=CARTESIAN_POINT('Ctrl Pts',(-13.3756677923777,2.61098864655695,4.36978493900161));
#86937=CARTESIAN_POINT('Ctrl Pts',(-13.2953600436244,2.55746062904744,4.36479972987776));
#86938=CARTESIAN_POINT('Ctrl Pts',(-13.2381613227809,2.51933561398523,4.36124904405418));
#86939=CARTESIAN_POINT('Ctrl Pts',(-13.1822253101393,2.47927946661832,4.35769835823061));
#86940=CARTESIAN_POINT('Ctrl Pts',(-13.1276888212995,2.43738653071546,4.35414767240703));
#86941=CARTESIAN_POINT('',(-18.0734992704458,0.00211768020265139,4.79157655282255));
#86942=CARTESIAN_POINT('Ctrl Pts',(-18.0702676004121,0.00213770170989528,
4.791575403523));
#86943=CARTESIAN_POINT('Ctrl Pts',(-18.0725846333099,0.362048543166639,
4.7729831523707));
#86944=CARTESIAN_POINT('Ctrl Pts',(-17.8482361699865,1.73885344748678,4.70171584497116));
#86945=CARTESIAN_POINT('Ctrl Pts',(-15.9143185581385,3.44829888129498,4.58366527076405));
#86946=CARTESIAN_POINT('Ctrl Pts',(-13.8440432611115,2.98320055308787,4.48420694770922));
#86947=CARTESIAN_POINT('Ctrl Pts',(-13.1255958151414,2.44015351965519,4.43742368090164));
#86948=CARTESIAN_POINT('Ctrl Pts',(-13.1276888212995,2.43738653071547,5.43736138633702));
#86949=CARTESIAN_POINT('Ctrl Pts',(-13.0510205330792,2.37849275606065,5.43236854431858));
#86950=CARTESIAN_POINT('Ctrl Pts',(-12.9771508045237,2.31599130424347,5.42737570230014));
#86951=CARTESIAN_POINT('Ctrl Pts',(-12.906424534798,2.25018755251741,5.4223828602817));
#86952=CARTESIAN_POINT('Ctrl Pts',(-12.8356222754107,2.1843130999775,5.41738465385797));
#86953=CARTESIAN_POINT('Ctrl Pts',(-12.7679705386501,2.11512956162114,5.41238644743423));
#86954=CARTESIAN_POINT('Ctrl Pts',(-12.7037777600287,2.04297960701055,5.4073882410105));
#86955=CARTESIAN_POINT('Ctrl Pts',(-12.6395477110153,1.97078776206371,5.40238713262309));
#86956=CARTESIAN_POINT('Ctrl Pts',(-12.5787808943321,1.89562641057895,5.39738602423567));
#86957=CARTESIAN_POINT('Ctrl Pts',(-12.5217444641205,1.81787011331464,5.39238491584826));
#86958=CARTESIAN_POINT('Ctrl Pts',(-12.4646153147323,1.73998741438342,5.3873756775928));
#86959=CARTESIAN_POINT('Ctrl Pts',(-12.4112289040444,1.65950170923796,5.38236643933734));
#86960=CARTESIAN_POINT('Ctrl Pts',(-12.3618081980268,1.57681522887158,5.37735720108188));
#86961=CARTESIAN_POINT('Ctrl Pts',(-12.3307046723726,1.5247754813533,5.37420457573227));
#86962=CARTESIAN_POINT('Ctrl Pts',(-12.3011710274356,1.4718645107532,5.37105195038266));
#86963=CARTESIAN_POINT('Ctrl Pts',(-12.2732531150491,1.41818675618217,5.36789932503305));
#86964=CARTESIAN_POINT('Ctrl Pts',(-12.229020765757,1.333141242874,5.36290439476317));
#86965=CARTESIAN_POINT('Ctrl Pts',(-12.1886920459263,1.24587254939232,5.3579094644933));
#86966=CARTESIAN_POINT('Ctrl Pts',(-12.1524966929214,1.15677446642659,5.35291453422342));
#86967=CARTESIAN_POINT('Ctrl Pts',(-12.1163508613921,1.06779828498065,5.34792643787826));
#86968=CARTESIAN_POINT('Ctrl Pts',(-12.0843273221457,0.97699809214518,5.3429383415331));
#86969=CARTESIAN_POINT('Ctrl Pts',(-12.0566099351616,0.884792165545563,
5.33795024518793));
#86970=CARTESIAN_POINT('Ctrl Pts',(-12.0289220695585,0.79268444612118,5.33296746159077));
#86971=CARTESIAN_POINT('Ctrl Pts',(-12.0055313651088,0.699174388146253,
5.3279846779936));
#86972=CARTESIAN_POINT('Ctrl Pts',(-11.9865731849166,0.604699164987345,
5.32300189439644));
#86973=CARTESIAN_POINT('Ctrl Pts',(-11.9676287900181,0.510292638754096,
5.31802273399171));
#86974=CARTESIAN_POINT('Ctrl Pts',(-11.9531105984872,0.41492277249696,5.31304357358699));
#86975=CARTESIAN_POINT('Ctrl Pts',(-11.9431035598391,0.319039815903618,
5.30806441318226));
#86976=CARTESIAN_POINT('Ctrl Pts',(-11.9331002282061,0.223192378265826,
5.30308709726151));
#86977=CARTESIAN_POINT('Ctrl Pts',(-11.9276047749072,0.126832664968066,
5.29810978134076));
#86978=CARTESIAN_POINT('Ctrl Pts',(-11.926650525246,0.0304180214548819,
5.29313246542001));
#86979=CARTESIAN_POINT('Ctrl Pts',(-11.9256963672343,-0.0659873620615559,
5.28815562753795));
#86980=CARTESIAN_POINT('Ctrl Pts',(-11.9292825499124,-0.162447225441892,
5.28317878965589));
#86981=CARTESIAN_POINT('Ctrl Pts',(-11.9373902825083,-0.258503323625889,
5.27820195177382));
#86982=CARTESIAN_POINT('Ctrl Pts',(-11.9454994611287,-0.354576553536986,
5.2732242262664));
#86983=CARTESIAN_POINT('Ctrl Pts',(-11.9581317540368,-0.450245436929502,
5.26824650075898));
#86984=CARTESIAN_POINT('Ctrl Pts',(-11.9752165244132,-0.545057039048925,
5.26326877525155));
#86985=CARTESIAN_POINT('Ctrl Pts',(-11.9923196282558,-0.639970382384078,
5.2582857082054));
#86986=CARTESIAN_POINT('Ctrl Pts',(-12.0138846697799,-0.734024174307596,
5.25330264115925));
#86987=CARTESIAN_POINT('Ctrl Pts',(-12.0397899523229,-0.826776102479868,
5.2483195741131));
#86988=CARTESIAN_POINT('Ctrl Pts',(-12.0657105249464,-0.919582775642581,
5.24333356591022));
#86989=CARTESIAN_POINT('Ctrl Pts',(-12.0959763010442,-1.01108563773112,
5.23834755770734));
#86990=CARTESIAN_POINT('Ctrl Pts',(-12.1304164882122,-1.10085999058721,
5.23336154950445));
#86991=CARTESIAN_POINT('Ctrl Pts',(-12.1649121265169,-1.19077888649965,
5.22836751347579));
#86992=CARTESIAN_POINT('Ctrl Pts',(-12.2035954191685,-1.2789633138907,5.22337347744712));
#86993=CARTESIAN_POINT('Ctrl Pts',(-12.2462485114045,-1.36501098495866,
5.21837944141845));
#86994=CARTESIAN_POINT('Ctrl Pts',(-12.2704625077885,-1.41385991681506,
5.21554434637608));
#86995=CARTESIAN_POINT('Ctrl Pts',(-12.2959550612654,-1.46202069568636,
5.2127092513337));
#86996=CARTESIAN_POINT('Ctrl Pts',(-12.3226801324512,-1.50942392217305,
5.20987415629133));
#86997=CARTESIAN_POINT('Ctrl Pts',(-12.3698321797499,-1.59305921585964,
5.20487209157818));
#86998=CARTESIAN_POINT('Ctrl Pts',(-12.4209889291442,-1.67462839778874,
5.19987002686503));
#86999=CARTESIAN_POINT('Ctrl Pts',(-12.4759444281291,-1.75372338756921,
5.19486796215188));
#87000=CARTESIAN_POINT('Ctrl Pts',(-12.5308257731993,-1.83271165093968,
5.18987264694854));
#87001=CARTESIAN_POINT('Ctrl Pts',(-12.5894954322247,-1.90923200048418,
5.1848773317452));
#87002=CARTESIAN_POINT('Ctrl Pts',(-12.6517019533244,-1.98290154419724,
5.17988201654187));
#87003=CARTESIAN_POINT('Ctrl Pts',(-12.7138432361192,-2.05649382790485,
5.17489194011239));
#87004=CARTESIAN_POINT('Ctrl Pts',(-12.7795137256188,-2.12724091618579,
5.16990186368291));
#87005=CARTESIAN_POINT('Ctrl Pts',(-12.8484197281198,-2.1947903279484,5.16491178725343));
#87006=CARTESIAN_POINT('Ctrl Pts',(-12.9172768052121,-2.26229177752404,
5.15992525393369));
#87007=CARTESIAN_POINT('Ctrl Pts',(-12.9893645160051,-2.32659975821772,
5.15493872061394));
#87008=CARTESIAN_POINT('Ctrl Pts',(-13.0643507490039,-2.38739695633515,
5.1499521872942));
#87009=CARTESIAN_POINT('Ctrl Pts',(-13.1393099497156,-2.44817223726517,
5.14496745160312));
#87010=CARTESIAN_POINT('Ctrl Pts',(-13.2171652562067,-2.50543897454987,
5.13998271591203));
#87011=CARTESIAN_POINT('Ctrl Pts',(-13.2975504868493,-2.55891928461466,
5.13499798022094));
#87012=CARTESIAN_POINT('Ctrl Pts',(-13.3779286184244,-2.61239487166843,
5.13001368474722));
#87013=CARTESIAN_POINT('Ctrl Pts',(-13.4608358647743,-2.66208445369521,
5.12502938927351));
#87014=CARTESIAN_POINT('Ctrl Pts',(-13.5458768866329,-2.70775335309025,
5.12004509379979));
#87015=CARTESIAN_POINT('Ctrl Pts',(-13.6309335446414,-2.7534306494418,5.11505988188375));
#87016=CARTESIAN_POINT('Ctrl Pts',(-13.7181243710789,-2.79508558755098,
5.11007466996771));
#87017=CARTESIAN_POINT('Ctrl Pts',(-13.8070302054619,-2.83252984438289,
5.10508945805167));
#87018=CARTESIAN_POINT('Ctrl Pts',(-13.8960312768007,-2.87001421193485,
5.10009890591909));
#87019=CARTESIAN_POINT('Ctrl Pts',(-13.9867506189721,-2.90327872310088,
5.09510835378651));
#87020=CARTESIAN_POINT('Ctrl Pts',(-14.0787501182962,-2.93218364115564,
5.09011780165394));
#87021=CARTESIAN_POINT('Ctrl Pts',(-14.170804026667,-2.96110565374948,5.08512429807938));
#87022=CARTESIAN_POINT('Ctrl Pts',(-14.2641391759466,-2.98566282778118,
5.08013079450483));
#87023=CARTESIAN_POINT('Ctrl Pts',(-14.3583054066296,-3.00576617501083,
5.07513729093028));
#87024=CARTESIAN_POINT('Ctrl Pts',(-14.4526219465686,-3.02590161144211,
5.07013581666601));
#87025=CARTESIAN_POINT('Ctrl Pts',(-14.5477717844515,-3.04156895477625,
5.06513434240174));
#87026=CARTESIAN_POINT('Ctrl Pts',(-14.6432978387497,-3.05273087876402,
5.06013286813747));
#87027=CARTESIAN_POINT('Ctrl Pts',(-14.696037383467,-3.05889333144365,5.05737157460817));
#87028=CARTESIAN_POINT('Ctrl Pts',(-14.7488915569139,-3.0636834119157,5.05461028107888));
#87029=CARTESIAN_POINT('Ctrl Pts',(-14.8017835631764,-3.0671016439259,5.05184898754958));
#87030=CARTESIAN_POINT('Ctrl Pts',(-14.8975915662202,-3.07329339209314,
5.04684721057884));
#87031=CARTESIAN_POINT('Ctrl Pts',(-14.9938563775379,-3.07500241943791,
5.04184543360811));
#87032=CARTESIAN_POINT('Ctrl Pts',(-15.0901237054268,-3.07217837498413,
5.03684365663737));
#87033=CARTESIAN_POINT('Ctrl Pts',(-15.1862614035205,-3.06935813327748,
5.03184861486266));
#87034=CARTESIAN_POINT('Ctrl Pts',(-15.2824011768329,-3.06201696431892,
5.02685357308795));
#87035=CARTESIAN_POINT('Ctrl Pts',(-15.3780849852503,-3.05015638843785,
5.02185853131324));
#87036=CARTESIAN_POINT('Ctrl Pts',(-15.4736687214783,-3.03830821709854,
5.01686871366971));
#87037=CARTESIAN_POINT('Ctrl Pts',(-15.568797007958,-3.02195008915829,5.01187889602618));
#87038=CARTESIAN_POINT('Ctrl Pts',(-15.6630142108175,-3.00113551947493,
5.00688907838265));
#87039=CARTESIAN_POINT('Ctrl Pts',(-15.7571649491824,-2.98033563320194,
5.00190278075136));
#87040=CARTESIAN_POINT('Ctrl Pts',(-15.8504054546709,-2.95508564923108,
4.99691648312007));
#87041=CARTESIAN_POINT('Ctrl Pts',(-15.9422885710765,-2.92549047149681,
4.99193018548879));
#87042=CARTESIAN_POINT('Ctrl Pts',(-16.0341388282225,-2.89590587759627,
4.98694567105831));
#87043=CARTESIAN_POINT('Ctrl Pts',(-16.1246322438638,-2.86197931184187,
4.98196115662784));
#87044=CARTESIAN_POINT('Ctrl Pts',(-16.2133360878607,-2.82386575245617,
4.97697664219736));
#87045=CARTESIAN_POINT('Ctrl Pts',(-16.3020323605703,-2.78575544624075,
4.97199255321847));
#87046=CARTESIAN_POINT('Ctrl Pts',(-16.3889389625577,-2.74345903026862,
4.96700846423958));
#87047=CARTESIAN_POINT('Ctrl Pts',(-16.4736434362022,-2.69717950328451,
4.96202437526069));
#87048=CARTESIAN_POINT('Ctrl Pts',(-16.5583637416606,-2.65089132635758,
4.95703935472334));
#87049=CARTESIAN_POINT('Ctrl Pts',(-16.6408807165536,-2.60061877010777,
4.95205433418599));
#87050=CARTESIAN_POINT('Ctrl Pts',(-16.7208077281701,-2.54661010220842,
4.94706931364865));
#87051=CARTESIAN_POINT('Ctrl Pts',(-16.8008207528596,-2.49254331313833,
4.94207892850519));
#87052=CARTESIAN_POINT('Ctrl Pts',(-16.8782378861775,-2.43473263176821,
4.93708854336173));
#87053=CARTESIAN_POINT('Ctrl Pts',(-16.952702846875,-2.37346873621838,4.93209815821828));
#87054=CARTESIAN_POINT('Ctrl Pts',(-17.0272120506079,-2.31216844098918,
4.927104808059));
#87055=CARTESIAN_POINT('Ctrl Pts',(-17.0987652641845,-2.24741114029537,
4.92211145789973));
#87056=CARTESIAN_POINT('Ctrl Pts',(-17.1670421439888,-2.17952531441518,
4.91711810774046));
#87057=CARTESIAN_POINT('Ctrl Pts',(-17.2354283256271,-2.11153081272407,
4.91211676391873));
#87058=CARTESIAN_POINT('Ctrl Pts',(-17.3005274050842,-2.04039810889525,
4.907115420097));
#87059=CARTESIAN_POINT('Ctrl Pts',(-17.3620585382765,-1.96648969276608,
4.90211407627527));
#87060=CARTESIAN_POINT('Ctrl Pts',(-17.3960566632211,-1.92565268171733,
4.89935065711946));
#87061=CARTESIAN_POINT('Ctrl Pts',(-17.4289662609585,-1.88396880226838,
4.89658723796366));
#87062=CARTESIAN_POINT('Ctrl Pts',(-17.4607457414077,-1.84150282273583,
4.89382381880785));
#87063=CARTESIAN_POINT('Ctrl Pts',(-17.5184291891083,-1.76442213813061,
4.88880789211252));
#87064=CARTESIAN_POINT('Ctrl Pts',(-17.5725898992664,-1.68449167440274,
4.88379196541719));
#87065=CARTESIAN_POINT('Ctrl Pts',(-17.6229351526086,-1.60206536546108,
4.87877603872186));
#87066=CARTESIAN_POINT('Ctrl Pts',(-17.6732122760822,-1.51975060017493,
4.87376689984472));
#87067=CARTESIAN_POINT('Ctrl Pts',(-17.7196839777768,-1.43494706825674,
4.86875776096759));
#87068=CARTESIAN_POINT('Ctrl Pts',(-17.762098714886,-1.34804040711883,4.86374862209045));
#87069=CARTESIAN_POINT('Ctrl Pts',(-17.8044673660001,-1.26122817495158,
4.85874492592417));
#87070=CARTESIAN_POINT('Ctrl Pts',(-17.8427876244817,-1.17231774389179,
4.85374122975788));
#87071=CARTESIAN_POINT('Ctrl Pts',(-17.8768526283568,-1.08172140808836,
4.8487375335916));
#87072=CARTESIAN_POINT('Ctrl Pts',(-17.9108890317255,-0.991201135716088,
4.84373803845945));
#87073=CARTESIAN_POINT('Ctrl Pts',(-17.9406771326098,-0.898998178990735,
4.8387385433273));
#87074=CARTESIAN_POINT('Ctrl Pts',(-17.9660576270989,-0.805546027690952,
4.83373904819515));
#87075=CARTESIAN_POINT('Ctrl Pts',(-17.991425186168,-0.712141505203933,
4.82874210110512));
#87076=CARTESIAN_POINT('Ctrl Pts',(-18.012389492138,-0.617489473104872,
4.82374515401509));
#87077=CARTESIAN_POINT('Ctrl Pts',(-18.0288409625587,-0.522038957862991,
4.81874820692505));
#87078=CARTESIAN_POINT('Ctrl Pts',(-18.0452922989824,-0.426589220063481,
4.81375130053505));
#87079=CARTESIAN_POINT('Ctrl Pts',(-18.0572307877008,-0.330341438581802,
4.80875439414504));
#87080=CARTESIAN_POINT('Ctrl Pts',(-18.0645980267115,-0.233754539369315,
4.80375748775503));
#87081=CARTESIAN_POINT('Ctrl Pts',(-18.070584387873,-0.155271397813929,
4.79969717611087));
#87082=CARTESIAN_POINT('Ctrl Pts',(-18.0735534835641,-0.0765646343269345,
4.79563686446671));
#87083=CARTESIAN_POINT('Ctrl Pts',(-18.0734992704458,0.00211768020265139,
4.79157655282255));
#87084=CARTESIAN_POINT('Origin',(15.,0.,8.20842344717745));
#87085=CARTESIAN_POINT('',(11.9265011624444,-0.00267311509943158,4.70842344717746));
#87086=CARTESIAN_POINT('Ctrl Pts',(16.8743174193178,2.43995797974749,5.35407234097178));
#87087=CARTESIAN_POINT('Ctrl Pts',(17.5785721639147,1.88987785061309,5.30765841680695));
#87088=CARTESIAN_POINT('Ctrl Pts',(18.5637879643976,0.0231525210448785,
5.20856943639487));
#87089=CARTESIAN_POINT('Ctrl Pts',(17.1019761085213,-2.95589625912284,5.05680539973555));
#87090=CARTESIAN_POINT('Ctrl Pts',(13.6723626328074,-3.37529520198335,4.8987802309938));
#87091=CARTESIAN_POINT('Ctrl Pts',(12.0374225320172,-1.43265805207317,4.78265291347445));
#87092=CARTESIAN_POINT('Ctrl Pts',(11.9237310852615,-0.210587998618168,
4.71920065220233));
#87093=CARTESIAN_POINT('Ctrl Pts',(11.9256181828774,-0.00267388305352438,
4.70842344717746));
#87094=CARTESIAN_POINT('Ctrl Pts',(11.9265011624444,-0.00267311509943158,
4.70842344717746));
#87095=CARTESIAN_POINT('Ctrl Pts',(11.9264186179886,0.0922349900664025,
4.70350244021915));
#87096=CARTESIAN_POINT('Ctrl Pts',(11.9307363572755,0.187280846398732,4.69858143326084));
#87097=CARTESIAN_POINT('Ctrl Pts',(11.9394659657117,0.282017153668012,4.69366042630253));
#87098=CARTESIAN_POINT('Ctrl Pts',(11.9481876941353,0.37666794469639,4.6887438614217));
#87099=CARTESIAN_POINT('Ctrl Pts',(11.9613133367653,0.471009293387588,4.68382729654086));
#87100=CARTESIAN_POINT('Ctrl Pts',(11.9788024226627,0.564594942140883,4.67891073166003));
#87101=CARTESIAN_POINT('Ctrl Pts',(11.9962832475833,0.658136385675146,4.6739964891206));
#87102=CARTESIAN_POINT('Ctrl Pts',(12.0181233410234,0.750922394056947,4.66908224658118));
#87103=CARTESIAN_POINT('Ctrl Pts',(12.0442306381959,0.842513934496294,4.66416800404175));
#87104=CARTESIAN_POINT('Ctrl Pts',(12.0703332027249,0.934088871527253,4.65925465233979));
#87105=CARTESIAN_POINT('Ctrl Pts',(12.1007013101754,1.02446933585973,4.65434130063783));
#87106=CARTESIAN_POINT('Ctrl Pts',(12.1351925544778,1.11322978314479,4.64942794893587));
#87107=CARTESIAN_POINT('Ctrl Pts',(12.1696875859408,1.20199997638338,4.64451405774477));
#87108=CARTESIAN_POINT('Ctrl Pts',(12.2083064876828,1.28914937836292,4.63960016655367));
#87109=CARTESIAN_POINT('Ctrl Pts',(12.2508585435057,1.37427198988562,4.63468627536257));
#87110=CARTESIAN_POINT('Ctrl Pts',(12.2934533242757,1.4594800698779,4.62976745031486));
#87111=CARTESIAN_POINT('Ctrl Pts',(12.3399889383471,1.54265689260553,4.62484862526715));
#87112=CARTESIAN_POINT('Ctrl Pts',(12.3902286954731,1.62342107540458,4.61992980021943));
#87113=CARTESIAN_POINT('Ctrl Pts',(12.440496549854,1.70423042665118,4.61500822425314));
#87114=CARTESIAN_POINT('Ctrl Pts',(12.4944724121225,1.78262408153428,4.61008664828685));
#87115=CARTESIAN_POINT('Ctrl Pts',(12.551877550136,1.85825152239187,4.60516507232055));
#87116=CARTESIAN_POINT('Ctrl Pts',(12.6093728827216,1.93399778858301,4.60023576360674));
#87117=CARTESIAN_POINT('Ctrl Pts',(12.6703079543828,2.00696882062901,4.59530645489292));
#87118=CARTESIAN_POINT('Ctrl Pts',(12.7343654610338,2.07684914855259,4.59037714617911));
#87119=CARTESIAN_POINT('Ctrl Pts',(12.7674913999929,2.11298623221784,4.58782806195618));
#87120=CARTESIAN_POINT('Ctrl Pts',(12.8014517667167,2.14829742447959,4.58527897773326));
#87121=CARTESIAN_POINT('Ctrl Pts',(12.836199237003,2.18274334452163,4.58272989351033));
#87122=CARTESIAN_POINT('Ctrl Pts',(12.9043684592838,2.25032097134355,4.57772898013236));
#87123=CARTESIAN_POINT('Ctrl Pts',(12.9758253945357,2.31481992588043,4.5727280667544));
#87124=CARTESIAN_POINT('Ctrl Pts',(13.0502607687252,2.37590386590618,4.56772715337643));
#87125=CARTESIAN_POINT('Ctrl Pts',(13.1245956188818,2.43690531284224,4.56273299366883));
#87126=CARTESIAN_POINT('Ctrl Pts',(13.2019005774341,2.49450063544591,4.55773883396123));
#87127=CARTESIAN_POINT('Ctrl Pts',(13.2818294598922,2.5483901281212,4.55274467425363));
#87128=CARTESIAN_POINT('Ctrl Pts',(13.3616744585565,2.60222306483138,4.54775575581865));
#87129=CARTESIAN_POINT('Ctrl Pts',(13.4441375449011,2.65235765932386,4.54276683738367));
#87130=CARTESIAN_POINT('Ctrl Pts',(13.528840184076,2.69853498143165,4.53777791894869));
#87131=CARTESIAN_POINT('Ctrl Pts',(13.6134826887818,2.74467952004211,4.53279254238636));
#87132=CARTESIAN_POINT('Ctrl Pts',(13.7003612014318,2.78687216204757,4.52780716582402));
#87133=CARTESIAN_POINT('Ctrl Pts',(13.7890698148569,2.82489828785204,4.52282178926169));
#87134=CARTESIAN_POINT('Ctrl Pts',(13.8777464637431,2.86291071163217,4.51783820908933));
#87135=CARTESIAN_POINT('Ctrl Pts',(13.9682515003463,2.89675942961718,4.51285462891697));
#87136=CARTESIAN_POINT('Ctrl Pts',(14.0601569936535,2.9262770500111,4.50787104874461));
#87137=CARTESIAN_POINT('Ctrl Pts',(14.1520544185593,2.95579207904727,4.50288790608174));
#87138=CARTESIAN_POINT('Ctrl Pts',(14.2453516380043,2.98097663254759,4.49790476341887));
#87139=CARTESIAN_POINT('Ctrl Pts',(14.3396044562356,3.0017128403257,4.492921620756));
#87140=CARTESIAN_POINT('Ctrl Pts',(14.4338746874182,3.02245287906166,4.48793755747111));
#87141=CARTESIAN_POINT('Ctrl Pts',(14.5291004395952,3.03874284569756,4.48295349418622));
#87142=CARTESIAN_POINT('Ctrl Pts',(14.6248272483537,3.05051596560683,4.47796943090132));
#87143=CARTESIAN_POINT('Ctrl Pts',(14.720656882956,3.06230173172257,4.47298001393841));
#87144=CARTESIAN_POINT('Ctrl Pts',(14.8169882125238,3.06956091152766,4.46799059697549));
#87145=CARTESIAN_POINT('Ctrl Pts',(14.9133617973856,3.0722786448901,4.46300118001257));
#87146=CARTESIAN_POINT('Ctrl Pts',(15.0097925065817,3.07499798915774,4.45800880563012));
#87147=CARTESIAN_POINT('Ctrl Pts',(15.1062650825882,3.07317053524227,4.45301643124767));
#87148=CARTESIAN_POINT('Ctrl Pts',(15.2023223512108,3.06683353252187,4.44802405686522));
#87149=CARTESIAN_POINT('Ctrl Pts',(15.2985333769842,3.06048638627462,4.44302369127844));
#87150=CARTESIAN_POINT('Ctrl Pts',(15.3943273325049,3.04961532775035,4.43802332569166));
#87151=CARTESIAN_POINT('Ctrl Pts',(15.4892544874145,3.03430919593649,4.43302296010487));
#87152=CARTESIAN_POINT('Ctrl Pts',(15.5418923996255,3.0258218160769,4.43025021499278));
#87153=CARTESIAN_POINT('Ctrl Pts',(15.5942639972722,3.01597164759197,4.42747746988069));
#87154=CARTESIAN_POINT('Ctrl Pts',(15.6462946088311,3.00478044598868,4.4247047247686));
#87155=CARTESIAN_POINT('Ctrl Pts',(15.7401431465919,2.98459467698101,4.41970347518578));
#87156=CARTESIAN_POINT('Ctrl Pts',(15.833208806245,2.95997271249419,4.41470222560295));
#87157=CARTESIAN_POINT('Ctrl Pts',(15.9250408235919,2.93098988819278,4.40970097602012));
#87158=CARTESIAN_POINT('Ctrl Pts',(16.0167260332122,2.90205339743246,4.40470772171066));
#87159=CARTESIAN_POINT('Ctrl Pts',(16.107181108879,2.86877004592674,4.39971446740119));
#87160=CARTESIAN_POINT('Ctrl Pts',(16.1959661404893,2.83126601378307,4.39472121309172));
#87161=CARTESIAN_POINT('Ctrl Pts',(16.2846687439218,2.79379680044808,4.38973259452824));
#87162=CARTESIAN_POINT('Ctrl Pts',(16.3717039814793,2.75211485994354,4.38474397596476));
#87163=CARTESIAN_POINT('Ctrl Pts',(16.4566482601966,2.70639577594747,4.37975535740128));
#87164=CARTESIAN_POINT('Ctrl Pts',(16.541534483932,2.66070793855956,4.37477014829827));
#87165=CARTESIAN_POINT('Ctrl Pts',(16.6243322039809,2.61098864880902,4.36978493919526));
#87166=CARTESIAN_POINT('Ctrl Pts',(16.7046399525167,2.55746063161955,4.36479973009225));
#87167=CARTESIAN_POINT('Ctrl Pts',(16.7618385480427,2.51933570021064,4.36124905205315));
#87168=CARTESIAN_POINT('Ctrl Pts',(16.8177744409165,2.47927964495925,4.35769837401405));
#87169=CARTESIAN_POINT('Ctrl Pts',(16.8723108164276,2.43738680900022,4.35414769597494));
#87170=CARTESIAN_POINT('',(11.9265007295358,0.00211765345701963,4.79157655282255));
#87171=CARTESIAN_POINT('Ctrl Pts',(11.9297330560105,0.002137679106189,4.791575403287));
#87172=CARTESIAN_POINT('Ctrl Pts',(11.9274160148606,0.362048478990828,4.77298315221337));
#87173=CARTESIAN_POINT('Ctrl Pts',(12.151764398138,1.73885322680167,4.70171584489249));
#87174=CARTESIAN_POINT('Ctrl Pts',(14.0856815469411,3.44829792336913,4.58366527839654));
#87175=CARTESIAN_POINT('Ctrl Pts',(16.1559561762778,2.98319997967846,4.48420696297422));
#87176=CARTESIAN_POINT('Ctrl Pts',(16.8744034286678,2.4401532777456,4.43742370379915));
#87177=CARTESIAN_POINT('Ctrl Pts',(16.8723108164276,2.43738680900022,5.43736140735745));
#87178=CARTESIAN_POINT('Ctrl Pts',(16.9489792105581,2.37849297110846,5.4323685573755));
#87179=CARTESIAN_POINT('Ctrl Pts',(17.0228490367164,2.31599144785443,5.42737570739354));
#87180=CARTESIAN_POINT('Ctrl Pts',(17.0935753952956,2.25018761755837,5.42238285741159));
#87181=CARTESIAN_POINT('Ctrl Pts',(17.1643777456509,2.18431308448554,5.41738464287325));
#87182=CARTESIAN_POINT('Ctrl Pts',(17.2320295644332,2.11512945825866,5.41238642833491));
#87183=CARTESIAN_POINT('Ctrl Pts',(17.2962224157258,2.04297940946999,5.40738821379658));
#87184=CARTESIAN_POINT('Ctrl Pts',(17.3604525385292,1.97078746908027,5.40238709720602));
#87185=CARTESIAN_POINT('Ctrl Pts',(17.4212194195263,1.89562601573753,5.39738598061546));
#87186=CARTESIAN_POINT('Ctrl Pts',(17.4782559042015,1.81786961119069,5.3923848640249));
#87187=CARTESIAN_POINT('Ctrl Pts',(17.53538510908,1.73998680352338,5.38737561747068));
#87188=CARTESIAN_POINT('Ctrl Pts',(17.588771565254,1.65950098411322,5.38236637091647));
#87189=CARTESIAN_POINT('Ctrl Pts',(17.6381923063921,1.57681438492086,5.37735712436226));
#87190=CARTESIAN_POINT('Ctrl Pts',(17.6692955503182,1.52477507096333,5.37420452458586));
#87191=CARTESIAN_POINT('Ctrl Pts',(17.6988289401045,1.47186454914168,5.37105192480945));
#87192=CARTESIAN_POINT('Ctrl Pts',(17.7267466251365,1.41818725572712,5.36789932503305));
#87193=CARTESIAN_POINT('Ctrl Pts',(17.7709788012614,1.33314211342738,5.3629044141584));
#87194=CARTESIAN_POINT('Ctrl Pts',(17.8113073878468,1.24587379722512,5.35790950328374));
#87195=CARTESIAN_POINT('Ctrl Pts',(17.8475026461821,1.15677609328071,5.35291459240909));
#87196=CARTESIAN_POINT('Ctrl Pts',(17.88364838107,1.06780029551037,5.34792651572261));
#87197=CARTESIAN_POINT('Ctrl Pts',(17.9156718626184,0.977000488300628,5.34293843903613));
#87198=CARTESIAN_POINT('Ctrl Pts',(17.9433892292822,0.884794945140182,5.33795036234965));
#87199=CARTESIAN_POINT('Ctrl Pts',(17.9710770731585,0.792687613497772,5.33296759864726));
#87200=CARTESIAN_POINT('Ctrl Pts',(17.9944677936174,0.699177941269497,5.32798483494486));
#87201=CARTESIAN_POINT('Ctrl Pts',(18.0134260258391,0.604703098053697,5.32300207124247));
#87202=CARTESIAN_POINT('Ctrl Pts',(18.0323704716355,0.510296956937685,5.31802293100551));
#87203=CARTESIAN_POINT('Ctrl Pts',(18.0468887505391,0.414927470116671,5.31304379076856));
#87204=CARTESIAN_POINT('Ctrl Pts',(18.0568959112316,0.319044883826335,5.3080646505316));
#87205=CARTESIAN_POINT('Ctrl Pts',(18.0668993645224,0.223197819625414,5.30308735494101));
#87206=CARTESIAN_POINT('Ctrl Pts',(18.0723949744294,0.126838470676509,5.29811005935043));
#87207=CARTESIAN_POINT('Ctrl Pts',(18.0733494138018,0.0304241792676716,
5.29313276375984));
#87208=CARTESIAN_POINT('Ctrl Pts',(18.0743037614796,-0.06598084944974,5.28815594634684));
#87209=CARTESIAN_POINT('Ctrl Pts',(18.0707178018187,-0.162440370266277,
5.28317912893384));
#87210=CARTESIAN_POINT('Ctrl Pts',(18.0626103237388,-0.258496141032276,
5.27820231152084));
#87211=CARTESIAN_POINT('Ctrl Pts',(18.0545013998621,-0.354569041308425,
5.27322460659797));
#87212=CARTESIAN_POINT('Ctrl Pts',(18.0418693934093,-0.450237610231264,
5.2682469016751));
#87213=CARTESIAN_POINT('Ctrl Pts',(18.0247849393674,-0.545048915764779,
5.26326919675224));
#87214=CARTESIAN_POINT('Ctrl Pts',(18.0076821523099,-0.639961961578314,
5.25828615034515));
#87215=CARTESIAN_POINT('Ctrl Pts',(17.9861174575717,-0.734015473909388,
5.25330310393805));
#87216=CARTESIAN_POINT('Ctrl Pts',(17.9602125500155,-0.826767142991621,
5.24832005753096));
#87217=CARTESIAN_POINT('Ctrl Pts',(17.9342923528586,-0.919573555986063,
5.24333407002904));
#87218=CARTESIAN_POINT('Ctrl Pts',(17.9040269805487,-1.01107617845491,5.23834808252711));
#87219=CARTESIAN_POINT('Ctrl Pts',(17.8695872237241,-1.10085031472934,5.23336209502518));
#87220=CARTESIAN_POINT('Ctrl Pts',(17.8350920155099,-1.1907689961763,5.2283680795939));
#87221=CARTESIAN_POINT('Ctrl Pts',(17.7964091793615,-1.27895323211523,5.22337406416262));
#87222=CARTESIAN_POINT('Ctrl Pts',(17.753756568313,-1.36500073716947,5.21838004873134));
#87223=CARTESIAN_POINT('Ctrl Pts',(17.7295410162616,-1.41385326427879,5.21554475125133));
#87224=CARTESIAN_POINT('Ctrl Pts',(17.7040467218771,-1.46201754260581,5.21270945377133));
#87225=CARTESIAN_POINT('Ctrl Pts',(17.6773197348229,-1.50942415759379,5.20987415629132));
#87226=CARTESIAN_POINT('Ctrl Pts',(17.6301675940733,-1.59305959984705,5.20487208308445));
#87227=CARTESIAN_POINT('Ctrl Pts',(17.5790107393177,-1.67462891798103,5.19987000987758));
#87228=CARTESIAN_POINT('Ctrl Pts',(17.5240551248562,-1.75372403093742,5.19486793667072));
#87229=CARTESIAN_POINT('Ctrl Pts',(17.46917366344,-1.83271241879279,5.18987261289182));
#87230=CARTESIAN_POINT('Ctrl Pts',(17.4105038778397,-1.90923287973844,5.18487728911293));
#87231=CARTESIAN_POINT('Ctrl Pts',(17.3482972216521,-1.98290252125038,5.17988196533404));
#87232=CARTESIAN_POINT('Ctrl Pts',(17.2861558029351,-2.05649490381021,5.17489188025963));
#87233=CARTESIAN_POINT('Ctrl Pts',(17.2204851689074,-2.12724207728245,5.16990179518521));
#87234=CARTESIAN_POINT('Ctrl Pts',(17.1515790149052,-2.19479156017599,5.16491171011079));
#87235=CARTESIAN_POINT('Ctrl Pts',(17.0827217854077,-2.26229308182359,5.15992516807901));
#87236=CARTESIAN_POINT('Ctrl Pts',(17.0106339151512,-2.32660112045707,5.15493862604722));
#87237=CARTESIAN_POINT('Ctrl Pts',(16.9356475171831,-2.38739836207175,5.14995208401543));
#87238=CARTESIAN_POINT('Ctrl Pts',(16.860688150942,-2.44817368698582,5.14496733957423));
#87239=CARTESIAN_POINT('Ctrl Pts',(16.7828326733712,-2.50544045376631,5.13998259513302));
#87240=CARTESIAN_POINT('Ctrl Pts',(16.7024472675756,-2.55892077859485,5.13499785069181));
#87241=CARTESIAN_POINT('Ctrl Pts',(16.6220689604118,-2.61239638071116,5.13001354644078));
#87242=CARTESIAN_POINT('Ctrl Pts',(16.5391615343711,-2.66208596303015,5.12502924218975));
#87243=CARTESIAN_POINT('Ctrl Pts',(16.4541203301321,-2.70775484774686,5.12004493793871));
#87244=CARTESIAN_POINT('Ctrl Pts',(16.3690634894584,-2.75343212955223,5.11505971722903));
#87245=CARTESIAN_POINT('Ctrl Pts',(16.2818724776512,-2.79508703811668,5.11007449651934));
#87246=CARTESIAN_POINT('Ctrl Pts',(16.1929664565577,-2.83253125022976,5.10508927580965));
#87247=CARTESIAN_POINT('Ctrl Pts',(16.1039651989865,-2.87001557272939,5.10009871491203));
#87248=CARTESIAN_POINT('Ctrl Pts',(16.0132456692638,-2.90328002370169,5.0951081540144));
#87249=CARTESIAN_POINT('Ctrl Pts',(15.9212459823961,-2.93218486625912,5.09011759311678));
#87250=CARTESIAN_POINT('Ctrl Pts',(15.8291918865314,-2.96110680326053,5.08512408078071));
#87251=CARTESIAN_POINT('Ctrl Pts',(15.7358565497685,-2.98566388639374,5.08013056844464));
#87252=CARTESIAN_POINT('Ctrl Pts',(15.6416901329319,-3.00576712725685,5.07513705610856));
#87253=CARTESIAN_POINT('Ctrl Pts',(15.5473734085243,-3.02590245672863,5.0701355731739));
#87254=CARTESIAN_POINT('Ctrl Pts',(15.45222338754,-3.0415696777737,5.06513409023924));
#87255=CARTESIAN_POINT('Ctrl Pts',(15.3566971528226,-3.05273146397914,5.06013260730458));
#87256=CARTESIAN_POINT('Ctrl Pts',(15.3039592605239,-3.05889363587365,5.05737140071958));
#87257=CARTESIAN_POINT('Ctrl Pts',(15.2511067479274,-3.06368352204467,5.05461019413458));
#87258=CARTESIAN_POINT('Ctrl Pts',(15.1982164035266,-3.06710164607777,5.05184898754958));
#87259=CARTESIAN_POINT('Ctrl Pts',(15.1024083595404,-3.07329339584653,5.04684720877601));
#87260=CARTESIAN_POINT('Ctrl Pts',(15.006143508681,-3.07500242085317,5.04184543000244));
#87261=CARTESIAN_POINT('Ctrl Pts',(14.9098761430184,-3.0721783705382,5.03684365122887));
#87262=CARTESIAN_POINT('Ctrl Pts',(14.8137384062145,-3.06935812294928,5.03184860760245));
#87263=CARTESIAN_POINT('Ctrl Pts',(14.7175985959546,-3.06201694450271,5.02685356397604));
#87264=CARTESIAN_POINT('Ctrl Pts',(14.6219147526597,-3.05015635595024,5.02185852034962));
#87265=CARTESIAN_POINT('Ctrl Pts',(14.52633098067,-3.03830817183864,5.01686870080825));
#87266=CARTESIAN_POINT('Ctrl Pts',(14.4312026605024,-3.02195002786311,5.01187888126688));
#87267=CARTESIAN_POINT('Ctrl Pts',(14.3369854262807,-3.00113543930223,5.00688906172551));
#87268=CARTESIAN_POINT('Ctrl Pts',(14.2428346553922,-2.98033553390359,5.00190276213505));
#87269=CARTESIAN_POINT('Ctrl Pts',(14.1495941197248,-2.95508552785747,4.99691646254458));
#87270=CARTESIAN_POINT('Ctrl Pts',(14.0577109756917,-2.92549032551266,4.99193016295412));
#87271=CARTESIAN_POINT('Ctrl Pts',(13.9658606902278,-2.89590570678482,4.98694564652717));
#87272=CARTESIAN_POINT('Ctrl Pts',(13.8753672488383,-2.86197911360387,4.98196113010021));
#87273=CARTESIAN_POINT('Ctrl Pts',(13.7866633818244,-2.82386552459466,4.97697661367326));
#87274=CARTESIAN_POINT('Ctrl Pts',(13.697967085474,-2.78575518848935,4.9719925226629));
#87275=CARTESIAN_POINT('Ctrl Pts',(13.6110604626015,-2.74345874037196,4.96700843165253));
#87276=CARTESIAN_POINT('Ctrl Pts',(13.5263559709507,-2.69717917937375,4.96202434064216));
#87277=CARTESIAN_POINT('Ctrl Pts',(13.4416356469328,-2.65089096812596,4.95703931804061));
#87278=CARTESIAN_POINT('Ctrl Pts',(13.3591186563884,-2.60061837563425,4.95205429543906));
#87279=CARTESIAN_POINT('Ctrl Pts',(13.2791916321199,-2.54660966994035,4.94706927283751));
#87280=CARTESIAN_POINT('Ctrl Pts',(13.1991785941939,-2.49254284264924,4.94207888559201));
#87281=CARTESIAN_POINT('Ctrl Pts',(13.1217614506819,-2.43473212144877,4.93708849834652));
#87282=CARTESIAN_POINT('Ctrl Pts',(13.0472964829005,-2.37346818481038,4.93209811110102));
#87283=CARTESIAN_POINT('Ctrl Pts',(12.9727872717327,-2.31216784818284,4.92710475881522));
#87284=CARTESIAN_POINT('Ctrl Pts',(12.9012340538619,-2.24741050479877,4.92211140652942));
#87285=CARTESIAN_POINT('Ctrl Pts',(12.8329571729522,-2.17952463526812,4.91711805424361));
#87286=CARTESIAN_POINT('Ctrl Pts',(12.7645709900054,-2.11153008965672,4.91211670827724));
#87287=CARTESIAN_POINT('Ctrl Pts',(12.6994719124577,-2.04039734092574,4.90711536231086));
#87288=CARTESIAN_POINT('Ctrl Pts',(12.6379407844251,-1.96648887922559,4.90211401634449));
#87289=CARTESIAN_POINT('Ctrl Pts',(12.6039429226847,-1.92565215572201,4.89935061716561));
#87290=CARTESIAN_POINT('Ctrl Pts',(12.5710335724665,-1.883968576587,4.89658721798673));
#87291=CARTESIAN_POINT('Ctrl Pts',(12.5392543229165,-1.84150290869026,4.89382381880785));
#87292=CARTESIAN_POINT('Ctrl Pts',(12.4815709191545,-1.76442228841168,4.88880789574964));
#87293=CARTESIAN_POINT('Ctrl Pts',(12.4274102455408,-1.68449189134849,4.88379197269143));
#87294=CARTESIAN_POINT('Ctrl Pts',(12.3770650214843,-1.60206565048959,4.87877604963322));
#87295=CARTESIAN_POINT('Ctrl Pts',(12.3267879278441,-1.51975095415582,4.87376691444681));
#87296=CARTESIAN_POINT('Ctrl Pts',(12.2803162486563,-1.43494749266234,4.8687577792604));
#87297=CARTESIAN_POINT('Ctrl Pts',(12.2379015269199,-1.34804090257257,4.86374864407399));
#87298=CARTESIAN_POINT('Ctrl Pts',(12.1955328916047,-1.26122874228337,4.85874495164671));
#87299=CARTESIAN_POINT('Ctrl Pts',(12.1572126417202,-1.1723183837677,4.85374125921942));
#87300=CARTESIAN_POINT('Ctrl Pts',(12.1231476394767,-1.08172212039477,4.84873756679214));
#87301=CARTESIAN_POINT('Ctrl Pts',(12.0891112381515,-0.991201921491761,
4.84373807545658));
#87302=CARTESIAN_POINT('Ctrl Pts',(12.0593231322546,-0.898999038163477,
4.83873858412102));
#87303=CARTESIAN_POINT('Ctrl Pts',(12.0339426259614,-0.805546959469903,
4.83373909278546));
#87304=CARTESIAN_POINT('Ctrl Pts',(12.0085750552694,-0.7121425101975,4.82874214952462));
#87305=CARTESIAN_POINT('Ctrl Pts',(11.9876107308319,-0.617490550540763,
4.82374520626377));
#87306=CARTESIAN_POINT('Ctrl Pts',(11.9711592353833,-0.522040106309965,
4.81874826300292));
#87307=CARTESIAN_POINT('Ctrl Pts',(11.9547078740308,-0.426590440095431,
4.81375136047214));
#87308=CARTESIAN_POINT('Ctrl Pts',(11.9427693537697,-0.330342728777753,
4.80875445794136));
#87309=CARTESIAN_POINT('Ctrl Pts',(11.9354020768965,-0.233755897700299,
4.80375755541058));
#87310=CARTESIAN_POINT('Ctrl Pts',(11.9294156470961,-0.155272314982306,
4.79969722121457));
#87311=CARTESIAN_POINT('Ctrl Pts',(11.9264465167955,-0.0765651061646668,
4.79563688701856));
#87312=CARTESIAN_POINT('Ctrl Pts',(11.9265007295358,0.00211765345701963,
4.79157655282255));
#87313=CARTESIAN_POINT('Ctrl Pts',(16.9092545419647,1.63408129378416,5.99751862268169));
#87314=CARTESIAN_POINT('Ctrl Pts',(17.4503910847081,1.00187072518604,5.94481637259664));
#87315=CARTESIAN_POINT('Ctrl Pts',(17.846030394839,-0.831019091968321,5.83943906626436));
#87316=CARTESIAN_POINT('Ctrl Pts',(15.854778737488,-2.84170029323275,5.68138670368482));
#87317=CARTESIAN_POINT('Ctrl Pts',(13.0882748849575,-2.26629684041423,5.52336153494307));
#87318=CARTESIAN_POINT('Ctrl Pts',(12.0566111632693,0.362281029851998,5.36533636620135));
#87319=CARTESIAN_POINT('Ctrl Pts',(13.6960010987147,2.66384541131324,5.20731119745959));
#87320=CARTESIAN_POINT('Ctrl Pts',(16.5187402906678,2.54713911068689,5.04928602871788));
#87321=CARTESIAN_POINT('Ctrl Pts',(17.963258105202,0.119422738630435,4.89126085997614));
#87322=CARTESIAN_POINT('Ctrl Pts',(16.7186900320778,-2.41690160788,4.7332356912344));
#87323=CARTESIAN_POINT('Ctrl Pts',(13.9144514535833,-2.75982500250668,4.57521052249267));
#87324=CARTESIAN_POINT('Ctrl Pts',(12.0953224532673,-0.598334453229223,
4.41718535375093));
#87325=CARTESIAN_POINT('Ctrl Pts',(12.9121191859219,2.10616193894731,4.2591601850092));
#87326=CARTESIAN_POINT('Ctrl Pts',(15.6236181183402,2.89935030149973,4.10113501626745));
#87327=CARTESIAN_POINT('Ctrl Pts',(17.7691984294259,1.061455514847,3.94310984752573));
#87328=CARTESIAN_POINT('Ctrl Pts',(17.4017970424563,-1.73968914675123,3.78508467878397));
#87329=CARTESIAN_POINT('Ctrl Pts',(14.8548219664639,-2.96210511531461,3.62705951004225));
#87330=CARTESIAN_POINT('Ctrl Pts',(12.4395925050909,-1.49648226314551,3.46903434130051));
#87331=CARTESIAN_POINT('Ctrl Pts',(12.3478719394043,1.32716321501271,3.31100917255878));
#87332=CARTESIAN_POINT('Ctrl Pts',(14.662894506894,2.94643935627629,3.15298400381705));
#87333=CARTESIAN_POINT('Ctrl Pts',(17.283832284677,1.89189200897181,2.99495883507531));
#87334=CARTESIAN_POINT('Ctrl Pts',(17.8322466004053,-0.879502394853007,
2.83693366633358));
#87335=CARTESIAN_POINT('Ctrl Pts',(15.8104644735628,-2.85276928882038,2.67890849759183));
#87336=CARTESIAN_POINT('Ctrl Pts',(13.0532051588045,-2.23721586799097,2.52088332885009));
#87337=CARTESIAN_POINT('Ctrl Pts',(12.0626157696289,0.408557624148013,2.36285816010837));
#87338=CARTESIAN_POINT('Ctrl Pts',(13.7376328649657,2.6835750260205,2.20483299136663));
#87339=CARTESIAN_POINT('Ctrl Pts',(16.5582177838479,2.52331145792478,2.04680782262489));
#87340=CARTESIAN_POINT('Ctrl Pts',(17.9647577610854,0.0732036785898677,
1.88878265388316));
#87341=CARTESIAN_POINT('Ctrl Pts',(16.6808493574509,-2.44333648707884,1.73075748514142));
#87342=CARTESIAN_POINT('Ctrl Pts',(13.8716125530259,-2.74260341607019,1.57273231639968));
#87343=CARTESIAN_POINT('Ctrl Pts',(12.0863558135253,-0.553029801627824,
1.41470714765794));
#87344=CARTESIAN_POINT('Ctrl Pts',(12.9451710463004,2.13841851363382,1.2566819789162));
#87345=CARTESIAN_POINT('Ctrl Pts',(15.6686767610793,2.88927691304951,1.09865681017448));
#87346=CARTESIAN_POINT('Ctrl Pts',(17.7854091902781,1.01823595067672,0.940631641432738));
#87347=CARTESIAN_POINT('Ctrl Pts',(17.3743807791228,-1.77692889679917,0.782606472691003));
#87348=CARTESIAN_POINT('Ctrl Pts',(14.8087915159287,-2.95937983964669,0.624581303949266));
#87349=CARTESIAN_POINT('Ctrl Pts',(12.4164593581283,-1.45664108884959,0.466556135207532));
#87350=CARTESIAN_POINT('Ctrl Pts',(12.3691365153999,1.3687011047629,0.308530966465794));
#87351=CARTESIAN_POINT('Ctrl Pts',(14.7082682063417,2.95054009376668,0.150505797724059));
#87352=CARTESIAN_POINT('Ctrl Pts',(17.3140818173384,1.85766858973412,-0.00751937101767656));
#87353=CARTESIAN_POINT('Ctrl Pts',(17.816056514554,-0.926786128220127,-0.165544539759413));
#87354=CARTESIAN_POINT('Ctrl Pts',(16.4525749211699,-2.21298286387085,-0.270894652253902));
#87355=CARTESIAN_POINT('Ctrl Pts',(15.649053482972,-2.42779823849155,-0.323569708501147));
#87356=CARTESIAN_POINT('Ctrl Pts',(17.0521313248951,1.75636581539771,6.10609621406853));
#87357=CARTESIAN_POINT('Ctrl Pts',(17.6337631743951,1.07684452411148,6.05339396398347));
#87358=CARTESIAN_POINT('Ctrl Pts',(18.0590096796851,-0.8932074130143,5.94801665765119));
#87359=CARTESIAN_POINT('Ctrl Pts',(15.9187450832242,-3.0543555400977,5.78996429507165));
#87360=CARTESIAN_POINT('Ctrl Pts',(12.945213219642,-2.43589245724096,5.63193912632992));
#87361=CARTESIAN_POINT('Ctrl Pts',(11.8363461757247,0.389391897954849,5.47391395758817));
#87362=CARTESIAN_POINT('Ctrl Pts',(13.5984178986409,2.86319110054791,5.31588878884644));
#87363=CARTESIAN_POINT('Ctrl Pts',(16.6323934060946,2.73775122332677,5.15786362010471));
#87364=CARTESIAN_POINT('Ctrl Pts',(18.1850099857178,0.128359596618317,4.99983845136296));
#87365=CARTESIAN_POINT('Ctrl Pts',(16.8473061475514,-2.59776755257373,4.84181328262124));
#87366=CARTESIAN_POINT('Ctrl Pts',(13.8332157248642,-2.96635320979502,4.68378811387949));
#87367=CARTESIAN_POINT('Ctrl Pts',(11.8779543788667,-0.643110097290728,
4.52576294513777));
#87368=CARTESIAN_POINT('Ctrl Pts',(12.7558751192975,2.26377405171339,4.36773777639603));
#87369=CARTESIAN_POINT('Ctrl Pts',(15.6702858352774,3.11631971786699,4.20971260765429));
#87370=CARTESIAN_POINT('Ctrl Pts',(17.9764280859206,1.14088827032916,4.05168743891255));
#87371=CARTESIAN_POINT('Ctrl Pts',(17.5815326550398,-1.86987670588675,3.89366227017082));
#87372=CARTESIAN_POINT('Ctrl Pts',(14.843957741748,-3.18377071320937,3.73563710142908));
#87373=CARTESIAN_POINT('Ctrl Pts',(12.2479874687677,-1.6084697256714,3.57761193268735));
#87374=CARTESIAN_POINT('Ctrl Pts',(12.1494031041135,1.42647988883321,3.41958676394561));
#87375=CARTESIAN_POINT('Ctrl Pts',(14.6376676200099,3.1669326258071,3.26156159520388));
#87376=CARTESIAN_POINT('Ctrl Pts',(17.454740145528,2.03346948748628,3.10353642646214));
#87377=CARTESIAN_POINT('Ctrl Pts',(18.0441943914605,-0.945318905954183,
2.9455112577204));
#87378=CARTESIAN_POINT('Ctrl Pts',(15.8711146142941,-3.06625287074756,2.78748608897867));
#87379=CARTESIAN_POINT('Ctrl Pts',(12.9075190924252,-2.40463524498535,2.62946092023693));
#87380=CARTESIAN_POINT('Ctrl Pts',(11.8428001296284,0.439131545904872,2.47143575149519));
#87381=CARTESIAN_POINT('Ctrl Pts',(13.6431651283877,2.8843971574036,2.31341058275346));
#87382=CARTESIAN_POINT('Ctrl Pts',(16.6748251503188,2.71214045663376,2.15538541401172));
#87383=CARTESIAN_POINT('Ctrl Pts',(18.1866218665578,0.0786817884310189,
1.99736024526999));
#87384=CARTESIAN_POINT('Ctrl Pts',(16.8066337112417,-2.62618065437941,1.83933507652825));
#87385=CARTESIAN_POINT('Ctrl Pts',(13.7871710263571,-2.94784286650975,1.68130990778652));
#87386=CARTESIAN_POINT('Ctrl Pts',(11.8683167313509,-0.594415126205828,
1.52328473904478));
#87387=CARTESIAN_POINT('Ctrl Pts',(12.791400376165,2.29844450863419,1.36525957030304));
#87388=CARTESIAN_POINT('Ctrl Pts',(15.7187163877207,3.10549249942535,1.20723440156131));
#87389=CARTESIAN_POINT('Ctrl Pts',(17.9938519596965,1.09443442170253,1.04920923281957));
#87390=CARTESIAN_POINT('Ctrl Pts',(17.5520647283902,-1.90990324814445,0.89118406407784));
#87391=CARTESIAN_POINT('Ctrl Pts',(14.794482657433,-3.18084149479233,0.733158895336105));
#87392=CARTESIAN_POINT('Ctrl Pts',(12.223123180386,-1.56564708468969,0.575133726594368));
#87393=CARTESIAN_POINT('Ctrl Pts',(12.172258989252,1.47112621694339,0.417108557852632));
#87394=CARTESIAN_POINT('Ctrl Pts',(14.6864368060542,3.17134023708901,0.259083389110896));
#87395=CARTESIAN_POINT('Ctrl Pts',(17.4872533658312,1.99668499955184,0.10105822036916));
#87396=CARTESIAN_POINT('Ctrl Pts',(18.0267927398745,-0.996141061024619,
-0.0569669483725758));
#87397=CARTESIAN_POINT('Ctrl Pts',(16.5612766302089,-2.37858879294967,-0.162317060867066));
#87398=CARTESIAN_POINT('Ctrl Pts',(15.6976246250374,-2.60947961952043,-0.214992117114311));
#87399=CARTESIAN_POINT('Ctrl Pts',(17.1950081078255,1.87865033701126,6.21467380545536));
#87400=CARTESIAN_POINT('Ctrl Pts',(17.8171352640822,1.15181832303692,6.16197155537032));
#87401=CARTESIAN_POINT('Ctrl Pts',(18.2719889645311,-0.955395734060278,
6.05659424903803));
#87402=CARTESIAN_POINT('Ctrl Pts',(15.9827114289604,-3.26701078696264,5.89854188645848));
#87403=CARTESIAN_POINT('Ctrl Pts',(12.8021515543266,-2.60548807406771,5.74051671771676));
#87404=CARTESIAN_POINT('Ctrl Pts',(11.6160811881801,0.416502766057701,5.58249154897501));
#87405=CARTESIAN_POINT('Ctrl Pts',(13.5008346985671,3.0625367897826,5.42446638023328));
#87406=CARTESIAN_POINT('Ctrl Pts',(16.7460465215216,2.92836333596666,5.26644121149155));
#87407=CARTESIAN_POINT('Ctrl Pts',(18.4067618662335,0.137296454606198,5.10841604274981));
#87408=CARTESIAN_POINT('Ctrl Pts',(16.9759222630251,-2.77863349726747,4.95039087400808));
#87409=CARTESIAN_POINT('Ctrl Pts',(13.7519799961451,-3.17288141708336,4.79236570526634));
#87410=CARTESIAN_POINT('Ctrl Pts',(11.6605863044662,-0.687885741352231,
4.63434053652461));
#87411=CARTESIAN_POINT('Ctrl Pts',(12.5996310526731,2.42138616447946,4.47631536778287));
#87412=CARTESIAN_POINT('Ctrl Pts',(15.7169535522147,3.33328913423425,4.31829019904113));
#87413=CARTESIAN_POINT('Ctrl Pts',(18.1836577424154,1.22032102581132,4.1602650302994));
#87414=CARTESIAN_POINT('Ctrl Pts',(17.7612682676234,-2.00006426502227,4.00223986155766));
#87415=CARTESIAN_POINT('Ctrl Pts',(14.8330935170321,-3.40543631110413,3.84421469281592));
#87416=CARTESIAN_POINT('Ctrl Pts',(12.0563824324444,-1.72045718819729,3.68618952407419));
#87417=CARTESIAN_POINT('Ctrl Pts',(11.9509342688227,1.52579656265371,3.52816435533245));
#87418=CARTESIAN_POINT('Ctrl Pts',(14.6124407331258,3.38742589533789,3.37013918659072));
#87419=CARTESIAN_POINT('Ctrl Pts',(17.625648006379,2.17504696600075,3.21211401784898));
#87420=CARTESIAN_POINT('Ctrl Pts',(18.2561421825157,-1.01113541705537,3.05408884910725));
#87421=CARTESIAN_POINT('Ctrl Pts',(15.9317647550255,-3.27973645267473,2.89606368036551));
#87422=CARTESIAN_POINT('Ctrl Pts',(12.761833026046,-2.57205462197974,2.73803851162378));
#87423=CARTESIAN_POINT('Ctrl Pts',(11.6229844896278,0.469705467661738,2.58001334288204));
#87424=CARTESIAN_POINT('Ctrl Pts',(13.5486973918097,3.0852192887867,2.4219881741403));
#87425=CARTESIAN_POINT('Ctrl Pts',(16.7914325167898,2.90096945534274,2.26396300539856));
#87426=CARTESIAN_POINT('Ctrl Pts',(18.40848597203,0.0841598982721637,2.10593783665683));
#87427=CARTESIAN_POINT('Ctrl Pts',(16.9324180650325,-2.80902482167996,1.94791266791509));
#87428=CARTESIAN_POINT('Ctrl Pts',(13.7027294996884,-3.15308231694932,1.78988749917336));
#87429=CARTESIAN_POINT('Ctrl Pts',(11.6502776491765,-0.635800450783829,
1.63186233043162));
#87430=CARTESIAN_POINT('Ctrl Pts',(12.6376297060296,2.45847050363454,1.47383716168988));
#87431=CARTESIAN_POINT('Ctrl Pts',(15.7687560143621,3.3217080858012,1.31581199294815));
#87432=CARTESIAN_POINT('Ctrl Pts',(18.2022947291149,1.17063289272834,1.15778682420641));
#87433=CARTESIAN_POINT('Ctrl Pts',(17.7297486776575,-2.04287759948972,0.999761655464675));
#87434=CARTESIAN_POINT('Ctrl Pts',(14.7801737989374,-3.40230314993799,0.841736486722942));
#87435=CARTESIAN_POINT('Ctrl Pts',(12.0297870026437,-1.67465308052978,0.683711317981204));
#87436=CARTESIAN_POINT('Ctrl Pts',(11.9753814631039,1.57355132912387,0.525686149239469));
#87437=CARTESIAN_POINT('Ctrl Pts',(14.6646054057666,3.39214038041133,0.367660980497734));
#87438=CARTESIAN_POINT('Ctrl Pts',(17.6604249143241,2.13570140936955,0.209635811755997));
#87439=CARTESIAN_POINT('Ctrl Pts',(18.2375289651951,-1.06549599382911,0.0516106430142612));
#87440=CARTESIAN_POINT('Ctrl Pts',(16.669978339248,-2.54419472202848,-0.0537394694802286));
#87441=CARTESIAN_POINT('Ctrl Pts',(15.7461957671028,-2.7911610005493,-0.106414525727474));
#87442=CARTESIAN_POINT('Ctrl Pts',(17.337884890756,2.00093485862481,6.3232513968422));
#87443=CARTESIAN_POINT('Ctrl Pts',(18.0005073537692,1.22679212196236,6.27054914675716));
#87444=CARTESIAN_POINT('Ctrl Pts',(18.4849682493773,-1.01758405510626,6.16517184042487));
#87445=CARTESIAN_POINT('Ctrl Pts',(16.0466777746965,-3.47966603382759,6.00711947784533));
#87446=CARTESIAN_POINT('Ctrl Pts',(12.6590898890111,-2.77508369089444,5.8490943091036));
#87447=CARTESIAN_POINT('Ctrl Pts',(11.3958162006355,0.44361363416055,5.69106914036185));
#87448=CARTESIAN_POINT('Ctrl Pts',(13.4032514984932,3.26188247901728,5.53304397162013));
#87449=CARTESIAN_POINT('Ctrl Pts',(16.8596996369486,3.11897544860654,5.37501880287838));
#87450=CARTESIAN_POINT('Ctrl Pts',(18.6285137467491,0.146233312594081,5.21699363413665));
#87451=CARTESIAN_POINT('Ctrl Pts',(17.1045383784986,-2.9594994419612,5.05896846539492));
#87452=CARTESIAN_POINT('Ctrl Pts',(13.6707442674259,-3.3794096243717,4.90094329665316));
#87453=CARTESIAN_POINT('Ctrl Pts',(11.4432182300656,-0.732661385413735,
4.74291812791145));
#87454=CARTESIAN_POINT('Ctrl Pts',(12.4433869860487,2.57899827724554,4.58489295916969));
#87455=CARTESIAN_POINT('Ctrl Pts',(15.7636212691519,3.55025855060152,4.42686779042797));
#87456=CARTESIAN_POINT('Ctrl Pts',(18.3908873989101,1.29975378129348,4.26884262168623));
#87457=CARTESIAN_POINT('Ctrl Pts',(17.9410038802068,-2.13025182415778,4.1108174529445));
#87458=CARTESIAN_POINT('Ctrl Pts',(14.8222292923162,-3.62710190899889,3.95279228420276));
#87459=CARTESIAN_POINT('Ctrl Pts',(11.8647773961211,-1.83244465072319,3.79476711546102));
#87460=CARTESIAN_POINT('Ctrl Pts',(11.7524654335319,1.6251132364742,3.63674194671928));
#87461=CARTESIAN_POINT('Ctrl Pts',(14.5872138462417,3.6079191648687,3.47871677797756));
#87462=CARTESIAN_POINT('Ctrl Pts',(17.7965558672301,2.31662444451522,3.32069160923582));
#87463=CARTESIAN_POINT('Ctrl Pts',(18.4680899735709,-1.07695192815655,3.16266644049408));
#87464=CARTESIAN_POINT('Ctrl Pts',(15.9924148957568,-3.49322003460191,3.00464127175234));
#87465=CARTESIAN_POINT('Ctrl Pts',(12.6161469596667,-2.73947399897413,2.8466161030106));
#87466=CARTESIAN_POINT('Ctrl Pts',(11.4031688496272,0.500279389418601,2.68859093426888));
#87467=CARTESIAN_POINT('Ctrl Pts',(13.4542296552316,3.28604142016981,2.53056576552714));
#87468=CARTESIAN_POINT('Ctrl Pts',(16.9080398832607,3.08979845405171,2.3725405967854));
#87469=CARTESIAN_POINT('Ctrl Pts',(18.6303500775023,0.0896380081133119,
2.21451542804366));
#87470=CARTESIAN_POINT('Ctrl Pts',(17.0582024188234,-2.99186898898052,2.05649025930192));
#87471=CARTESIAN_POINT('Ctrl Pts',(13.6182879730196,-3.35832176738888,1.89846509056019));
#87472=CARTESIAN_POINT('Ctrl Pts',(11.4322385670019,-0.677185775361829,
1.74043992181845));
#87473=CARTESIAN_POINT('Ctrl Pts',(12.4838590358943,2.61849649863489,1.58241475307672));
#87474=CARTESIAN_POINT('Ctrl Pts',(15.8187956410036,3.53792367217705,1.42438958433498));
#87475=CARTESIAN_POINT('Ctrl Pts',(18.4107374985333,1.24683136375414,1.26636441559324));
#87476=CARTESIAN_POINT('Ctrl Pts',(17.9074326269248,-2.17585195083499,1.10833924685151));
#87477=CARTESIAN_POINT('Ctrl Pts',(14.7658649404417,-3.62376480508365,0.950314078109777));
#87478=CARTESIAN_POINT('Ctrl Pts',(11.8364508249014,-1.78365907636988,0.792288909368042));
#87479=CARTESIAN_POINT('Ctrl Pts',(11.778503936956,1.67597644130436,0.634263740626305));
#87480=CARTESIAN_POINT('Ctrl Pts',(14.6427740054791,3.61294052373364,0.476238571884569));
#87481=CARTESIAN_POINT('Ctrl Pts',(17.833596462817,2.27471781918727,0.318213403142834));
#87482=CARTESIAN_POINT('Ctrl Pts',(18.4482651905155,-1.1348509266336,0.160188234401097));
#87483=CARTESIAN_POINT('Ctrl Pts',(16.7786800482871,-2.7098006511073,0.0548381219066082));
#87484=CARTESIAN_POINT('Ctrl Pts',(15.7947669091682,-2.97284238157818,0.00216306565936305));
#87485=CARTESIAN_POINT('',(16.915303916182,1.63722281354575,-0.00127815611057945));
#87486=CARTESIAN_POINT('Ctrl Pts',(15.7937992825328,-2.9692229537457,-1.0547118733939E-15));
#87487=CARTESIAN_POINT('Ctrl Pts',(15.8877631253111,-2.93485056032367,7.25862686238765E-15));
#87488=CARTESIAN_POINT('Ctrl Pts',(15.9796217175756,-2.89562062532635,1.07572107203012E-14));
#87489=CARTESIAN_POINT('Ctrl Pts',(16.0691601441602,-2.85186997887123,1.02695629777827E-14));
#87490=CARTESIAN_POINT('Ctrl Pts',(16.1600181502287,-2.80747455388162,9.77472848895889E-15));
#87491=CARTESIAN_POINT('Ctrl Pts',(16.2484877472778,-2.75842350101316,3.64929086425418E-15));
#87492=CARTESIAN_POINT('Ctrl Pts',(16.3343150074473,-2.70502273461287,-5.55111512312578E-16));
#87493=CARTESIAN_POINT('Ctrl Pts',(16.420213530084,-2.65157762949835,-4.76300480873003E-15));
#87494=CARTESIAN_POINT('Ctrl Pts',(16.5034659125644,-2.59377480350178,1.56120952333745E-14));
#87495=CARTESIAN_POINT('Ctrl Pts',(16.5837791746464,-2.53188639447444,1.50435219836709E-14));
#87496=CARTESIAN_POINT('Ctrl Pts',(16.6470097276724,-2.48316171031579,1.45958848178708E-14));
#87497=CARTESIAN_POINT('Ctrl Pts',(16.708417838421,-2.43190381471692,1.97835687267867E-15));
#87498=CARTESIAN_POINT('Ctrl Pts',(16.7678402202613,-2.37823520474345,-3.71924713249427E-15));
#87499=CARTESIAN_POINT('Ctrl Pts',(16.7818815953477,-2.36555343299908,-4.8695573782049E-15));
#87500=CARTESIAN_POINT('Ctrl Pts',(16.7958146517509,-2.35273441817498,7.35895762980806E-15));
#87501=CARTESIAN_POINT('Ctrl Pts',(16.8096179419118,-2.33979804184713,3.99680288865056E-15));
#87502=CARTESIAN_POINT('Ctrl Pts',(16.8820575556246,-2.27190798859838,-1.27952815608437E-14));
#87503=CARTESIAN_POINT('Ctrl Pts',(16.9510310384028,-2.20069650513415,2.17879392813487E-15));
#87504=CARTESIAN_POINT('Ctrl Pts',(17.0162982669385,-2.12645339766838,-5.93969318174459E-15));
#87505=CARTESIAN_POINT('Ctrl Pts',(17.0812101119845,-2.05261454782477,-1.40139747026275E-14));
#87506=CARTESIAN_POINT('Ctrl Pts',(17.1424564417789,-1.97577620343073,4.24462762398128E-15));
#87507=CARTESIAN_POINT('Ctrl Pts',(17.1997573990558,-1.89619667621841,9.35362898246694E-15));
#87508=CARTESIAN_POINT('Ctrl Pts',(17.2557584952793,-1.81842239507851,1.43467336403883E-14));
#87509=CARTESIAN_POINT('Ctrl Pts',(17.3079914815835,-1.73802914831672,-8.69766376979819E-15));
#87510=CARTESIAN_POINT('Ctrl Pts',(17.3561478113119,-1.65524376258327,-6.24500451351651E-15));
#87511=CARTESIAN_POINT('Ctrl Pts',(17.3754619924059,-1.62204081831805,-5.26131025556974E-15));
#87512=CARTESIAN_POINT('Ctrl Pts',(17.394119841153,-1.58845297300426,-6.73148743896928E-15));
#87513=CARTESIAN_POINT('Ctrl Pts',(17.4120990805709,-1.55449458909069,-8.49320613838245E-15));
#87514=CARTESIAN_POINT('Ctrl Pts',(17.4253275583043,-1.52950923153335,-8.21298736870903E-15));
#87515=CARTESIAN_POINT('Ctrl Pts',(17.4381886433291,-1.50432328064783,-9.92679727242235E-15));
#87516=CARTESIAN_POINT('Ctrl Pts',(17.4506729597229,-1.47894245110775,-5.60662627435704E-15));
#87517=CARTESIAN_POINT('Ctrl Pts',(17.4574660965599,-1.46513188730399,-3.36795545207024E-15));
#87518=CARTESIAN_POINT('Ctrl Pts',(17.4641485246816,-1.45126166531956,-9.50468321427569E-15));
#87519=CARTESIAN_POINT('Ctrl Pts',(17.4707111365409,-1.43734914681016,-1.06581410364015E-14));
#87520=CARTESIAN_POINT('Ctrl Pts',(17.5106942755179,-1.35258622420957,-1.98793348162394E-14));
#87521=CARTESIAN_POINT('Ctrl Pts',(17.5462960054721,-1.26613123171125,-1.32361921656702E-14));
#87522=CARTESIAN_POINT('Ctrl Pts',(17.5772717642454,-1.17821446018303,-2.83106871279415E-15));
#87523=CARTESIAN_POINT('Ctrl Pts',(17.6081064320176,-1.09069813938794,7.52666060535023E-15));
#87524=CARTESIAN_POINT('Ctrl Pts',(17.6343575472885,-1.00173266645316,-3.25504417137631E-15));
#87525=CARTESIAN_POINT('Ctrl Pts',(17.6557334149071,-0.911535908124523,
-8.52096171399808E-15));
#87526=CARTESIAN_POINT('Ctrl Pts',(17.6587134931134,-0.898961288999205,
-8.66732429744353E-15));
#87527=CARTESIAN_POINT('Ctrl Pts',(17.6615987301009,-0.886362732909987,
-3.82633183530923E-15));
#87528=CARTESIAN_POINT('Ctrl Pts',(17.6643882507676,-0.873740826918426,
-1.63757896132211E-15));
#87529=CARTESIAN_POINT('Ctrl Pts',(17.6849564629332,-0.780674644090523,
1.63395851942713E-14));
#87530=CARTESIAN_POINT('Ctrl Pts',(17.7003250436256,-0.686338012910902,
-1.92404708757836E-14));
#87531=CARTESIAN_POINT('Ctrl Pts',(17.7105713114964,-0.591140293501985,
-1.74582570622306E-14));
#87532=CARTESIAN_POINT('Ctrl Pts',(17.7164074023686,-0.536917375625885,
-1.64431399580609E-14));
#87533=CARTESIAN_POINT('Ctrl Pts',(17.7205807502074,-0.482415289412221,
-1.20770545210332E-14));
#87534=CARTESIAN_POINT('Ctrl Pts',(17.7230986015199,-0.427712441435951,
-2.27318164292001E-14));
#87535=CARTESIAN_POINT('Ctrl Pts',(17.7236733846671,-0.415224700415009,
-2.47925753357554E-14));
#87536=CARTESIAN_POINT('Ctrl Pts',(17.7241617587452,-0.402728082302084,
5.67804429951126E-15));
#87537=CARTESIAN_POINT('Ctrl Pts',(17.7245636675657,-0.390232963134124,
7.04991620636974E-15));
#87538=CARTESIAN_POINT('Ctrl Pts',(17.7275525323397,-0.297310838444643,
1.56178684923478E-14));
#87539=CARTESIAN_POINT('Ctrl Pts',(17.7257709900994,-0.204325895882787,
1.14009966214644E-14));
#87540=CARTESIAN_POINT('Ctrl Pts',(17.7193534316054,-0.111650468563709,
-3.89965837399586E-15));
#87541=CARTESIAN_POINT('Ctrl Pts',(17.7129132516647,-0.018648366819267,
-1.92542471124444E-14));
#87542=CARTESIAN_POINT('Ctrl Pts',(17.701803954752,0.074043009764724,-1.90773904346453E-14));
#87543=CARTESIAN_POINT('Ctrl Pts',(17.6861107070086,0.166035470154942,-1.06165076729781E-14));
#87544=CARTESIAN_POINT('Ctrl Pts',(17.6705478903124,0.257263355032181,-2.22594571532359E-15));
#87545=CARTESIAN_POINT('Ctrl Pts',(17.6504765789002,0.347804777454888,-9.29780401233961E-15));
#87546=CARTESIAN_POINT('Ctrl Pts',(17.6259361013488,0.437255629196133,-1.19626530903361E-14));
#87547=CARTESIAN_POINT('Ctrl Pts',(17.6168824130534,0.470256622258459,-1.24188389511132E-14));
#87548=CARTESIAN_POINT('Ctrl Pts',(17.607220033895,0.503108861729303,-1.77227151771264E-14));
#87549=CARTESIAN_POINT('Ctrl Pts',(17.5969495907262,0.535790803903075,-1.23789867245705E-14));
#87550=CARTESIAN_POINT('Ctrl Pts',(17.5906923635436,0.555702148875279,-9.16506532922899E-15));
#87551=CARTESIAN_POINT('Ctrl Pts',(17.5842094210688,0.575550268330647,2.38196241363701E-15));
#87552=CARTESIAN_POINT('Ctrl Pts',(17.5775007819672,0.595330144314736,-1.24206200879939E-14));
#87553=CARTESIAN_POINT('Ctrl Pts',(17.5720344395212,0.611447209792455,-2.43995415110235E-14));
#87554=CARTESIAN_POINT('Ctrl Pts',(17.5664177473268,0.627520100869461,3.28653594930177E-15));
#87555=CARTESIAN_POINT('Ctrl Pts',(17.5606568980948,0.643529501722759,2.28983498828939E-15));
#87556=CARTESIAN_POINT('Ctrl Pts',(17.5300998777373,0.72844746573855,1.8961345380147E-15));
#87557=CARTESIAN_POINT('Ctrl Pts',(17.4954544625937,0.81169001210649,8.70397767353563E-15));
#87558=CARTESIAN_POINT('Ctrl Pts',(17.4567798259733,0.892884379764742,7.42461647718073E-15));
#87559=CARTESIAN_POINT('Ctrl Pts',(17.4252161779729,0.959149784286503,6.38048755973252E-15));
#87560=CARTESIAN_POINT('Ctrl Pts',(17.3909678991583,1.02405068948786,8.96555908749261E-15));
#87561=CARTESIAN_POINT('Ctrl Pts',(17.3540486134849,1.08736649490362,-1.60982338570648E-15));
#87562=CARTESIAN_POINT('Ctrl Pts',(17.3403704993332,1.11082417557878,-5.21161029651093E-15));
#87563=CARTESIAN_POINT('Ctrl Pts',(17.3263256078231,1.13406409955685,1.28764437023275E-14));
#87564=CARTESIAN_POINT('Ctrl Pts',(17.3119141100336,1.15707434952577,-6.28663787693995E-15));
#87565=CARTESIAN_POINT('Ctrl Pts',(17.3022209349234,1.17255104636444,-1.95408450057356E-14));
#87566=CARTESIAN_POINT('Ctrl Pts',(17.2923614563489,1.18792433165914,9.0007685035821E-15));
#87567=CARTESIAN_POINT('Ctrl Pts',(17.2823446805049,1.20317728665099,9.74220704108575E-15));
#87568=CARTESIAN_POINT('Ctrl Pts',(17.2351636329007,1.27502180097183,8.69901979580413E-15));
#87569=CARTESIAN_POINT('Ctrl Pts',(17.1844507000559,1.34427231397538,8.43316798846986E-15));
#87570=CARTESIAN_POINT('Ctrl Pts',(17.1302392162511,1.41057629209039,7.63278329429795E-15));
#87571=CARTESIAN_POINT('Ctrl Pts',(17.0809261548577,1.47088919839622,9.33123635964826E-15));
#87572=CARTESIAN_POINT('Ctrl Pts',(17.0287176381672,1.52876397615804,-5.08825234704773E-15));
#87573=CARTESIAN_POINT('Ctrl Pts',(16.9736175325606,1.58390431335901,8.71091393461754E-15));
#87574=CARTESIAN_POINT('Ctrl Pts',(16.955089701729,1.60244567237107,1.28632355881959E-14));
#87575=CARTESIAN_POINT('Ctrl Pts',(16.9362347568812,1.62067756637814,-1.19777121980603E-15));
#87576=CARTESIAN_POINT('Ctrl Pts',(16.9170623502469,1.63859592449701,9.04051139505313E-15));
#87577=CARTESIAN_POINT('Ctrl Pts',(16.9134659966651,1.63598720337494,6.));
#87578=CARTESIAN_POINT('Ctrl Pts',(16.9755094815351,1.5776815625216,5.99999999999999));
#87579=CARTESIAN_POINT('Ctrl Pts',(17.034139121574,1.51618400144596,5.99999999999998));
#87580=CARTESIAN_POINT('Ctrl Pts',(17.0893566813826,1.45188668377136,5.99999999999998));
#87581=CARTESIAN_POINT('Ctrl Pts',(17.1457272627278,1.38624674624397,5.99999999999998));
#87582=CARTESIAN_POINT('Ctrl Pts',(17.1985421988915,1.31768842238335,6.));
#87583=CARTESIAN_POINT('Ctrl Pts',(17.2477776475324,1.24658007436298,6.00000000000001));
#87584=CARTESIAN_POINT('Ctrl Pts',(17.2982360478219,1.17370547714931,6.00000000000001));
#87585=CARTESIAN_POINT('Ctrl Pts',(17.3449354505362,1.09815203002923,6.00000000000002));
#87586=CARTESIAN_POINT('Ctrl Pts',(17.3878162017473,1.02027348726958,6.));
#87587=CARTESIAN_POINT('Ctrl Pts',(17.4063927730161,0.98653535864483,5.99999999999999));
#87588=CARTESIAN_POINT('Ctrl Pts',(17.4242522071428,0.952360385941308,5.99999999999999));
#87589=CARTESIAN_POINT('Ctrl Pts',(17.4413873608898,0.917775372037375,6.));
#87590=CARTESIAN_POINT('Ctrl Pts',(17.4513051088949,0.897757725407784,6.00000000000001));
#87591=CARTESIAN_POINT('Ctrl Pts',(17.4609801930981,0.877602693578679,5.99999999999999));
#87592=CARTESIAN_POINT('Ctrl Pts',(17.4704109979228,0.8573153278544,6.));
#87593=CARTESIAN_POINT('Ctrl Pts',(17.4789439761822,0.838959349347455,6.00000000000001));
#87594=CARTESIAN_POINT('Ctrl Pts',(17.4872793672599,0.820489262936239,6.00000000000001));
#87595=CARTESIAN_POINT('Ctrl Pts',(17.4954022352014,0.801940725847788,6.00000000000001));
#87596=CARTESIAN_POINT('Ctrl Pts',(17.532082498778,0.718181487821601,5.99999999999999));
#87597=CARTESIAN_POINT('Ctrl Pts',(17.564479455655,0.632730199218269,5.99999999999999));
#87598=CARTESIAN_POINT('Ctrl Pts',(17.5925671692333,0.545988213295408,5.99999999999999));
#87599=CARTESIAN_POINT('Ctrl Pts',(17.6210371396809,0.458065721174328,6.));
#87600=CARTESIAN_POINT('Ctrl Pts',(17.6450802539788,0.368816386817013,5.99999999999999));
#87601=CARTESIAN_POINT('Ctrl Pts',(17.6646303946722,0.278621061222165,5.99999999999998));
#87602=CARTESIAN_POINT('Ctrl Pts',(17.6842040041827,0.18831746133696,5.99999999999998));
#87603=CARTESIAN_POINT('Ctrl Pts',(17.6992742681111,0.0970647054962511,
6.));
#87604=CARTESIAN_POINT('Ctrl Pts',(17.7097292318061,0.00522075650062019,
6.));
#87605=CARTESIAN_POINT('Ctrl Pts',(17.7136173613966,-0.0289353808343625,
6.));
#87606=CARTESIAN_POINT('Ctrl Pts',(17.7168666892977,-0.0631734552839064,
6.));
#87607=CARTESIAN_POINT('Ctrl Pts',(17.7194696669028,-0.09747552158852,5.99999999999999));
#87608=CARTESIAN_POINT('Ctrl Pts',(17.7212325560646,-0.120706893535899,
5.99999999999999));
#87609=CARTESIAN_POINT('Ctrl Pts',(17.722698957133,-0.143967621373419,5.99999999999999));
#87610=CARTESIAN_POINT('Ctrl Pts',(17.7238662552278,-0.167252159912536,
6.));
#87611=CARTESIAN_POINT('Ctrl Pts',(17.7245262789947,-0.180417904726593,
6.));
#87612=CARTESIAN_POINT('Ctrl Pts',(17.7250904489575,-0.193587605540001,
5.99999999999998));
#87613=CARTESIAN_POINT('Ctrl Pts',(17.7255582477108,-0.206751979691985,
5.99999999999998));
#87614=CARTESIAN_POINT('Ctrl Pts',(17.7290248924967,-0.304307196955097,
6.00000000000001));
#87615=CARTESIAN_POINT('Ctrl Pts',(17.7272102314639,-0.401701395411429,
6.));
#87616=CARTESIAN_POINT('Ctrl Pts',(17.7200480989972,-0.4985064694598,6.));
#87617=CARTESIAN_POINT('Ctrl Pts',(17.7128859665305,-0.595311543508181,
6.));
#87618=CARTESIAN_POINT('Ctrl Pts',(17.7003768098819,-0.691528572964534,
6.00000000000001));
#87619=CARTESIAN_POINT('Ctrl Pts',(17.6824005104444,-0.786748819384737,
6.00000000000001));
#87620=CARTESIAN_POINT('Ctrl Pts',(17.665301687038,-0.877321085601708,6.00000000000001));
#87621=CARTESIAN_POINT('Ctrl Pts',(17.6432564988628,-0.966992484953733,
5.99999999999999));
#87622=CARTESIAN_POINT('Ctrl Pts',(17.6165400759011,-1.05552334469227,6.));
#87623=CARTESIAN_POINT('Ctrl Pts',(17.6012165843948,-1.10630117072041,6.));
#87624=CARTESIAN_POINT('Ctrl Pts',(17.5843553947488,-1.15670375619126,6.00000000000001));
#87625=CARTESIAN_POINT('Ctrl Pts',(17.5660009192215,-1.20668470741449,5.99999999999999));
#87626=CARTESIAN_POINT('Ctrl Pts',(17.5600040426582,-1.22301476242238,5.99999999999998));
#87627=CARTESIAN_POINT('Ctrl Pts',(17.5538468430946,-1.23930175643138,6.00000000000002));
#87628=CARTESIAN_POINT('Ctrl Pts',(17.5475394190055,-1.25552261396836,6.00000000000002));
#87629=CARTESIAN_POINT('Ctrl Pts',(17.5132439135909,-1.34372066433486,6.00000000000001));
#87630=CARTESIAN_POINT('Ctrl Pts',(17.4744620559964,-1.43010229333925,6.00000000000001));
#87631=CARTESIAN_POINT('Ctrl Pts',(17.4315373968039,-1.51442487125201,6.));
#87632=CARTESIAN_POINT('Ctrl Pts',(17.3877735627611,-1.60039595116852,5.99999999999999));
#87633=CARTESIAN_POINT('Ctrl Pts',(17.3397030795252,-1.68422740148093,5.99999999999998));
#87634=CARTESIAN_POINT('Ctrl Pts',(17.2876347517893,-1.76565902892484,5.99999999999998));
#87635=CARTESIAN_POINT('Ctrl Pts',(17.2346998347258,-1.84844594820065,5.99999999999999));
#87636=CARTESIAN_POINT('Ctrl Pts',(17.1776325286954,-1.92875332663683,6.));
#87637=CARTESIAN_POINT('Ctrl Pts',(17.1167056749116,-2.006292820283,5.99999999999999));
#87638=CARTESIAN_POINT('Ctrl Pts',(17.0750631441813,-2.05928982482935,5.99999999999998));
#87639=CARTESIAN_POINT('Ctrl Pts',(17.0316165436599,-2.1109935011868,5.99999999999999));
#87640=CARTESIAN_POINT('Ctrl Pts',(16.9864408800736,-2.1613047605532,6.00000000000001));
#87641=CARTESIAN_POINT('Ctrl Pts',(16.9750475422705,-2.17399329964164,6.00000000000001));
#87642=CARTESIAN_POINT('Ctrl Pts',(16.9635434048419,-2.18659396301802,5.99999999999998));
#87643=CARTESIAN_POINT('Ctrl Pts',(16.9519414333288,-2.19909266058292,5.99999999999998));
#87644=CARTESIAN_POINT('Ctrl Pts',(16.8830336246512,-2.27332641124779,6.));
#87645=CARTESIAN_POINT('Ctrl Pts',(16.8105865574123,-2.34406896254778,5.99999999999998));
#87646=CARTESIAN_POINT('Ctrl Pts',(16.7349147382584,-2.4110269921092,5.99999999999999));
#87647=CARTESIAN_POINT('Ctrl Pts',(16.6721145810702,-2.46659556213289,6.));
#87648=CARTESIAN_POINT('Ctrl Pts',(16.6070923153041,-2.51955756893482,6.00000000000001));
#87649=CARTESIAN_POINT('Ctrl Pts',(16.5400041594286,-2.56973166063313,6.00000000000001));
#87650=CARTESIAN_POINT('Ctrl Pts',(16.5180622947882,-2.58614160832257,6.00000000000001));
#87651=CARTESIAN_POINT('Ctrl Pts',(16.4958992912228,-2.60225321472728,6.00000000000001));
#87652=CARTESIAN_POINT('Ctrl Pts',(16.4735201854318,-2.61805974701069,6.00000000000001));
#87653=CARTESIAN_POINT('Ctrl Pts',(16.4507974239471,-2.63410900591904,6.00000000000001));
#87654=CARTESIAN_POINT('Ctrl Pts',(16.4278464912961,-2.6498471559999,6.));
#87655=CARTESIAN_POINT('Ctrl Pts',(16.4047016736817,-2.66524800157915,6.));
#87656=CARTESIAN_POINT('Ctrl Pts',(16.3197414959508,-2.72178154612555,6.));
#87657=CARTESIAN_POINT('Ctrl Pts',(16.2321168885192,-2.77381412681324,6.));
#87658=CARTESIAN_POINT('Ctrl Pts',(16.1421188622891,-2.82103724255303,6.));
#87659=CARTESIAN_POINT('Ctrl Pts',(16.058344827335,-2.86499455044454,6.00000000000001));
#87660=CARTESIAN_POINT('Ctrl Pts',(15.9725134939175,-2.90478489918908,6.00000000000001));
#87661=CARTESIAN_POINT('Ctrl Pts',(15.8848316115121,-2.94013000968632,6.00000000000001));
#87662=CARTESIAN_POINT('Ctrl Pts',(15.8554933457997,-2.9519564465163,6.00000000000001));
#87663=CARTESIAN_POINT('Ctrl Pts',(15.8259477042398,-2.96328493422549,6.00000000000001));
#87664=CARTESIAN_POINT('Ctrl Pts',(15.7962062164482,-2.97411882975737,6.00000000000001));
#87665=CARTESIAN_POINT('Ctrl Pts',(16.9136316953219,1.63579338079708,-0.00127815611057958));
#87666=CARTESIAN_POINT('Ctrl Pts',(16.9051833118704,1.64567671602558,-0.000852104073719735));
#87667=CARTESIAN_POINT('Ctrl Pts',(16.8966583601906,1.65549459987556,-0.000426052036859841));
#87668=CARTESIAN_POINT('Ctrl Pts',(16.8880578635265,1.66524585391345,0.));
#87669=CARTESIAN_POINT('Ctrl Pts',(14.2051896689321,-2.97300480210898,5.99773986754201));
#87670=CARTESIAN_POINT('Ctrl Pts',(13.2212227739548,-2.70994870041619,5.94506481129476));
#87671=CARTESIAN_POINT('Ctrl Pts',(11.5515433528338,-1.13493172195381,5.83971469880028));
#87672=CARTESIAN_POINT('Ctrl Pts',(12.1662514122567,2.27485164275103,5.68168953005853));
#87673=CARTESIAN_POINT('Ctrl Pts',(15.3572450886927,3.61313057072747,5.52366436131681));
#87674=CARTESIAN_POINT('Ctrl Pts',(18.2216707218686,1.67607095050132,5.36563919257506));
#87675=CARTESIAN_POINT('Ctrl Pts',(18.16372112867,-1.78375794773966,5.20761402383333));
#87676=CARTESIAN_POINT('Ctrl Pts',(15.234147542334,-3.62396028172564,5.0495888550916));
#87677=CARTESIAN_POINT('Ctrl Pts',(12.0924097431305,-2.17597071420578,4.89156368634986));
#87678=CARTESIAN_POINT('Ctrl Pts',(11.5890772899766,1.24689941213705,4.73353851760813));
#87679=CARTESIAN_POINT('Ctrl Pts',(14.1811599880455,3.53811546760277,4.57551334886638));
#87680=CARTESIAN_POINT('Ctrl Pts',(17.5162774785844,2.61863872630337,4.41748818012465));
#87681=CARTESIAN_POINT('Ctrl Pts',(18.5679550843236,-0.677222592335036,
4.25946301138291));
#87682=CARTESIAN_POINT('Ctrl Pts',(16.3817870007077,-3.35850399264624,4.10143784264118));
#87683=CARTESIAN_POINT('Ctrl Pts',(12.9416858874442,-2.99203138157406,3.94341267389944));
#87684=CARTESIAN_POINT('Ctrl Pts',(11.3694528936595,0.0896428835206473,
3.78538750515772));
#87685=CARTESIAN_POINT('Ctrl Pts',(13.0918565671579,3.08996613614193,3.62736233641597));
#87686=CARTESIAN_POINT('Ctrl Pts',(16.5458542345706,3.28621976149866,3.46933716767424));
#87687=CARTESIAN_POINT('Ctrl Pts',(18.5970263563853,0.500306538668845,3.3113119989325));
#87688=CARTESIAN_POINT('Ctrl Pts',(17.38398241508,-2.73962267337911,3.15328683019077));
#87689=CARTESIAN_POINT('Ctrl Pts',(14.0075312446594,-3.49340961705167,2.99526166144903));
#87690=CARTESIAN_POINT('Ctrl Pts',(11.5317218080708,-1.07701037592612,2.83723649270729));
#87691=CARTESIAN_POINT('Ctrl Pts',(12.2032923596136,2.31675017147752,2.67921132396556));
#87692=CARTESIAN_POINT('Ctrl Pts',(15.4128085563852,3.60811497096177,2.52118615522382));
#87693=CARTESIAN_POINT('Ctrl Pts',(18.2477108145854,1.62520143551189,2.36316098648209));
#87694=CARTESIAN_POINT('Ctrl Pts',(18.1353927575591,-1.8325441034938,2.20513581774035));
#87695=CARTESIAN_POINT('Ctrl Pts',(15.1777803543678,-3.62729875091689,2.04711064899861));
#87696=CARTESIAN_POINT('Ctrl Pts',(12.0588365095769,-2.13036744730225,1.88908548025688));
#87697=CARTESIAN_POINT('Ctrl Pts',(11.6089285681624,1.29982434138019,1.73106031151514));
#87698=CARTESIAN_POINT('Ctrl Pts',(14.2363372968936,3.55045119102204,1.57303514277341));
#87699=CARTESIAN_POINT('Ctrl Pts',(17.5567517477241,2.57913831033334,1.41500997403167));
#87700=CARTESIAN_POINT('Ctrl Pts',(18.5569748354369,-0.732701268045499,
1.25698480528994));
#87701=CARTESIAN_POINT('Ctrl Pts',(16.3293278072767,-3.3795928169039,1.0989596365482));
#87702=CARTESIAN_POINT('Ctrl Pts',(12.8953475337801,-2.95966043224143,0.940934467806465));
#87703=CARTESIAN_POINT('Ctrl Pts',(11.3712890776038,0.146241897576049,0.782909299064727));
#87704=CARTESIAN_POINT('Ctrl Pts',(13.1401999240478,3.11914361205027,0.624884130322993));
#87705=CARTESIAN_POINT('Ctrl Pts',(16.5968342039323,3.26206136074565,0.466858961581257));
#87706=CARTESIAN_POINT('Ctrl Pts',(18.6043812699741,0.443634682954898,0.30883379283952));
#87707=CARTESIAN_POINT('Ctrl Pts',(17.3410334970383,-2.77522949326083,0.150808624097785));
#87708=CARTESIAN_POINT('Ctrl Pts',(13.9532726620765,-3.47986248795946,-0.00721654464395101));
#87709=CARTESIAN_POINT('Ctrl Pts',(11.5152477272064,-1.01804953619222,-0.165241713385687));
#87710=CARTESIAN_POINT('Ctrl Pts',(11.9990787995815,1.22570074963817,-0.270591825880177));
#87711=CARTESIAN_POINT('Ctrl Pts',(12.660961939353,1.99984548567625,-0.323266882127422));
#87712=CARTESIAN_POINT('Ctrl Pts',(14.2536953592163,-2.79156824484793,6.10617114577956));
#87713=CARTESIAN_POINT('Ctrl Pts',(13.3297780025906,-2.54456593271639,6.05349608953231));
#87714=CARTESIAN_POINT('Ctrl Pts',(11.7619957885252,-1.06566910111593,5.94814597703782));
#87715=CARTESIAN_POINT('Ctrl Pts',(12.3391894403214,2.13602198124237,5.79012080829609));
#87716=CARTESIAN_POINT('Ctrl Pts',(15.3354431329929,3.3926284137103,5.63209563955435));
#87717=CARTESIAN_POINT('Ctrl Pts',(18.0250585791671,1.57378368114728,5.47407047081262));
#87718=CARTESIAN_POINT('Ctrl Pts',(17.9706455341359,-1.67489875558656,5.31604530207088));
#87719=CARTESIAN_POINT('Ctrl Pts',(15.2198579845297,-3.40279720903209,5.15802013332914));
#87720=CARTESIAN_POINT('Ctrl Pts',(12.2698541810803,-2.04317555867616,4.99999496458742));
#87721=CARTESIAN_POINT('Ctrl Pts',(11.7972391042971,1.17080362634199,4.84196979584567));
#87722=CARTESIAN_POINT('Ctrl Pts',(14.2311321618581,3.32219133280872,4.68394462710394));
#87723=CARTESIAN_POINT('Ctrl Pts',(17.3627140795262,2.45882842432408,4.5259194583622));
#87724=CARTESIAN_POINT('Ctrl Pts',(18.3502098971975,-0.635893047369115,
4.36789428962046));
#87725=CARTESIAN_POINT('Ctrl Pts',(16.297459294241,-3.15354118816609,4.20986912087873));
#87726=CARTESIAN_POINT('Ctrl Pts',(13.0673006950891,-2.80943367009216,4.05184395213699));
#87727=CARTESIAN_POINT('Ctrl Pts',(11.5910179471305,0.0841721570161353,
3.89381878339526));
#87728=CARTESIAN_POINT('Ctrl Pts',(13.2083067575408,2.90139166179291,3.73579361465352));
#87729=CARTESIAN_POINT('Ctrl Pts',(16.451513831841,3.08566831956807,3.57776844591179));
#87730=CARTESIAN_POINT('Ctrl Pts',(18.3775070074704,0.469773827827989,3.41974327717005));
#87731=CARTESIAN_POINT('Ctrl Pts',(17.2384927200562,-2.57242896225573,3.26171810842832));
#87732=CARTESIAN_POINT('Ctrl Pts',(14.0680996346029,-3.28021379120878,3.10369293968658));
#87733=CARTESIAN_POINT('Ctrl Pts',(11.7433839131305,-1.01128257938712,2.94566777094485));
#87734=CARTESIAN_POINT('Ctrl Pts',(12.3739698524913,2.17536352627309,2.78764260220311));
#87735=CARTESIAN_POINT('Ctrl Pts',(15.3876156730016,3.38791890600118,2.62961743346137));
#87736=CARTESIAN_POINT('Ctrl Pts',(18.0495094969287,1.52601863126421,2.47159226471964));
#87737=CARTESIAN_POINT('Ctrl Pts',(17.9440459870497,-1.72070758949588,2.3135670959779));
#87738=CARTESIAN_POINT('Ctrl Pts',(15.1669307736936,-3.40593193810287,2.15554192723617));
#87739=CARTESIAN_POINT('Ctrl Pts',(12.2383298550521,-2.00035536825505,1.99751675849443));
#87740=CARTESIAN_POINT('Ctrl Pts',(11.8158788985427,1.22049865264372,1.83949158975269));
#87741=CARTESIAN_POINT('Ctrl Pts',(14.282942109527,3.33377423161536,1.68146642101096));
#87742=CARTESIAN_POINT('Ctrl Pts',(17.400718284694,2.42173864000821,1.52344125226922));
#87743=CARTESIAN_POINT('Ctrl Pts',(18.3398997510145,-0.687985970081409,
1.36541608352749));
#87744=CARTESIAN_POINT('Ctrl Pts',(16.248201580823,-3.17334300351367,1.20739091478575));
#87745=CARTESIAN_POINT('Ctrl Pts',(13.0237902787871,-2.77903825527531,1.04936574604401));
#87746=CARTESIAN_POINT('Ctrl Pts',(11.5927420724286,0.137317046057244,0.891340577302276));
#87747=CARTESIAN_POINT('Ctrl Pts',(13.253699815718,2.92878849450329,0.733315408560539));
#87748=CARTESIAN_POINT('Ctrl Pts',(16.4993825952861,3.06298425786033,0.575290239818805));
#87749=CARTESIAN_POINT('Ctrl Pts',(18.3844130653427,0.416560542509571,0.417265071077067));
#87750=CARTESIAN_POINT('Ctrl Pts',(17.1981648888767,-2.60586276889182,0.259239902335333));
#87751=CARTESIAN_POINT('Ctrl Pts',(14.0171523451665,-3.26749341640285,0.101214733593596));
#87752=CARTESIAN_POINT('Ctrl Pts',(11.7279152125851,-0.955920002181071,
-0.056810435148139));
#87753=CARTESIAN_POINT('Ctrl Pts',(12.1822190389883,1.15089867596211,-0.16216054764263));
#87754=CARTESIAN_POINT('Ctrl Pts',(12.803708770009,1.87779890178989,-0.214835603889875));
#87755=CARTESIAN_POINT('Ctrl Pts',(14.3022010495005,-2.61013168758689,6.2146024240171));
#87756=CARTESIAN_POINT('Ctrl Pts',(13.4383332312262,-2.3791831650166,6.16192736776986));
#87757=CARTESIAN_POINT('Ctrl Pts',(11.9724482242165,-0.996406480278056,
6.05657725527536));
#87758=CARTESIAN_POINT('Ctrl Pts',(12.512127468386,1.99719231973372,5.89855208653363));
#87759=CARTESIAN_POINT('Ctrl Pts',(15.3136411772931,3.17212625669313,5.74052691779189));
#87760=CARTESIAN_POINT('Ctrl Pts',(17.8284464364657,1.47149641179321,5.58250174905016));
#87761=CARTESIAN_POINT('Ctrl Pts',(17.7775699396018,-1.56603956343343,5.42447658030842));
#87762=CARTESIAN_POINT('Ctrl Pts',(15.2055684267254,-3.18163413633856,5.26645141156668));
#87763=CARTESIAN_POINT('Ctrl Pts',(12.44729861903,-1.91038040314654,5.10842624282495));
#87764=CARTESIAN_POINT('Ctrl Pts',(12.0054009186174,1.09470784054693,4.95040107408321));
#87765=CARTESIAN_POINT('Ctrl Pts',(14.2811043356706,3.10626719801468,4.79237590534148));
#87766=CARTESIAN_POINT('Ctrl Pts',(17.2091506804682,2.29901812234478,4.63435073659974));
#87767=CARTESIAN_POINT('Ctrl Pts',(18.1324647100716,-0.594563502403188,
4.47632556785801));
#87768=CARTESIAN_POINT('Ctrl Pts',(16.2131315877742,-2.94857838368594,4.31830039911627));
#87769=CARTESIAN_POINT('Ctrl Pts',(13.1929155027339,-2.62683595861024,4.16027523037453));
#87770=CARTESIAN_POINT('Ctrl Pts',(11.8125830006014,0.0787014305116236,
4.0022500616328));
#87771=CARTESIAN_POINT('Ctrl Pts',(13.3247569479238,2.71281718744388,3.84422489289106));
#87772=CARTESIAN_POINT('Ctrl Pts',(16.3571734291114,2.88511687763747,3.68619972414933));
#87773=CARTESIAN_POINT('Ctrl Pts',(18.1579876585555,0.439241116987135,3.52817455540759));
#87774=CARTESIAN_POINT('Ctrl Pts',(17.0930030250325,-2.40523525113236,3.37014938666586));
#87775=CARTESIAN_POINT('Ctrl Pts',(14.1286680245464,-3.0670179653659,3.21212421792412));
#87776=CARTESIAN_POINT('Ctrl Pts',(11.9550460181903,-0.945554782848137,
3.05409904918239));
#87777=CARTESIAN_POINT('Ctrl Pts',(12.5446473453691,2.03397688106867,2.89607388044065));
#87778=CARTESIAN_POINT('Ctrl Pts',(15.3624227896179,3.16772284104057,2.73804871169891));
#87779=CARTESIAN_POINT('Ctrl Pts',(17.851308179272,1.42683582701653,2.58002354295718));
#87780=CARTESIAN_POINT('Ctrl Pts',(17.7526992165401,-1.60887107549796,2.42199837421544));
#87781=CARTESIAN_POINT('Ctrl Pts',(15.1560811930195,-3.18456512528884,2.26397320547371));
#87782=CARTESIAN_POINT('Ctrl Pts',(12.4178232005272,-1.87034328920784,2.10594803673197));
#87783=CARTESIAN_POINT('Ctrl Pts',(12.0228292289231,1.14117296390725,1.94792286799024));
#87784=CARTESIAN_POINT('Ctrl Pts',(14.3295469221603,3.11709727220868,1.7898976992485));
#87785=CARTESIAN_POINT('Ctrl Pts',(17.2446848216638,2.2643389696831,1.63187253050676));
#87786=CARTESIAN_POINT('Ctrl Pts',(18.1228246665922,-0.643270672117315,
1.47384736176503));
#87787=CARTESIAN_POINT('Ctrl Pts',(16.1670753543694,-2.96709319012346,1.31582219302329));
#87788=CARTESIAN_POINT('Ctrl Pts',(13.1522330237942,-2.5984160783092,1.15779702428156));
#87789=CARTESIAN_POINT('Ctrl Pts',(11.8141950672532,0.128392194538437,0.999771855539822));
#87790=CARTESIAN_POINT('Ctrl Pts',(13.3671997073883,2.73843337695631,0.841746686798087));
#87791=CARTESIAN_POINT('Ctrl Pts',(16.4019309866401,2.86390715497503,0.683721518056352));
#87792=CARTESIAN_POINT('Ctrl Pts',(18.1644448607113,0.389486402064242,0.525696349314615));
#87793=CARTESIAN_POINT('Ctrl Pts',(17.0552962807149,-2.43649604452279,0.367671180572879));
#87794=CARTESIAN_POINT('Ctrl Pts',(14.0810320282566,-3.05512434484625,0.209646011831144));
#87795=CARTESIAN_POINT('Ctrl Pts',(11.9405826979638,-0.893790468169929,
0.051620843089408));
#87796=CARTESIAN_POINT('Ctrl Pts',(12.365359278395,1.07609660228605,-0.0537292694050819));
#87797=CARTESIAN_POINT('Ctrl Pts',(12.9464556006651,1.75575231790353,-0.106404325652328));
#87798=CARTESIAN_POINT('Ctrl Pts',(14.3507067397847,-2.42869513032583,6.32303370225465));
#87799=CARTESIAN_POINT('Ctrl Pts',(13.5468884598619,-2.2138003973168,6.27035864600741));
#87800=CARTESIAN_POINT('Ctrl Pts',(12.1829006599078,-0.927143859440181,
6.16500853351291));
#87801=CARTESIAN_POINT('Ctrl Pts',(12.6850654964508,1.85836265822507,6.00698336477119));
#87802=CARTESIAN_POINT('Ctrl Pts',(15.2918392215932,2.95162409967596,5.84895819602944));
#87803=CARTESIAN_POINT('Ctrl Pts',(17.6318342937641,1.36920914243917,5.69093302728772));
#87804=CARTESIAN_POINT('Ctrl Pts',(17.5844943450677,-1.45718037128031,5.53290785854596));
#87805=CARTESIAN_POINT('Ctrl Pts',(15.1912788689212,-2.96047106364502,5.37488268980425));
#87806=CARTESIAN_POINT('Ctrl Pts',(12.6247430569797,-1.77758524761693,5.21685752106249));
#87807=CARTESIAN_POINT('Ctrl Pts',(12.2135627329378,1.01861205475188,5.05883235232077));
#87808=CARTESIAN_POINT('Ctrl Pts',(14.3310765094832,2.89034306322065,4.90080718357903));
#87809=CARTESIAN_POINT('Ctrl Pts',(17.0555872814102,2.13920782036547,4.7427820148373));
#87810=CARTESIAN_POINT('Ctrl Pts',(17.9147195229455,-0.553233957437266,
4.58475684609556));
#87811=CARTESIAN_POINT('Ctrl Pts',(16.1288038813074,-2.74361557920579,4.42673167735383));
#87812=CARTESIAN_POINT('Ctrl Pts',(13.3185303103786,-2.44423824712834,4.26870650861208));
#87813=CARTESIAN_POINT('Ctrl Pts',(12.0341480540722,0.0732307040071116,
4.11068133987036));
#87814=CARTESIAN_POINT('Ctrl Pts',(13.4412071383069,2.52424271309487,3.95265617112861));
#87815=CARTESIAN_POINT('Ctrl Pts',(16.2628330263819,2.68456543570688,3.79463100238688));
#87816=CARTESIAN_POINT('Ctrl Pts',(17.9384683096406,0.40870840614628,3.63660583364514));
#87817=CARTESIAN_POINT('Ctrl Pts',(16.9475133300087,-2.23804154000899,3.4785806649034));
#87818=CARTESIAN_POINT('Ctrl Pts',(14.18923641449,-2.85382213952302,3.32055549616167));
#87819=CARTESIAN_POINT('Ctrl Pts',(12.1667081232501,-0.879826986309144,
3.16253032741993));
#87820=CARTESIAN_POINT('Ctrl Pts',(12.7153248382468,1.89259023586425,3.0045051586782));
#87821=CARTESIAN_POINT('Ctrl Pts',(15.3372299062344,2.94752677607998,2.84647998993646));
#87822=CARTESIAN_POINT('Ctrl Pts',(17.6531068616151,1.32765302276885,2.68845482119473));
#87823=CARTESIAN_POINT('Ctrl Pts',(17.5613524460306,-1.49703456150004,2.53042965245299));
#87824=CARTESIAN_POINT('Ctrl Pts',(15.1452316123453,-2.96319831247482,2.37240448371126));
#87825=CARTESIAN_POINT('Ctrl Pts',(12.5973165460024,-1.74033121016063,2.21437931496952));
#87826=CARTESIAN_POINT('Ctrl Pts',(12.2297795593035,1.06184727517078,2.05635414622779));
#87827=CARTESIAN_POINT('Ctrl Pts',(14.3761517347936,2.90042031280201,1.89832897748605));
#87828=CARTESIAN_POINT('Ctrl Pts',(17.0886513586337,2.10693929935797,1.74030380874431));
#87829=CARTESIAN_POINT('Ctrl Pts',(17.9057495821698,-0.598555374153223,
1.58227864000258));
#87830=CARTESIAN_POINT('Ctrl Pts',(16.0859491279158,-2.76084337673324,1.42425347126084));
#87831=CARTESIAN_POINT('Ctrl Pts',(13.2806757688012,-2.41779390134308,1.26622830251911));
#87832=CARTESIAN_POINT('Ctrl Pts',(12.0356480620778,0.119467343019631,1.10820313377737));
#87833=CARTESIAN_POINT('Ctrl Pts',(13.4806995990586,2.54807825940933,0.950177965035635));
#87834=CARTESIAN_POINT('Ctrl Pts',(16.3044793779939,2.66483005208971,0.792152796293899));
#87835=CARTESIAN_POINT('Ctrl Pts',(17.94447665608,0.362412261618913,0.634127627552163));
#87836=CARTESIAN_POINT('Ctrl Pts',(16.9124276725532,-2.26712932015377,0.476102458810427));
#87837=CARTESIAN_POINT('Ctrl Pts',(14.1449117113466,-2.84275527328963,0.318077290068692));
#87838=CARTESIAN_POINT('Ctrl Pts',(12.1532501833424,-0.831660934158786,
0.160052121326955));
#87839=CARTESIAN_POINT('Ctrl Pts',(12.5484995178017,1.00129452861,0.0547020088324655));
#87840=CARTESIAN_POINT('Ctrl Pts',(13.0892024313212,1.63370573401717,0.00202695258522012));
#87841=CARTESIAN_POINT('Ctrl Pts',(13.0865340033349,1.6359872033749,-1.11022302462516E-15));
#87842=CARTESIAN_POINT('Ctrl Pts',(13.0246968436933,1.57787545757268,-1.42432143907935E-14));
#87843=CARTESIAN_POINT('Ctrl Pts',(12.9662508181783,1.51659301622886,-1.45896528824685E-14));
#87844=CARTESIAN_POINT('Ctrl Pts',(12.9111941550382,1.45252821261314,-9.15933995315754E-15));
#87845=CARTESIAN_POINT('Ctrl Pts',(12.8541852271874,1.38619172291679,-3.53647252279832E-15));
#87846=CARTESIAN_POINT('Ctrl Pts',(12.800809794498,1.31687166945573,-1.37441483129643E-14));
#87847=CARTESIAN_POINT('Ctrl Pts',(12.7510925676234,1.24494849184277,-1.2712053631958E-14));
#87848=CARTESIAN_POINT('Ctrl Pts',(12.7013753407488,1.17302531422982,-1.16799589509518E-14));
#87849=CARTESIAN_POINT('Ctrl Pts',(12.6553159499066,1.09849829006597,1.01924597636171E-14));
#87850=CARTESIAN_POINT('Ctrl Pts',(12.6129716803907,1.02170689819782,8.54871728961371E-15));
#87851=CARTESIAN_POINT('Ctrl Pts',(12.5833476634006,0.967983702039261,8.28664904516205E-15));
#87852=CARTESIAN_POINT('Ctrl Pts',(12.5555426419577,0.913151367850236,-1.61718727885097E-14));
#87853=CARTESIAN_POINT('Ctrl Pts',(12.5295872014039,0.85731712410759,2.27595720048157E-15));
#87854=CARTESIAN_POINT('Ctrl Pts',(12.5203776154169,0.837505853029321,9.14664374412348E-15));
#87855=CARTESIAN_POINT('Ctrl Pts',(12.5113986372893,0.817562575119292,6.86217500987582E-15));
#87856=CARTESIAN_POINT('Ctrl Pts',(12.5026676497318,0.797529280254451,3.94129173741931E-15));
#87857=CARTESIAN_POINT('Ctrl Pts',(12.4661263202705,0.713685016014067,-8.28332286359483E-15));
#87858=CARTESIAN_POINT('Ctrl Pts',(12.43387109168,0.628155083435122,3.282298611734E-15));
#87859=CARTESIAN_POINT('Ctrl Pts',(12.4059285496426,0.541340460493411,1.01030295240889E-14));
#87860=CARTESIAN_POINT('Ctrl Pts',(12.3776099242671,0.453357385048541,1.7015561792458E-14));
#87861=CARTESIAN_POINT('Ctrl Pts',(12.3537203794151,0.364054027731861,2.19382220206576E-16));
#87862=CARTESIAN_POINT('Ctrl Pts',(12.3343268282525,0.273810866462743,7.21644966006352E-16));
#87863=CARTESIAN_POINT('Ctrl Pts',(12.3149149474258,0.183482412571172,1.22438242153645E-15));
#87864=CARTESIAN_POINT('Ctrl Pts',(12.3000071430258,0.0922114838591795,
4.21376165523926E-15));
#87865=CARTESIAN_POINT('Ctrl Pts',(12.2897162151444,0.00035562118077955,
-6.02295990859147E-15));
#87866=CARTESIAN_POINT('Ctrl Pts',(12.2860706085107,-0.0321847236929611,
-9.6493637150612E-15));
#87867=CARTESIAN_POINT('Ctrl Pts',(12.2830048501706,-0.0647986307443293,
-1.48809799554544E-14));
#87868=CARTESIAN_POINT('Ctrl Pts',(12.2805254843104,-0.0974705972111431,
-1.60704782814491E-14));
#87869=CARTESIAN_POINT('Ctrl Pts',(12.2787625414514,-0.120701864082326,
-1.72889664486694E-14));
#87870=CARTESIAN_POINT('Ctrl Pts',(12.2772960875482,-0.14396248857046,6.72941439601323E-15));
#87871=CARTESIAN_POINT('Ctrl Pts',(12.2761287376726,-0.167246925725108,
1.13242748511766E-14));
#87872=CARTESIAN_POINT('Ctrl Pts',(12.2754686811477,-0.180412682618434,
1.4340930014615E-14));
#87873=CARTESIAN_POINT('Ctrl Pts',(12.2749044797864,-0.193582396115722,
1.77390633662612E-15));
#87874=CARTESIAN_POINT('Ctrl Pts',(12.2744366510455,-0.206746783659478,
-2.77555756156289E-16));
#87875=CARTESIAN_POINT('Ctrl Pts',(12.2709697976906,-0.304301715917482,
-1.83947143932132E-14));
#87876=CARTESIAN_POINT('Ctrl Pts',(12.2727842857417,-0.401695668560479,
-7.28963219131405E-15));
#87877=CARTESIAN_POINT('Ctrl Pts',(12.2799462946648,-0.498500550756148,
2.16493489801906E-15));
#87878=CARTESIAN_POINT('Ctrl Pts',(12.2871083035879,-0.595305432951817,
1.15216481752733E-14));
#87879=CARTESIAN_POINT('Ctrl Pts',(12.2996173861023,-0.691522324483779,
-1.87906254926288E-14));
#87880=CARTESIAN_POINT('Ctrl Pts',(12.3175936746857,-0.786742501729336,
-1.97064586870965E-14));
#87881=CARTESIAN_POINT('Ctrl Pts',(12.3346924509195,-0.877314506963681,
-2.23083733320138E-14));
#87882=CARTESIAN_POINT('Ctrl Pts',(12.3567376278471,-0.966985711385258,
-1.66241219421888E-14));
#87883=CARTESIAN_POINT('Ctrl Pts',(12.3834540669815,-1.05551643358463,-6.52256026967279E-15));
#87884=CARTESIAN_POINT('Ctrl Pts',(12.3924682953621,-1.08538703664647,-2.5035240808304E-15));
#87885=CARTESIAN_POINT('Ctrl Pts',(12.4020147482449,-1.11512776886543,-9.97226500510694E-15));
#87886=CARTESIAN_POINT('Ctrl Pts',(12.4120841660463,-1.14472924022538,-4.16333634234434E-16));
#87887=CARTESIAN_POINT('Ctrl Pts',(12.4191312473773,-1.16544582784787,6.94088720832354E-15));
#87888=CARTESIAN_POINT('Ctrl Pts',(12.4264344851179,-1.18609420448,-2.1092073521417E-14));
#87889=CARTESIAN_POINT('Ctrl Pts',(12.4339908862363,-1.20667110461397,-8.79851747015437E-15));
#87890=CARTESIAN_POINT('Ctrl Pts',(12.4399883408572,-1.22300282428556,6.32926458462707E-16));
#87891=CARTESIAN_POINT('Ctrl Pts',(12.4461461531738,-1.23929147885018,1.7986801302824E-14));
#87892=CARTESIAN_POINT('Ctrl Pts',(12.4524542218356,-1.25551398610641,1.68476343986868E-14));
#87893=CARTESIAN_POINT('Ctrl Pts',(12.4867496980242,-1.34371191817618,1.40459420071657E-14));
#87894=CARTESIAN_POINT('Ctrl Pts',(12.5255315419816,-1.43009348828233,9.21519657422252E-15));
#87895=CARTESIAN_POINT('Ctrl Pts',(12.5684561946922,-1.51441605785902,1.2712053631958E-14));
#87896=CARTESIAN_POINT('Ctrl Pts',(12.6122200752026,-1.60038723354108,1.62772783867871E-14));
#87897=CARTESIAN_POINT('Ctrl Pts',(12.6602906227897,-1.68421882699259,-8.03770240444636E-15));
#87898=CARTESIAN_POINT('Ctrl Pts',(12.712359022737,-1.76565063551856,-6.99440505513849E-15));
#87899=CARTESIAN_POINT('Ctrl Pts',(12.7652941152924,-1.84843789853507,-5.93374173910713E-15));
#87900=CARTESIAN_POINT('Ctrl Pts',(12.8223616208756,-1.92874565038163,9.00741210667174E-15));
#87901=CARTESIAN_POINT('Ctrl Pts',(12.8832886862843,-2.00628553627795,-4.12170297892089E-15));
#87902=CARTESIAN_POINT('Ctrl Pts',(12.9249302016807,-2.05928133265722,-1.30949933271466E-14));
#87903=CARTESIAN_POINT('Ctrl Pts',(12.9683756920542,-2.11098388168042,-1.09972078411733E-14));
#87904=CARTESIAN_POINT('Ctrl Pts',(13.0135501530493,-2.16129409957465,-1.51545442861334E-14));
#87905=CARTESIAN_POINT('Ctrl Pts',(13.0249459289848,-2.1739854290949,-1.58022044252471E-14));
#87906=CARTESIAN_POINT('Ctrl Pts',(13.0364525536874,-2.18658884793829,-6.82249416347656E-15));
#87907=CARTESIAN_POINT('Ctrl Pts',(13.0480570543102,-2.19909025794491,-8.09075029195583E-15));
#87908=CARTESIAN_POINT('Ctrl Pts',(13.1169652321276,-2.27332433416292,-1.62663069842411E-14));
#87909=CARTESIAN_POINT('Ctrl Pts',(13.1894126660034,-2.3440672132455,-1.00541840446858E-14));
#87910=CARTESIAN_POINT('Ctrl Pts',(13.2650848374145,-2.41102556089288,-1.13867248963118E-14));
#87911=CARTESIAN_POINT('Ctrl Pts',(13.3278852605644,-2.46659437155688,-1.24926021003911E-14));
#87912=CARTESIAN_POINT('Ctrl Pts',(13.3929077805362,-2.5195566145235,1.16609985742211E-14));
#87913=CARTESIAN_POINT('Ctrl Pts',(13.4599961723147,-2.56973093141732,1.08524300657109E-14));
#87914=CARTESIAN_POINT('Ctrl Pts',(13.4819381207051,-2.58614095769194,9.9633548728848E-15));
#87915=CARTESIAN_POINT('Ctrl Pts',(13.504101206195,-2.60225264132935,-1.12667630852908E-14));
#87916=CARTESIAN_POINT('Ctrl Pts',(13.5264803918495,-2.61805924925994,-1.21430643318376E-15));
#87917=CARTESIAN_POINT('Ctrl Pts',(13.5510376032739,-2.635404215196,7.9186405249631E-15));
#87918=CARTESIAN_POINT('Ctrl Pts',(13.5758604919219,-2.65238520209721,8.64516985986044E-15));
#87919=CARTESIAN_POINT('Ctrl Pts',(13.6009083282656,-2.66897104610506,4.15639744844043E-15));
#87920=CARTESIAN_POINT('Ctrl Pts',(13.6859725059094,-2.72529771487193,-1.10877828699206E-14));
#87921=CARTESIAN_POINT('Ctrl Pts',(13.7736934061109,-2.77711837429031,-5.52596575509762E-15));
#87922=CARTESIAN_POINT('Ctrl Pts',(13.863781021542,-2.82412395861086,-1.49186218934005E-16));
#87923=CARTESIAN_POINT('Ctrl Pts',(13.9456845295005,-2.86685926946434,4.73913392834114E-15));
#87924=CARTESIAN_POINT('Ctrl Pts',(14.0295451217468,-2.90561477915702,-2.80944019091112E-15));
#87925=CARTESIAN_POINT('Ctrl Pts',(14.1151705147995,-2.94013097355399,3.65939917257307E-15));
#87926=CARTESIAN_POINT('Ctrl Pts',(14.1446077022585,-2.9519973095626,5.89368974534453E-15));
#87927=CARTESIAN_POINT('Ctrl Pts',(14.1742536602921,-2.96336232955947,-4.71883449063881E-15));
#87928=CARTESIAN_POINT('Ctrl Pts',(14.204096742977,-2.97422942397538,-3.61516372393567E-15));
#87929=CARTESIAN_POINT('Ctrl Pts',(14.2062007174671,-2.96922295374569,6.));
#87930=CARTESIAN_POINT('Ctrl Pts',(14.112236572373,-2.93485044973517,6.));
#87931=CARTESIAN_POINT('Ctrl Pts',(14.0203776766673,-2.89562046290185,6.00000000000001));
#87932=CARTESIAN_POINT('Ctrl Pts',(13.9308389508323,-2.8518698079655,6.00000000000001));
#87933=CARTESIAN_POINT('Ctrl Pts',(13.8399807998063,-2.80747445191565,6.00000000000001));
#87934=CARTESIAN_POINT('Ctrl Pts',(13.7515110537651,-2.75842352890383,6.));
#87935=CARTESIAN_POINT('Ctrl Pts',(13.6656836450528,-2.70502293578984,6.));
#87936=CARTESIAN_POINT('Ctrl Pts',(13.579785175186,-2.65157812943612,6.));
#87937=CARTESIAN_POINT('Ctrl Pts',(13.4965328335216,-2.59377566615863,6.00000000000001));
#87938=CARTESIAN_POINT('Ctrl Pts',(13.416219602925,-2.53188766444664,6.00000000000001));
#87939=CARTESIAN_POINT('Ctrl Pts',(13.352988970228,-2.48316322047234,6.00000000000001));
#87940=CARTESIAN_POINT('Ctrl Pts',(13.2915807800382,-2.43190558434592,6.00000000000001));
#87941=CARTESIAN_POINT('Ctrl Pts',(13.2321583210611,-2.37823724421546,6.));
#87942=CARTESIAN_POINT('Ctrl Pts',(13.2181172434773,-2.36555582139089,6.));
#87943=CARTESIAN_POINT('Ctrl Pts',(13.2041844800433,-2.35273716244636,5.99999999999999));
#87944=CARTESIAN_POINT('Ctrl Pts',(13.1903814772932,-2.33980114775681,5.99999999999999));
#87945=CARTESIAN_POINT('Ctrl Pts',(13.1179418149603,-2.27191153322796,6.));
#87946=CARTESIAN_POINT('Ctrl Pts',(13.0489682803957,-2.20070050515602,6.));
#87947=CARTESIAN_POINT('Ctrl Pts',(12.9837009998789,-2.12645785153675,6.));
#87948=CARTESIAN_POINT('Ctrl Pts',(12.9187891629334,-2.05261952109033,6.00000000000001));
#87949=CARTESIAN_POINT('Ctrl Pts',(12.8575428342958,-1.97578170012202,6.));
#87950=CARTESIAN_POINT('Ctrl Pts',(12.8002418733548,-1.8962026816294,6.));
#87951=CARTESIAN_POINT('Ctrl Pts',(12.7442407816496,-1.81842890891738,6.));
#87952=CARTESIAN_POINT('Ctrl Pts',(12.6920077941674,-1.73803615732598,6.00000000000001));
#87953=CARTESIAN_POINT('Ctrl Pts',(12.6438514592926,-1.6552512354046,5.99999999999999));
#87954=CARTESIAN_POINT('Ctrl Pts',(12.6245372121835,-1.62204836722422,5.99999999999999));
#87955=CARTESIAN_POINT('Ctrl Pts',(12.6058793011271,-1.58846059039376,5.99999999999999));
#87956=CARTESIAN_POINT('Ctrl Pts',(12.5879000034355,-1.55450226629581,6.));
#87957=CARTESIAN_POINT('Ctrl Pts',(12.5746716428088,-1.52951725491477,6.00000000000001));
#87958=CARTESIAN_POINT('Ctrl Pts',(12.5618106681902,-1.50433165036472,6.));
#87959=CARTESIAN_POINT('Ctrl Pts',(12.5493264552966,-1.47895116667682,6.));
#87960=CARTESIAN_POINT('Ctrl Pts',(12.5425330890363,-1.46514021014923,6.));
#87961=CARTESIAN_POINT('Ctrl Pts',(12.5358504386754,-1.45126959011197,6.));
#87962=CARTESIAN_POINT('Ctrl Pts',(12.5292876124697,-1.43735666935141,6.));
#87963=CARTESIAN_POINT('Ctrl Pts',(12.4893045010192,-1.3525941228605,6.00000000000002));
#87964=CARTESIAN_POINT('Ctrl Pts',(12.4537027965796,-1.2661394597289,5.99999999999999));
#87965=CARTESIAN_POINT('Ctrl Pts',(12.4227270631163,-1.17822295375644,5.99999999999999));
#87966=CARTESIAN_POINT('Ctrl Pts',(12.3918924146296,-1.09070688053558,6.));
#87967=CARTESIAN_POINT('Ctrl Pts',(12.3656413201946,-1.00174159141967,5.99999999999999));
#87968=CARTESIAN_POINT('Ctrl Pts',(12.3442654767827,-0.911544935711397,
6.00000000000001));
#87969=CARTESIAN_POINT('Ctrl Pts',(12.3412853594997,-0.898970151766612,
6.00000000000001));
#87970=CARTESIAN_POINT('Ctrl Pts',(12.338400086203,-0.886371428596121,6.00000000000002));
#87971=CARTESIAN_POINT('Ctrl Pts',(12.3356105320368,-0.873749353237649,
6.00000000000002));
#87972=CARTESIAN_POINT('Ctrl Pts',(12.3150423389811,-0.780683125706667,
6.00000000000001));
#87973=CARTESIAN_POINT('Ctrl Pts',(12.2996737954968,-0.686346358438301,
6.00000000000002));
#87974=CARTESIAN_POINT('Ctrl Pts',(12.2894275798084,-0.591148428203356,
6.));
#87975=CARTESIAN_POINT('Ctrl Pts',(12.2835915289072,-0.536925485466267,
5.99999999999998));
#87976=CARTESIAN_POINT('Ctrl Pts',(12.2794182200608,-0.482423351119525,
6.));
#87977=CARTESIAN_POINT('Ctrl Pts',(12.2769004062244,-0.427720434386167,
6.00000000000001));
#87978=CARTESIAN_POINT('Ctrl Pts',(12.2763256322878,-0.415232691908223,
6.00000000000001));
#87979=CARTESIAN_POINT('Ctrl Pts',(12.2758372671371,-0.402736071144333,
5.99999999999998));
#87980=CARTESIAN_POINT('Ctrl Pts',(12.275435366957,-0.390240948305382,5.99999999999999));
#87981=CARTESIAN_POINT('Ctrl Pts',(12.2724465583895,-0.297318546064596,
5.99999999999999));
#87982=CARTESIAN_POINT('Ctrl Pts',(12.2742281667087,-0.204333268112907,
6.));
#87983=CARTESIAN_POINT('Ctrl Pts',(12.280645798089,-0.111657463647094,6.));
#87984=CARTESIAN_POINT('Ctrl Pts',(12.2870860503062,-0.0186549959419595,
6.));
#87985=CARTESIAN_POINT('Ctrl Pts',(12.2981954251014,0.0740367887701639,
6.00000000000001));
#87986=CARTESIAN_POINT('Ctrl Pts',(12.3138887533189,0.16602968371911,6.00000000000002));
#87987=CARTESIAN_POINT('Ctrl Pts',(12.3294516393369,0.25725793808997,6.00000000000002));
#87988=CARTESIAN_POINT('Ctrl Pts',(12.3495230165553,0.347799756950362,6.00000000000002));
#87989=CARTESIAN_POINT('Ctrl Pts',(12.3740635534643,0.437251017449185,6.00000000000001));
#87990=CARTESIAN_POINT('Ctrl Pts',(12.3831172052085,0.470251948261792,6.00000000000001));
#87991=CARTESIAN_POINT('Ctrl Pts',(12.3927795390774,0.503104129077211,6.00000000000001));
#87992=CARTESIAN_POINT('Ctrl Pts',(12.4030499280732,0.535786015862936,6.00000000000002));
#87993=CARTESIAN_POINT('Ctrl Pts',(12.4093064823122,0.555695290710277,6.00000000000002));
#87994=CARTESIAN_POINT('Ctrl Pts',(12.4157887023811,0.575541354183405,5.99999999999998));
#87995=CARTESIAN_POINT('Ctrl Pts',(12.422496569579,0.595319189801257,5.99999999999999));
#87996=CARTESIAN_POINT('Ctrl Pts',(12.4279638159807,0.611439112487062,6.00000000000001));
#87997=CARTESIAN_POINT('Ctrl Pts',(12.4335814641443,0.627514847993582,5.99999999999999));
#87998=CARTESIAN_POINT('Ctrl Pts',(12.4393433186991,0.643527071723061,5.99999999999999));
#87999=CARTESIAN_POINT('Ctrl Pts',(12.4699004093487,0.728445385323959,5.99999999999999));
#88000=CARTESIAN_POINT('Ctrl Pts',(12.5045458819893,0.81168828046424,5.99999999999999));
#88001=CARTESIAN_POINT('Ctrl Pts',(12.5432205607682,0.89288298252984,5.99999999999999));
#88002=CARTESIAN_POINT('Ctrl Pts',(12.5747843101636,0.959148800608798,5.99999999999999));
#88003=CARTESIAN_POINT('Ctrl Pts',(12.6090326915418,1.02405010401912,5.99999999999999));
#88004=CARTESIAN_POINT('Ctrl Pts',(12.6459520793395,1.087366283338,6.00000000000001));
#88005=CARTESIAN_POINT('Ctrl Pts',(12.6596302052844,1.11082405787692,6.00000000000002));
#88006=CARTESIAN_POINT('Ctrl Pts',(12.6736751071307,1.1340640732078,6.00000000000002));
#88007=CARTESIAN_POINT('Ctrl Pts',(12.6880866137171,1.15707441161647,6.));
#88008=CARTESIAN_POINT('Ctrl Pts',(12.6977797682187,1.1725511255875,5.99999999999999));
#88009=CARTESIAN_POINT('Ctrl Pts',(12.7076392245588,1.18792442723443,6.));
#88010=CARTESIAN_POINT('Ctrl Pts',(12.7176559765905,1.20317739777071,6.));
#88011=CARTESIAN_POINT('Ctrl Pts',(12.7648369644737,1.27502206516142,5.99999999999999));
#88012=CARTESIAN_POINT('Ctrl Pts',(12.8155498102687,1.34427270741682,6.00000000000001));
#88013=CARTESIAN_POINT('Ctrl Pts',(12.8697611773098,1.41057678007138,6.));
#88014=CARTESIAN_POINT('Ctrl Pts',(12.9190744293929,1.47089013550598,5.99999999999999));
#88015=CARTESIAN_POINT('Ctrl Pts',(12.971283147028,1.52876530435445,6.00000000000001));
#88016=CARTESIAN_POINT('Ctrl Pts',(13.0263834616836,1.58390596072205,6.00000000000001));
#88017=CARTESIAN_POINT('Ctrl Pts',(13.0449113026906,1.60244736689347,6.00000000000001));
#88018=CARTESIAN_POINT('Ctrl Pts',(13.0637662565083,1.62067930192608,5.99999999999999));
#88019=CARTESIAN_POINT('Ctrl Pts',(13.0829386709519,1.63859769523264,5.99999999999999));
#88020=CARTESIAN_POINT('Origin',(0.,0.,6.));
#88021=CARTESIAN_POINT('',(-25.,30.,6.));
#88022=CARTESIAN_POINT('',(-25.,-30.,6.));
#88023=CARTESIAN_POINT('',(-25.,30.,6.));
#88024=CARTESIAN_POINT('',(25.,-30.,6.));
#88025=CARTESIAN_POINT('',(-25.,-30.,6.));
#88026=CARTESIAN_POINT('',(25.,30.,6.));
#88027=CARTESIAN_POINT('',(25.,-30.,6.));
#88028=CARTESIAN_POINT('',(25.,30.,6.));
#88029=CARTESIAN_POINT('Ctrl Pts',(-13.0865340033349,1.63598720337492,6.));
#88030=CARTESIAN_POINT('Ctrl Pts',(-13.0246970130234,1.57787561670136,5.99999999999999));
#88031=CARTESIAN_POINT('Ctrl Pts',(-12.9662511655096,1.51659332338802,5.99999999999999));
#88032=CARTESIAN_POINT('Ctrl Pts',(-12.9111946833098,1.45252865944064,5.99999999999999));
#88033=CARTESIAN_POINT('Ctrl Pts',(-12.854185836343,1.38619219047224,6.));
#88034=CARTESIAN_POINT('Ctrl Pts',(-12.800810501265,1.31687213764253,6.));
#88035=CARTESIAN_POINT('Ctrl Pts',(-12.7510933826585,1.24494894576893,6.));
#88036=CARTESIAN_POINT('Ctrl Pts',(-12.701376264052,1.17302575389534,5.99999999999999));
#88037=CARTESIAN_POINT('Ctrl Pts',(-12.6553169921464,1.09849870057196,5.99999999999999));
#88038=CARTESIAN_POINT('Ctrl Pts',(-12.612972846328,1.02170726964558,6.));
#88039=CARTESIAN_POINT('Ctrl Pts',(-12.5941124949904,0.987503878857991,
6.));
#88040=CARTESIAN_POINT('Ctrl Pts',(-12.575989640936,0.952850788172522,6.00000000000002));
#88041=CARTESIAN_POINT('Ctrl Pts',(-12.5586117249717,0.917775962781449,
6.));
#88042=CARTESIAN_POINT('Ctrl Pts',(-12.5486939802334,0.89775842065026,5.99999999999999));
#88043=CARTESIAN_POINT('Ctrl Pts',(-12.5390188969959,0.877603494962885,
5.99999999999999));
#88044=CARTESIAN_POINT('Ctrl Pts',(-12.5295880909113,0.857316236876344,
5.99999999999999));
#88045=CARTESIAN_POINT('Ctrl Pts',(-12.5210550868119,0.838960302625967,
5.99999999999999));
#88046=CARTESIAN_POINT('Ctrl Pts',(-12.5127196692249,0.820490261091803,
6.00000000000002));
#88047=CARTESIAN_POINT('Ctrl Pts',(-12.5045967742098,0.80194176932807,6.00000000000001));
#88048=CARTESIAN_POINT('Ctrl Pts',(-12.4680063703819,0.718388208340872,
5.99999999999998));
#88049=CARTESIAN_POINT('Ctrl Pts',(-12.4356782866175,0.633150881056809,
6.00000000000001));
#88050=CARTESIAN_POINT('Ctrl Pts',(-12.4076382326647,0.546628236228551,
6.));
#88051=CARTESIAN_POINT('Ctrl Pts',(-12.3790534776866,0.458424818123778,
5.99999999999999));
#88052=CARTESIAN_POINT('Ctrl Pts',(-12.3549244489257,0.368884915467499,
6.));
#88053=CARTESIAN_POINT('Ctrl Pts',(-12.3353178885102,0.278393148285168,
6.00000000000001));
#88054=CARTESIAN_POINT('Ctrl Pts',(-12.3164053528586,0.191104570546898,
6.00000000000002));
#88055=CARTESIAN_POINT('Ctrl Pts',(-12.301700662964,0.102929389819606,6.00000000000001));
#88056=CARTESIAN_POINT('Ctrl Pts',(-12.2913042242818,0.0141911085737902,
6.00000000000001));
#88057=CARTESIAN_POINT('Ctrl Pts',(-12.2869540962369,-0.0229391913018656,
6.));
#88058=CARTESIAN_POINT('Ctrl Pts',(-12.2833587635632,-0.0601682677303705,
6.00000000000001));
#88059=CARTESIAN_POINT('Ctrl Pts',(-12.2805278793397,-0.0974730292652828,
6.00000000000001));
#88060=CARTESIAN_POINT('Ctrl Pts',(-12.2787649629962,-0.120704348035766,
6.));
#88061=CARTESIAN_POINT('Ctrl Pts',(-12.2772985351823,-0.143965023569731,
5.99999999999998));
#88062=CARTESIAN_POINT('Ctrl Pts',(-12.2761312108751,-0.167249510799076,
6.));
#88063=CARTESIAN_POINT('Ctrl Pts',(-12.2754711705252,-0.180415261740913,
6.00000000000002));
#88064=CARTESIAN_POINT('Ctrl Pts',(-12.2749069846676,-0.193584968987863,
6.00000000000001));
#88065=CARTESIAN_POINT('Ctrl Pts',(-12.2744391707337,-0.206749349931413,
6.00000000000001));
#88066=CARTESIAN_POINT('Ctrl Pts',(-12.2709724203682,-0.304304422879126,
6.00000000000002));
#88067=CARTESIAN_POINT('Ctrl Pts',(-12.2727869938187,-0.401698496843062,
5.99999999999999));
#88068=CARTESIAN_POINT('Ctrl Pts',(-12.2799490637078,-0.498503473694779,
5.99999999999999));
#88069=CARTESIAN_POINT('Ctrl Pts',(-12.2871111335968,-0.595308450546486,
6.));
#88070=CARTESIAN_POINT('Ctrl Pts',(-12.299620252658,-0.691525410085519,
6.));
#88071=CARTESIAN_POINT('Ctrl Pts',(-12.3175965465156,-0.78674562136694,
5.99999999999999));
#88072=CARTESIAN_POINT('Ctrl Pts',(-12.3347011817646,-0.877348667534142,
5.99999999999999));
#88073=CARTESIAN_POINT('Ctrl Pts',(-12.3567555739435,-0.967050265529378,
6.00000000000002));
#88074=CARTESIAN_POINT('Ctrl Pts',(-12.3834843158721,-1.05561049186739,
6.00000000000002));
#88075=CARTESIAN_POINT('Ctrl Pts',(-12.3924905257796,-1.08545072864266,
6.00000000000001));
#88076=CARTESIAN_POINT('Ctrl Pts',(-12.4020278760569,-1.11516134375352,
6.));
#88077=CARTESIAN_POINT('Ctrl Pts',(-12.4120871355902,-1.14473297565289,
5.99999999999999));
#88078=CARTESIAN_POINT('Ctrl Pts',(-12.4191345524566,-1.16545056592121,
5.99999999999999));
#88079=CARTESIAN_POINT('Ctrl Pts',(-12.4264381495643,-1.18609993714932,
6.00000000000002));
#88080=CARTESIAN_POINT('Ctrl Pts',(-12.433994933511,-1.20667782341152,6.00000000000001));
#88081=CARTESIAN_POINT('Ctrl Pts',(-12.43999210244,-1.22300872038934,6.));
#88082=CARTESIAN_POINT('Ctrl Pts',(-12.4461496119182,-1.23929655429101,
5.99999999999999));
#88083=CARTESIAN_POINT('Ctrl Pts',(-12.452457362016,-1.25551824623984,5.99999999999999));
#88084=CARTESIAN_POINT('Ctrl Pts',(-12.4867528525614,-1.34371623668614,
6.00000000000001));
#88085=CARTESIAN_POINT('Ctrl Pts',(-12.525534703178,-1.43009783582075,6.00000000000002));
#88086=CARTESIAN_POINT('Ctrl Pts',(-12.5684593590188,-1.51442040944555,
6.00000000000001));
#88087=CARTESIAN_POINT('Ctrl Pts',(-12.6122232164358,-1.60039153762029,
5.99999999999999));
#88088=CARTESIAN_POINT('Ctrl Pts',(-12.6602937320879,-1.68422306016549,
5.99999999999999));
#88089=CARTESIAN_POINT('Ctrl Pts',(-12.7123620962136,-1.76565477904875,
6.00000000000001));
#88090=CARTESIAN_POINT('Ctrl Pts',(-12.765297101908,-1.84844187204008,6.00000000000002));
#88091=CARTESIAN_POINT('Ctrl Pts',(-12.8223645087377,-1.92874943921375,
5.99999999999999));
#88092=CARTESIAN_POINT('Ctrl Pts',(-12.883291469427,-2.00628913114377,5.99999999999999));
#88093=CARTESIAN_POINT('Ctrl Pts',(-12.9249334864398,-2.05928552443159,
6.));
#88094=CARTESIAN_POINT('Ctrl Pts',(-12.9683795252804,-2.11098863042859,
6.00000000000001));
#88095=CARTESIAN_POINT('Ctrl Pts',(-13.0135545804225,-2.1612993628776,6.));
#88096=CARTESIAN_POINT('Ctrl Pts',(-13.0249491514721,-2.17398931341881,
6.));
#88097=CARTESIAN_POINT('Ctrl Pts',(-13.0364545470035,-2.18659137056383,
6.));
#88098=CARTESIAN_POINT('Ctrl Pts',(-13.04805779778,-2.19909144013573,5.99999999999999));
#88099=CARTESIAN_POINT('Ctrl Pts',(-13.1169657930863,-2.27332535543923,
5.99999999999999));
#88100=CARTESIAN_POINT('Ctrl Pts',(-13.1894130456957,-2.34406807252095,
6.00000000000002));
#88101=CARTESIAN_POINT('Ctrl Pts',(-13.2650850429559,-2.4110262629765,6.00000000000001));
#88102=CARTESIAN_POINT('Ctrl Pts',(-13.3278853347565,-2.46659495484805,
6.));
#88103=CARTESIAN_POINT('Ctrl Pts',(-13.3929077292049,-2.51955708123384,
6.00000000000001));
#88104=CARTESIAN_POINT('Ctrl Pts',(-13.459996004521,-2.56973128696733,5.99999999999999));
#88105=CARTESIAN_POINT('Ctrl Pts',(-13.4864139606169,-2.58948883712003,
5.99999999999999));
#88106=CARTESIAN_POINT('Ctrl Pts',(-13.5131517477184,-2.60881342412512,
5.99999999999999));
#88107=CARTESIAN_POINT('Ctrl Pts',(-13.5402031725862,-2.62769502775298,
5.99999999999999));
#88108=CARTESIAN_POINT('Ctrl Pts',(-13.5584328350526,-2.64041913610002,
6.));
#88109=CARTESIAN_POINT('Ctrl Pts',(-13.5768038646028,-2.65294113604551,
6.));
#88110=CARTESIAN_POINT('Ctrl Pts',(-13.5952986555222,-2.66524780668941,
6.));
#88111=CARTESIAN_POINT('Ctrl Pts',(-13.6802589908623,-2.72178150146766,
6.00000000000001));
#88112=CARTESIAN_POINT('Ctrl Pts',(-13.7678837405493,-2.77381421749709,
5.99999999999999));
#88113=CARTESIAN_POINT('Ctrl Pts',(-13.8578818875583,-2.82103744760724,
6.));
#88114=CARTESIAN_POINT('Ctrl Pts',(-13.9416560498191,-2.86499486976769,
6.));
#88115=CARTESIAN_POINT('Ctrl Pts',(-14.027487492673,-2.90478531313897,6.00000000000001));
#88116=CARTESIAN_POINT('Ctrl Pts',(-14.1151694615309,-2.94013049350043,
6.00000000000001));
#88117=CARTESIAN_POINT('Ctrl Pts',(-14.1445077395108,-2.95195694699142,
6.00000000000001));
#88118=CARTESIAN_POINT('Ctrl Pts',(-14.1740533905285,-2.9632854491535,6.));
#88119=CARTESIAN_POINT('Ctrl Pts',(-14.2037948851047,-2.97411935705757,
6.00000000000001));
#88120=CARTESIAN_POINT('Ctrl Pts',(-15.7937992825329,-2.96922295374568,
6.));
#88121=CARTESIAN_POINT('Ctrl Pts',(-15.8877632500353,-2.934850514699,6.));
#88122=CARTESIAN_POINT('Ctrl Pts',(-15.9796219674832,-2.89562055829788,
5.99999999999999));
#88123=CARTESIAN_POINT('Ctrl Pts',(-16.069160517518,-2.85186990831237,5.99999999999999));
#88124=CARTESIAN_POINT('Ctrl Pts',(-16.1600185833041,-2.80747451177071,
6.));
#88125=CARTESIAN_POINT('Ctrl Pts',(-16.2484882417351,-2.75842351247667,
6.00000000000001));
#88126=CARTESIAN_POINT('Ctrl Pts',(-16.334315563103,-2.70502281756701,6.));
#88127=CARTESIAN_POINT('Ctrl Pts',(-16.4202140639116,-2.65157783569215,
6.));
#88128=CARTESIAN_POINT('Ctrl Pts',(-16.5034664294958,-2.59377515931806,
6.));
#88129=CARTESIAN_POINT('Ctrl Pts',(-16.5837796785328,-2.53188691831275,
6.));
#88130=CARTESIAN_POINT('Ctrl Pts',(-16.6470102644641,-2.4831623331671,6.));
#88131=CARTESIAN_POINT('Ctrl Pts',(-16.7084184080196,-2.43190454453287,
5.99999999999999));
#88132=CARTESIAN_POINT('Ctrl Pts',(-16.7678408217129,-2.37823604579948,
6.00000000000001));
#88133=CARTESIAN_POINT('Ctrl Pts',(-16.7818820741009,-2.36555441795637,
6.00000000000001));
#88134=CARTESIAN_POINT('Ctrl Pts',(-16.7958150096753,-2.35273554990402,
6.00000000000001));
#88135=CARTESIAN_POINT('Ctrl Pts',(-16.8096181812999,-2.3397993227231,6.00000000000001));
#88136=CARTESIAN_POINT('Ctrl Pts',(-16.8820533727342,-2.2719136137154,6.00000000000001));
#88137=CARTESIAN_POINT('Ctrl Pts',(-16.9510228592216,-2.20070688840159,
6.00000000000001));
#88138=CARTESIAN_POINT('Ctrl Pts',(-17.0162865616681,-2.12646889315391,
6.00000000000001));
#88139=CARTESIAN_POINT('Ctrl Pts',(-17.0807779367567,-2.05310942659178,
6.00000000000001));
#88140=CARTESIAN_POINT('Ctrl Pts',(-17.1416511471808,-1.97678920349332,
5.99999999999999));
#88141=CARTESIAN_POINT('Ctrl Pts',(-17.1986318998573,-1.89776160004079,
5.99999999999999));
#88142=CARTESIAN_POINT('Ctrl Pts',(-17.2542709860764,-1.82059477728679,
5.99999999999999));
#88143=CARTESIAN_POINT('Ctrl Pts',(-17.3061990346064,-1.74084585335279,
6.00000000000002));
#88144=CARTESIAN_POINT('Ctrl Pts',(-17.3541147728116,-1.65873676591806,
6.));
#88145=CARTESIAN_POINT('Ctrl Pts',(-17.3741535582349,-1.62439801948437,
5.99999999999999));
#88146=CARTESIAN_POINT('Ctrl Pts',(-17.3934900117363,-1.58964637356626,
6.));
#88147=CARTESIAN_POINT('Ctrl Pts',(-17.4120994581939,-1.55449775528887,
6.00000000000001));
#88148=CARTESIAN_POINT('Ctrl Pts',(-17.4253278876833,-1.52951254040944,
6.00000000000002));
#88149=CARTESIAN_POINT('Ctrl Pts',(-17.4381889272245,-1.50432673226678,
6.00000000000001));
#88150=CARTESIAN_POINT('Ctrl Pts',(-17.4506732009798,-1.47894604526973,
6.00000000000001));
#88151=CARTESIAN_POINT('Ctrl Pts',(-17.4574664323557,-1.46513531966157,
6.00000000000001));
#88152=CARTESIAN_POINT('Ctrl Pts',(-17.464148952056,-1.45126493367676,6.));
#88153=CARTESIAN_POINT('Ctrl Pts',(-17.4707116522414,-1.43735224943686,
6.));
#88154=CARTESIAN_POINT('Ctrl Pts',(-17.5106947798987,-1.35258948193268,
6.00000000000002));
#88155=CARTESIAN_POINT('Ctrl Pts',(-17.5462964993568,-1.26613462526213,
6.));
#88156=CARTESIAN_POINT('Ctrl Pts',(-17.5772722477121,-1.1782179632567,5.99999999999999));
#88157=CARTESIAN_POINT('Ctrl Pts',(-17.6081069075101,-1.09070174468405,
5.99999999999999));
#88158=CARTESIAN_POINT('Ctrl Pts',(-17.6343580141732,-1.00173634769329,
6.00000000000001));
#88159=CARTESIAN_POINT('Ctrl Pts',(-17.6557338718008,-0.911539631838522,
5.99999999999999));
#88160=CARTESIAN_POINT('Ctrl Pts',(-17.6587139661113,-0.898964944805013,
5.99999999999998));
#88161=CARTESIAN_POINT('Ctrl Pts',(-17.6615992180624,-0.886366319875325,
5.99999999999998));
#88162=CARTESIAN_POINT('Ctrl Pts',(-17.6643887525347,-0.873744344101168,
5.99999999999998));
#88163=CARTESIAN_POINT('Ctrl Pts',(-17.6849486211246,-0.780715860016505,
6.));
#88164=CARTESIAN_POINT('Ctrl Pts',(-17.7003130610805,-0.686417920490627,
6.00000000000002));
#88165=CARTESIAN_POINT('Ctrl Pts',(-17.7105593084943,-0.591259391971915,
5.99999999999999));
#88166=CARTESIAN_POINT('Ctrl Pts',(-17.7164019038377,-0.53699828025407,
5.99999999999998));
#88167=CARTESIAN_POINT('Ctrl Pts',(-17.7205793832134,-0.482457537922925,
6.00000000000001));
#88168=CARTESIAN_POINT('Ctrl Pts',(-17.72309901058,-0.427715739212653,6.00000000000002));
#88169=CARTESIAN_POINT('Ctrl Pts',(-17.7236737899306,-0.415227997600035,
6.00000000000002));
#88170=CARTESIAN_POINT('Ctrl Pts',(-17.7241621603287,-0.402731378403247,
6.00000000000002));
#88171=CARTESIAN_POINT('Ctrl Pts',(-17.7245640655875,-0.390236257730834,
6.00000000000002));
#88172=CARTESIAN_POINT('Ctrl Pts',(-17.7275529071898,-0.297314018776729,
6.));
#88173=CARTESIAN_POINT('Ctrl Pts',(-17.7257713377121,-0.204328938103657,
6.00000000000001));
#88174=CARTESIAN_POINT('Ctrl Pts',(-17.7193537491782,-0.111653355453281,
6.));
#88175=CARTESIAN_POINT('Ctrl Pts',(-17.7129135394428,-0.0186511028990985,
6.));
#88176=CARTESIAN_POINT('Ctrl Pts',(-17.7018042104191,0.0740404418833223,
5.99999999999997));
#88177=CARTESIAN_POINT('Ctrl Pts',(-17.6861109294909,0.166033081375381,
5.99999999999998));
#88178=CARTESIAN_POINT('Ctrl Pts',(-17.6705480842034,0.257261118556288,
5.99999999999999));
#88179=CARTESIAN_POINT('Ctrl Pts',(-17.6504767456414,0.347802704397206,
6.));
#88180=CARTESIAN_POINT('Ctrl Pts',(-17.6259362435908,0.437253724644228,
6.));
#88181=CARTESIAN_POINT('Ctrl Pts',(-17.6168825703273,0.470254692135947,
6.));
#88182=CARTESIAN_POINT('Ctrl Pts',(-17.6072202097986,0.503106907518295,
6.00000000000001));
#88183=CARTESIAN_POINT('Ctrl Pts',(-17.5969497889173,0.535788826950787,
5.99999999999999));
#88184=CARTESIAN_POINT('Ctrl Pts',(-17.5906928388196,0.555699319553684,
5.99999999999998));
#88185=CARTESIAN_POINT('Ctrl Pts',(-17.5842101937972,0.575546592464114,
5.99999999999998));
#88186=CARTESIAN_POINT('Ctrl Pts',(-17.5775018725303,0.595325628334281,
5.99999999999999));
#88187=CARTESIAN_POINT('Ctrl Pts',(-17.572035158038,0.611443869803769,5.99999999999999));
#88188=CARTESIAN_POINT('Ctrl Pts',(-17.5664180723908,0.627517931614629,
6.));
#88189=CARTESIAN_POINT('Ctrl Pts',(-17.5606568093946,0.643528494331941,
6.));
#88190=CARTESIAN_POINT('Ctrl Pts',(-17.5300997600929,0.728446602500721,
5.99999999999998));
#88191=CARTESIAN_POINT('Ctrl Pts',(-17.4954543212718,0.811689292699246,
5.99999999999999));
#88192=CARTESIAN_POINT('Ctrl Pts',(-17.4567796672896,0.892883798280689,
5.99999999999999));
#88193=CARTESIAN_POINT('Ctrl Pts',(-17.4252159774462,0.959149373464304,
5.99999999999999));
#88194=CARTESIAN_POINT('Ctrl Pts',(-17.3909676562918,1.02405044300496,5.99999999999999));
#88195=CARTESIAN_POINT('Ctrl Pts',(-17.3540483284449,1.08736640274463,5.99999999999999));
#88196=CARTESIAN_POINT('Ctrl Pts',(-17.3403702095884,1.11082412186727,6.));
#88197=CARTESIAN_POINT('Ctrl Pts',(-17.3263253139819,1.13406408326418,6.00000000000001));
#88198=CARTESIAN_POINT('Ctrl Pts',(-17.3119138127385,1.157074369458,5.99999999999999));
#88199=CARTESIAN_POINT('Ctrl Pts',(-17.3022206458985,1.17255107374768,5.99999999999998));
#88200=CARTESIAN_POINT('Ctrl Pts',(-17.2923611762558,1.18792436616809,6.));
#88201=CARTESIAN_POINT('Ctrl Pts',(-17.2823444099864,1.20317732794761,6.));
#88202=CARTESIAN_POINT('Ctrl Pts',(-17.2351633869987,1.27502190542827,6.));
#88203=CARTESIAN_POINT('Ctrl Pts',(-17.1844504900327,1.34427247178924,6.));
#88204=CARTESIAN_POINT('Ctrl Pts',(-17.1302390543522,1.41057648897033,6.00000000000001));
#88205=CARTESIAN_POINT('Ctrl Pts',(-17.0809259142552,1.4708895806124,6.00000000000001));
#88206=CARTESIAN_POINT('Ctrl Pts',(-17.0287173146208,1.52876451979022,5.99999999999998));
#88207=CARTESIAN_POINT('Ctrl Pts',(-16.9736171227159,1.58390498876622,6.));
#88208=CARTESIAN_POINT('Ctrl Pts',(-16.9550892876871,1.60244636724923,6.00000000000001));
#88209=CARTESIAN_POINT('Ctrl Pts',(-16.936234339139,1.62067827820074,6.));
#88210=CARTESIAN_POINT('Ctrl Pts',(-16.9170619292826,1.6385966508594,6.));
#88211=CARTESIAN_POINT('',(-11.,1.34711147906209E-15,6.));
#88212=CARTESIAN_POINT('Origin',(0.,0.,6.));
#88213=CARTESIAN_POINT('Ctrl Pts',(-13.0907445586006,1.63408170136227,5.99751915277646));
#88214=CARTESIAN_POINT('Ctrl Pts',(-12.5496079497899,1.00187089822864,5.9448169085008));
#88215=CARTESIAN_POINT('Ctrl Pts',(-12.1539631618182,-0.831013794683539,
5.83943960797791));
#88216=CARTESIAN_POINT('Ctrl Pts',(-14.1452240851043,-2.84170398134258,
5.68138725120779));
#88217=CARTESIAN_POINT('Ctrl Pts',(-16.911723975924,-2.26629529617324,5.52336208246603));
#88218=CARTESIAN_POINT('Ctrl Pts',(-17.9433901746218,0.362279851730001,
5.36533691372431));
#88219=CARTESIAN_POINT('Ctrl Pts',(-16.303998759699,2.66384669060504,5.20731174498257));
#88220=CARTESIAN_POINT('Ctrl Pts',(-13.4812596174396,2.54713914628003,5.04928657624084));
#88221=CARTESIAN_POINT('Ctrl Pts',(-12.0367412189483,0.119423028973387,
4.8912614074991));
#88222=CARTESIAN_POINT('Ctrl Pts',(-13.2813096887287,-2.41690222892453,
4.73323623875736));
#88223=CARTESIAN_POINT('Ctrl Pts',(-16.0855487290697,-2.75982544810006,
4.57521107001563));
#88224=CARTESIAN_POINT('Ctrl Pts',(-17.9046781218851,-0.59833461826069,
4.41718590127389));
#88225=CARTESIAN_POINT('Ctrl Pts',(-17.0878812104006,2.10616237353801,4.25916073253216));
#88226=CARTESIAN_POINT('Ctrl Pts',(-14.3763817648042,2.89935084640419,4.10113556379042));
#88227=CARTESIAN_POINT('Ctrl Pts',(-12.2308010336203,1.06145572840915,3.94311039504869));
#88228=CARTESIAN_POINT('Ctrl Pts',(-12.5982024944047,-1.73968948755044,
3.78508522630695));
#88229=CARTESIAN_POINT('Ctrl Pts',(-15.1451780611008,-2.96210568514241,
3.62706005756521));
#88230=CARTESIAN_POINT('Ctrl Pts',(-17.5604079898984,-1.49648255368145,
3.46903488882348));
#88231=CARTESIAN_POINT('Ctrl Pts',(-17.652128572941,1.32716347219163,3.31100972008174));
#88232=CARTESIAN_POINT('Ctrl Pts',(-15.3371055582946,2.946439925236,3.15298455134001));
#88233=CARTESIAN_POINT('Ctrl Pts',(-12.7161672740172,1.89189237470017,2.99495938259826));
#88234=CARTESIAN_POINT('Ctrl Pts',(-12.16775285229,-0.879502564808503,2.83693421385654));
#88235=CARTESIAN_POINT('Ctrl Pts',(-14.1895353699199,-2.8527698401918,2.6789090451148));
#88236=CARTESIAN_POINT('Ctrl Pts',(-16.9467952172,-2.23721629994614,2.52088387637306));
#88237=CARTESIAN_POINT('Ctrl Pts',(-17.9373847982726,0.408557702420045,
2.36285870763132));
#88238=CARTESIAN_POINT('Ctrl Pts',(-16.2623673783843,2.68357554583426,2.20483353888959));
#88239=CARTESIAN_POINT('Ctrl Pts',(-13.441781916094,2.52331194313473,2.04680837014785));
#88240=CARTESIAN_POINT('Ctrl Pts',(-12.0352416641978,0.0732036971019031,
1.88878320140612));
#88241=CARTESIAN_POINT('Ctrl Pts',(-13.3191503210149,-2.4433369672288,1.73075803266438));
#88242=CARTESIAN_POINT('Ctrl Pts',(-16.1283876593297,-2.74260393131891,
1.57273286392265));
#88243=CARTESIAN_POINT('Ctrl Pts',(-17.9136447592549,-0.553029935281315,
1.41470769518091));
#88244=CARTESIAN_POINT('Ctrl Pts',(-17.0548293342031,2.13841897542678,1.25668252643918));
#88245=CARTESIAN_POINT('Ctrl Pts',(-14.3313231370429,2.88927738372614,1.09865735769744));
#88246=CARTESIAN_POINT('Ctrl Pts',(-12.2145902278525,1.0182363043339,0.940632188955702));
#88247=CARTESIAN_POINT('Ctrl Pts',(-12.6256188283705,-1.77692951890069,
0.782607020213967));
#88248=CARTESIAN_POINT('Ctrl Pts',(-15.1912084285039,-2.9593799210309,0.62458185147223));
#88249=CARTESIAN_POINT('Ctrl Pts',(-17.5835412498342,-1.45664222331674,
0.466556682730496));
#88250=CARTESIAN_POINT('Ctrl Pts',(-17.6308639198215,1.36870283349263,0.308531513988758));
#88251=CARTESIAN_POINT('Ctrl Pts',(-15.2917317296307,2.95053817591071,0.150506345247024));
#88252=CARTESIAN_POINT('Ctrl Pts',(-12.685918419667,1.85767322794601,-0.00751882349471303));
#88253=CARTESIAN_POINT('Ctrl Pts',(-12.183941158064,-0.926794243668898,
-0.165543992236448));
#88254=CARTESIAN_POINT('Ctrl Pts',(-13.5474245306813,-2.21298369896996,
-0.270894104730938));
#88255=CARTESIAN_POINT('Ctrl Pts',(-14.3509462720988,-2.42779915465415,
-0.323569160978183));
#88256=CARTESIAN_POINT('Ctrl Pts',(-12.9478680952619,1.75636592233901,6.1060964911164));
#88257=CARTESIAN_POINT('Ctrl Pts',(-12.3662362844088,1.07684450708003,6.05339424684075));
#88258=CARTESIAN_POINT('Ctrl Pts',(-11.9409839715256,-0.893201550913282,
5.94801694631786));
#88259=CARTESIAN_POINT('Ctrl Pts',(-14.081258123809,-3.05435892834755,5.78996458954772));
#88260=CARTESIAN_POINT('Ctrl Pts',(-17.0547851685949,-2.4358903381866,5.631939420806));
#88261=CARTESIAN_POINT('Ctrl Pts',(-18.1636546658245,0.389390558255529,
5.47391425206424));
#88262=CARTESIAN_POINT('Ctrl Pts',(-16.4015816849294,2.8631919357605,5.31588908332252));
#88263=CARTESIAN_POINT('Ctrl Pts',(-13.3676068029002,2.73775074542011,5.15786391458077));
#88264=CARTESIAN_POINT('Ctrl Pts',(-11.8149898883439,0.128359884488338,
4.99983874583904));
#88265=CARTESIAN_POINT('Ctrl Pts',(-13.1526939006449,-2.5977677303218,4.84181357709731));
#88266=CARTESIAN_POINT('Ctrl Pts',(-16.1667842514772,-2.96635312947079,
4.68378840835557));
#88267=CARTESIAN_POINT('Ctrl Pts',(-18.1220456507098,-0.643110153422998,
4.52576323961383));
#88268=CARTESIAN_POINT('Ctrl Pts',(-17.2441248835859,2.26377409202425,4.36773807087211));
#88269=CARTESIAN_POINT('Ctrl Pts',(-14.3297141654948,3.11631971601164,4.20971290213036));
#88270=CARTESIAN_POINT('Ctrl Pts',(-12.0235718981058,1.14088828477496,4.05168773338863));
#88271=CARTESIAN_POINT('Ctrl Pts',(-12.4184673338734,-1.86987671965101,
3.89366256464689));
#88272=CARTESIAN_POINT('Ctrl Pts',(-15.15604225846,-3.18377072542555,3.73563739590515));
#88273=CARTESIAN_POINT('Ctrl Pts',(-17.7520125444114,-1.60846973469552,
3.57761222716342));
#88274=CARTESIAN_POINT('Ctrl Pts',(-17.8505969091337,1.42647989631562,3.41958705842168));
#88275=CARTESIAN_POINT('Ctrl Pts',(-15.3623323817446,3.1669326402648,3.26156188967995));
#88276=CARTESIAN_POINT('Ctrl Pts',(-12.5452598429473,2.03346949720218,3.10353672093821));
#88277=CARTESIAN_POINT('Ctrl Pts',(-11.9558055942168,-0.945318910401867,
2.94551155219648));
#88278=CARTESIAN_POINT('Ctrl Pts',(-14.1288853817119,-3.0662528852825,2.78748638345474));
#88279=CARTESIAN_POINT('Ctrl Pts',(-17.0924809172101,-2.40463525590612,
2.62946121471301));
#88280=CARTESIAN_POINT('Ctrl Pts',(-18.157199885527,0.439131547242386,2.47143604597126));
#88281=CARTESIAN_POINT('Ctrl Pts',(-16.3568348773615,2.88439717230558,2.31341087722953));
#88282=CARTESIAN_POINT('Ctrl Pts',(-13.3251748429328,2.7121404668189,2.1553857084878));
#88283=CARTESIAN_POINT('Ctrl Pts',(-11.8133781165089,0.0786817934940617,
1.99736053974606));
#88284=CARTESIAN_POINT('Ctrl Pts',(-13.1933662837771,-2.62618067533236,
1.83933537100432));
#88285=CARTESIAN_POINT('Ctrl Pts',(-16.2128289732284,-2.94784286454329,
1.68131020226259));
#88286=CARTESIAN_POINT('Ctrl Pts',(-18.1316832938591,-0.594415157792721,
1.52328503352085));
#88287=CARTESIAN_POINT('Ctrl Pts',(-17.2085996164135,2.29844457164632,1.36525986477911));
#88288=CARTESIAN_POINT('Ctrl Pts',(-14.2812836382811,3.10549241982875,1.20723469603738));
#88289=CARTESIAN_POINT('Ctrl Pts',(-12.0061479793382,1.09443459548537,1.04920952729564));
#88290=CARTESIAN_POINT('Ctrl Pts',(-12.4479353308854,-1.90990355671544,
0.891184358553913));
#88291=CARTESIAN_POINT('Ctrl Pts',(-15.2055172440938,-3.1808409825652,0.733159189812176));
#88292=CARTESIAN_POINT('Ctrl Pts',(-17.7768769495327,-1.565648008873,0.575134021070441));
#88293=CARTESIAN_POINT('Ctrl Pts',(-17.827740945409,1.47112779768063,0.417108852328704));
#88294=CARTESIAN_POINT('Ctrl Pts',(-15.313563066009,3.17133757780266,0.259083683586969));
#88295=CARTESIAN_POINT('Ctrl Pts',(-12.5127473578457,1.99668960841177,0.101058514845233));
#88296=CARTESIAN_POINT('Ctrl Pts',(-11.973205329235,-0.99614959597368,-0.0569666538965035));
#88297=CARTESIAN_POINT('Ctrl Pts',(-13.4387230749784,-2.37858924209377,
-0.162316766390993));
#88298=CARTESIAN_POINT('Ctrl Pts',(-14.3023752432315,-2.60948011226316,
-0.214991822638238));
#88299=CARTESIAN_POINT('Ctrl Pts',(-12.8049916319232,1.87865014331576,6.21467382945635));
#88300=CARTESIAN_POINT('Ctrl Pts',(-12.1828646190277,1.15181811593143,6.1619715851807));
#88301=CARTESIAN_POINT('Ctrl Pts',(-11.7280047812329,-0.955389307143031,
6.05659428465781));
#88302=CARTESIAN_POINT('Ctrl Pts',(-14.0172921625136,-3.26701387535251,
5.89854192788767));
#88303=CARTESIAN_POINT('Ctrl Pts',(-17.1978463612657,-2.60548538019996,
5.74051675914593));
#88304=CARTESIAN_POINT('Ctrl Pts',(-18.3839191570272,0.416501264781063,
5.5824915904042));
#88305=CARTESIAN_POINT('Ctrl Pts',(-16.4991646101598,3.06253718091595,5.42446642166246));
#88306=CARTESIAN_POINT('Ctrl Pts',(-13.2539539883606,2.9283623445602,5.26644125292072));
#88307=CARTESIAN_POINT('Ctrl Pts',(-11.5932385577395,0.137296740003281,
5.10841608417899));
#88308=CARTESIAN_POINT('Ctrl Pts',(-13.024078112561,-2.77863323171906,4.95039091543725));
#88309=CARTESIAN_POINT('Ctrl Pts',(-16.2480197738846,-3.17288081084153,
4.79236574669552));
#88310=CARTESIAN_POINT('Ctrl Pts',(-18.3394131795346,-0.687885688585299,
4.63434057795378));
#88311=CARTESIAN_POINT('Ctrl Pts',(-17.4003685567714,2.42138581051048,4.47631540921205));
#88312=CARTESIAN_POINT('Ctrl Pts',(-14.2830465661856,3.33328858561909,4.31829024047031));
#88313=CARTESIAN_POINT('Ctrl Pts',(-11.8163427625913,1.22032084114078,4.16026507172857));
#88314=CARTESIAN_POINT('Ctrl Pts',(-12.238732173342,-2.00006395175156,4.00223990298685));
#88315=CARTESIAN_POINT('Ctrl Pts',(-15.1669064558191,-3.40543576570869,
3.8442147342451));
#88316=CARTESIAN_POINT('Ctrl Pts',(-17.9436170989244,-1.72045691570957,
3.68618956550337));
#88317=CARTESIAN_POINT('Ctrl Pts',(-18.0490652453263,1.5257963204396,3.52816439676163));
#88318=CARTESIAN_POINT('Ctrl Pts',(-15.3875592051944,3.38742535529361,3.3701392280199));
#88319=CARTESIAN_POINT('Ctrl Pts',(-12.3743524118776,2.17504661970418,3.21211405927816));
#88320=CARTESIAN_POINT('Ctrl Pts',(-11.7438583361436,-1.01113525599524,
3.05408889053642));
#88321=CARTESIAN_POINT('Ctrl Pts',(-14.0682353935039,-3.27973593037319,
2.89606372179469));
#88322=CARTESIAN_POINT('Ctrl Pts',(-17.2381666172201,-2.57205421186611,
2.73803855305295));
#88323=CARTESIAN_POINT('Ctrl Pts',(-18.3770149727813,0.469705392064734,
2.58001338431122));
#88324=CARTESIAN_POINT('Ctrl Pts',(-16.4513023763387,3.08521879877688,2.42198821556948));
#88325=CARTESIAN_POINT('Ctrl Pts',(-13.2085677697714,2.90096899050306,2.26396304682775));
#88326=CARTESIAN_POINT('Ctrl Pts',(-11.5915145688199,0.0841598898862171,
2.10593787808601));
#88327=CARTESIAN_POINT('Ctrl Pts',(-13.0675822465394,-2.80902438343592,
1.94791270934427));
#88328=CARTESIAN_POINT('Ctrl Pts',(-16.2972702871271,-3.15308179776768,
1.78988754060254));
#88329=CARTESIAN_POINT('Ctrl Pts',(-18.3497218284633,-0.635800380304125,
1.6318623718608));
#88330=CARTESIAN_POINT('Ctrl Pts',(-17.3623698986238,2.45847016786588,1.47383720311907));
#88331=CARTESIAN_POINT('Ctrl Pts',(-14.2312441395194,3.32170745593136,1.31581203437733));
#88332=CARTESIAN_POINT('Ctrl Pts',(-11.7977057308239,1.17063288663686,1.15778686563559));
#88333=CARTESIAN_POINT('Ctrl Pts',(-12.2702518334002,-2.04287759453019,
0.999761696893858));
#88334=CARTESIAN_POINT('Ctrl Pts',(-15.2198260596839,-3.40230204409951,
0.841736528152121));
#88335=CARTESIAN_POINT('Ctrl Pts',(-17.970212649231,-1.67465379442927,0.683711359410386));
#88336=CARTESIAN_POINT('Ctrl Pts',(-18.0246179709966,1.57355276186863,0.525686190668649));
#88337=CARTESIAN_POINT('Ctrl Pts',(-15.3353944023873,3.39213697969462,0.367661021926914));
#88338=CARTESIAN_POINT('Ctrl Pts',(-12.3395762960243,2.13570598887754,0.209635853185178));
#88339=CARTESIAN_POINT('Ctrl Pts',(-11.7624695004062,-1.06550494827847,
0.0516106844434421));
#88340=CARTESIAN_POINT('Ctrl Pts',(-13.3300216192754,-2.54419478521757,
-0.0537394280510476));
#88341=CARTESIAN_POINT('Ctrl Pts',(-14.2538042143642,-2.79116106987219,
-0.106414484298293));
#88342=CARTESIAN_POINT('Ctrl Pts',(-12.6621151685845,2.0009343642925,6.32325116779629));
#88343=CARTESIAN_POINT('Ctrl Pts',(-11.9994929536466,1.22679172478282,6.27054892352065));
#88344=CARTESIAN_POINT('Ctrl Pts',(-11.5150255909403,-1.01757706337277,
6.16517162299776));
#88345=CARTESIAN_POINT('Ctrl Pts',(-13.9533262012184,-3.47966882235748,
6.00711926622762));
#88346=CARTESIAN_POINT('Ctrl Pts',(-17.3409075539365,-2.77508042221333,
5.84909409748589));
#88347=CARTESIAN_POINT('Ctrl Pts',(-18.6041836482299,0.443611971306593,
5.69106892874414));
#88348=CARTESIAN_POINT('Ctrl Pts',(-16.5967475353903,3.2618824260714,5.53304376000242));
#88349=CARTESIAN_POINT('Ctrl Pts',(-13.1403011738212,3.11897394370029,5.37501859126067));
#88350=CARTESIAN_POINT('Ctrl Pts',(-11.3714872271351,0.146233595518226,
5.21699342251894));
#88351=CARTESIAN_POINT('Ctrl Pts',(-12.8954623244772,-2.95949873311632,
5.0589682537772));
#88352=CARTESIAN_POINT('Ctrl Pts',(-16.329255296292,-3.37940849221227,4.90094308503547));
#88353=CARTESIAN_POINT('Ctrl Pts',(-18.5567807083594,-0.732661223747603,
4.74291791629373));
#88354=CARTESIAN_POINT('Ctrl Pts',(-17.5566122299567,2.57899752899671,4.584892747552));
#88355=CARTESIAN_POINT('Ctrl Pts',(-14.2363789668763,3.55025745522654,4.42686757881026));
#88356=CARTESIAN_POINT('Ctrl Pts',(-11.6091136270768,1.2997533975066,4.26884241006853));
#88357=CARTESIAN_POINT('Ctrl Pts',(-12.0589970128107,-2.13025118385213,
4.11081724132679));
#88358=CARTESIAN_POINT('Ctrl Pts',(-15.1777706531783,-3.62710080599184,
3.95279207258505));
#88359=CARTESIAN_POINT('Ctrl Pts',(-18.1352216534374,-1.83244409672364,
3.79476690384331));
#88360=CARTESIAN_POINT('Ctrl Pts',(-18.247533581519,1.6251127445636,3.63674173510157));
#88361=CARTESIAN_POINT('Ctrl Pts',(-15.4127860286444,3.60791807032241,3.47871656635985));
#88362=CARTESIAN_POINT('Ctrl Pts',(-12.2034449808077,2.31662374220618,3.32069139761811));
#88363=CARTESIAN_POINT('Ctrl Pts',(-11.5319110780704,-1.0769516015886,3.16266622887638));
#88364=CARTESIAN_POINT('Ctrl Pts',(-14.0075854052959,-3.49321897546388,
3.00464106013463));
#88365=CARTESIAN_POINT('Ctrl Pts',(-17.3838523172302,-2.73947316782609,
2.8466158913929));
#88366=CARTESIAN_POINT('Ctrl Pts',(-18.5968300600357,0.500279236887077,
2.68859072265117));
#88367=CARTESIAN_POINT('Ctrl Pts',(-16.545769875316,3.28604042524819,2.53056555390943));
#88368=CARTESIAN_POINT('Ctrl Pts',(-13.0919606966101,3.08979751418722,2.37254038516769));
#88369=CARTESIAN_POINT('Ctrl Pts',(-11.3696510211309,0.0896379862783765,
2.21451521642595));
#88370=CARTESIAN_POINT('Ctrl Pts',(-12.9417982093016,-2.99186809153947,
2.05649004768421));
#88371=CARTESIAN_POINT('Ctrl Pts',(-16.3817116010259,-3.35832073099206,
1.89846487894248));
#88372=CARTESIAN_POINT('Ctrl Pts',(-18.5677603630673,-0.677185602815532,
1.74043971020074));
#88373=CARTESIAN_POINT('Ctrl Pts',(-17.5161401808341,2.61849576408543,1.58241454145901));
#88374=CARTESIAN_POINT('Ctrl Pts',(-14.1812046407576,3.53792249203398,1.42438937271727));
#88375=CARTESIAN_POINT('Ctrl Pts',(-11.5892634823095,1.24683117778833,1.26636420397553));
#88376=CARTESIAN_POINT('Ctrl Pts',(-12.0925683359151,-2.17585163234495,
1.1083390352338));
#88377=CARTESIAN_POINT('Ctrl Pts',(-15.2341348752738,-3.62376310563382,
0.950313866492068));
#88378=CARTESIAN_POINT('Ctrl Pts',(-18.1635483489294,-1.78365957998554,
0.792288697750331));
#88379=CARTESIAN_POINT('Ctrl Pts',(-18.2214949965841,1.67597772605664,0.634263529008596));
#88380=CARTESIAN_POINT('Ctrl Pts',(-15.3572257387657,3.61293638158657,0.476238360266859));
#88381=CARTESIAN_POINT('Ctrl Pts',(-12.1664052342031,2.27472236934331,0.318213191525124));
#88382=CARTESIAN_POINT('Ctrl Pts',(-11.5517336715772,-1.13486030058325,
0.160188022783388));
#88383=CARTESIAN_POINT('Ctrl Pts',(-13.2213201635726,-2.70980032834139,
0.0548379102888979));
#88384=CARTESIAN_POINT('Ctrl Pts',(-14.2052331854969,-2.97284202748121,
0.00216285404165282));
#88385=CARTESIAN_POINT('',(-13.0846966603782,1.6372236474585,-0.00127820437379453));
#88386=CARTESIAN_POINT('Ctrl Pts',(-14.2062007174672,-2.96922295374571,
-1.11022302462516E-15));
#88387=CARTESIAN_POINT('Ctrl Pts',(-14.1122367217159,-2.93485050436548,
5.64576421554524E-15));
#88388=CARTESIAN_POINT('Ctrl Pts',(-14.020377975911,-2.89562054314027,4.74471375630515E-15));
#88389=CARTESIAN_POINT('Ctrl Pts',(-13.9308393979082,-2.85186989239737,
-7.7715611723761E-16));
#88390=CARTESIAN_POINT('Ctrl Pts',(-13.8399813184291,-2.80747450226358,
-6.38040002655828E-15));
#88391=CARTESIAN_POINT('Ctrl Pts',(-13.7515116459329,-2.75842351507099,
-1.18049888343227E-15));
#88392=CARTESIAN_POINT('Ctrl Pts',(-13.6656843105487,-2.70502283631973,
1.0547118733939E-15));
#88393=CARTESIAN_POINT('Ctrl Pts',(-13.5797858146085,-2.65157788237369,
3.29177587242458E-15));
#88394=CARTESIAN_POINT('Ctrl Pts',(-13.4965334527781,-2.59377523991115,
7.44663497626135E-15));
#88395=CARTESIAN_POINT('Ctrl Pts',(-13.4162202066268,-2.53188703698736,
4.27435864480685E-15));
#88396=CARTESIAN_POINT('Ctrl Pts',(-13.3529896133675,-2.48316247442576,
1.77682649372841E-15));
#88397=CARTESIAN_POINT('Ctrl Pts',(-13.2915814624985,-2.43190471019256,
-1.27111200054493E-14));
#88398=CARTESIAN_POINT('Ctrl Pts',(-13.2321590416994,-2.37823623684125,
-8.27116153345742E-15));
#88399=CARTESIAN_POINT('Ctrl Pts',(-13.2181178171658,-2.36555464166943,
-7.6289592557529E-15));
#88400=CARTESIAN_POINT('Ctrl Pts',(-13.2041849090213,-2.35273580694004,
-1.00719496978036E-14));
#88401=CARTESIAN_POINT('Ctrl Pts',(-13.1903817643062,-2.33979961362129,
-8.10462807976364E-15));
#88402=CARTESIAN_POINT('Ctrl Pts',(-13.1179465671244,-2.27191394458243,
9.29987229349879E-15));
#88403=CARTESIAN_POINT('Ctrl Pts',(-13.0489770747074,-2.20070726068955,
3.12731471788556E-15));
#88404=CARTESIAN_POINT('Ctrl Pts',(-12.9837133664394,-2.12646930662299,
-7.7715611723761E-15));
#88405=CARTESIAN_POINT('Ctrl Pts',(-12.9192219935262,-2.05310988977285,
-1.8541458991958E-14));
#88406=CARTESIAN_POINT('Ctrl Pts',(-12.8583487844939,-1.97678971688283,
-1.95555689464262E-14));
#88407=CARTESIAN_POINT('Ctrl Pts',(-12.8013680326043,-1.8977621623991,-6.32827124036339E-15));
#88408=CARTESIAN_POINT('Ctrl Pts',(-12.7457289378947,-1.82059537461941,
6.58757920763005E-15));
#88409=CARTESIAN_POINT('Ctrl Pts',(-12.693800881531,-1.74084648362158,1.28239991180334E-14));
#88410=CARTESIAN_POINT('Ctrl Pts',(-12.6458851364556,-1.65873742553322,
-8.04911692853238E-16));
#88411=CARTESIAN_POINT('Ctrl Pts',(-12.6258463528357,-1.62439869938637,
-6.71154134295195E-15));
#88412=CARTESIAN_POINT('Ctrl Pts',(-12.6065099009786,-1.58964707331907,
1.33128856964392E-14));
#88413=CARTESIAN_POINT('Ctrl Pts',(-12.5879004560125,-1.55449847432752,
5.6621374255883E-15));
#88414=CARTESIAN_POINT('Ctrl Pts',(-12.5746720374845,-1.5295132918581,3.79392865924309E-16));
#88415=CARTESIAN_POINT('Ctrl Pts',(-12.5618110082776,-1.50432751614023,
-2.08393312802743E-14));
#88416=CARTESIAN_POINT('Ctrl Pts',(-12.5493267442101,-1.4789468615225,-1.93178806284777E-14));
#88417=CARTESIAN_POINT('Ctrl Pts',(-12.5425334913993,-1.46513609923887,
-1.72001277010202E-14));
#88418=CARTESIAN_POINT('Ctrl Pts',(-12.5358509509352,-1.45126567608035,
1.01097939998197E-14));
#88419=CARTESIAN_POINT('Ctrl Pts',(-12.5292882307234,-1.43735295427421,
6.07847105982273E-15));
#88420=CARTESIAN_POINT('Ctrl Pts',(-12.4893051056442,-1.35259022202115,
-1.96573038807791E-14));
#88421=CARTESIAN_POINT('Ctrl Pts',(-12.4537033885735,-1.26613539622463,
1.45565814917559E-14));
#88422=CARTESIAN_POINT('Ctrl Pts',(-12.4227276425839,-1.1782187591175,7.13318293321663E-15));
#88423=CARTESIAN_POINT('Ctrl Pts',(-12.3918929845728,-1.09070256371739,
-2.56403613302056E-16));
#88424=CARTESIAN_POINT('Ctrl Pts',(-12.3656418798435,-1.00173718392728,
-1.0741215117424E-14));
#88425=CARTESIAN_POINT('Ctrl Pts',(-12.3442660244676,-0.911540477667729,
-1.78190795452338E-14));
#88426=CARTESIAN_POINT('Ctrl Pts',(-12.3412859264738,-0.898965775105114,
-1.85340371603588E-14));
#88427=CARTESIAN_POINT('Ctrl Pts',(-12.3384006710999,-0.886367134434174,
-9.62165260182121E-15));
#88428=CARTESIAN_POINT('Ctrl Pts',(-12.3356111334694,-0.873745142704312,
-6.41153796721028E-15));
#88429=CARTESIAN_POINT('Ctrl Pts',(-12.315042930982,-0.780678937448357,
1.40106201757014E-14));
#88430=CARTESIAN_POINT('Ctrl Pts',(-12.299674369116,-0.686342237612556,
1.44936159865722E-14));
#88431=CARTESIAN_POINT('Ctrl Pts',(-12.28942812764,-0.591144411737914,-8.82627304576999E-15));
#88432=CARTESIAN_POINT('Ctrl Pts',(-12.2835920569734,-0.536921481269743,
-2.21088528726585E-14));
#88433=CARTESIAN_POINT('Ctrl Pts',(-12.2794187288502,-0.48241937068935,
-1.00134788350089E-14));
#88434=CARTESIAN_POINT('Ctrl Pts',(-12.2769008964915,-0.427716487911291,
1.80966353013901E-14));
#88435=CARTESIAN_POINT('Ctrl Pts',(-12.2763261180039,-0.415228746175687,
2.45270756093043E-14));
#88436=CARTESIAN_POINT('Ctrl Pts',(-12.2758377484422,-0.402732126744129,
2.70255838552933E-15));
#88437=CARTESIAN_POINT('Ctrl Pts',(-12.2754358439927,-0.390237005741378,
3.5527136788005E-15));
#88438=CARTESIAN_POINT('Ctrl Pts',(-12.2724426926483,-0.297180588281585,
8.8744226101631E-15));
#88439=CARTESIAN_POINT('Ctrl Pts',(-12.274233724762,-0.204061140642064,
2.30567975120578E-14));
#88440=CARTESIAN_POINT('Ctrl Pts',(-12.2806740030689,-0.111252623398913,
1.59594559789866E-14));
#88441=CARTESIAN_POINT('Ctrl Pts',(-12.2871453671104,-0.0179961408968059,
8.82785721896908E-15));
#88442=CARTESIAN_POINT('Ctrl Pts',(-12.2983113204397,0.0749473924486998,
2.19278460780688E-14));
#88443=CARTESIAN_POINT('Ctrl Pts',(-12.3140861273615,0.167186518104898,
1.25177646026486E-14));
#88444=CARTESIAN_POINT('Ctrl Pts',(-12.3296305385394,0.258078463914099,
3.24512016419198E-15));
#88445=CARTESIAN_POINT('Ctrl Pts',(-12.349650625959,0.348287277575547,-7.24335738920225E-15));
#88446=CARTESIAN_POINT('Ctrl Pts',(-12.3741075834303,0.4374131430529,-1.5404344466674E-15));
#88447=CARTESIAN_POINT('Ctrl Pts',(-12.3831485976605,0.470360340961913,
5.6776758695313E-16));
#88448=CARTESIAN_POINT('Ctrl Pts',(-12.392796332953,0.503159232797977,-2.0625677205409E-15));
#88449=CARTESIAN_POINT('Ctrl Pts',(-12.4030501659707,0.535788378267512,
-5.60662627435704E-15));
#88450=CARTESIAN_POINT('Ctrl Pts',(-12.4093070529646,0.555698676743727,
-7.86954492739309E-15));
#88451=CARTESIAN_POINT('Ctrl Pts',(-12.415789630245,0.575545756853617,2.60155169675598E-14));
#88452=CARTESIAN_POINT('Ctrl Pts',(-12.4224978791286,0.595324601387584,
2.53685961126848E-14));
#88453=CARTESIAN_POINT('Ctrl Pts',(-12.4279646784057,0.611443110834228,
2.47251388076511E-14));
#88454=CARTESIAN_POINT('Ctrl Pts',(-12.4335818537163,0.627517439423588,
-7.68104876148795E-15));
#88455=CARTESIAN_POINT('Ctrl Pts',(-12.4393432110049,0.643528266897872,
-6.0507154842071E-15));
#88456=CARTESIAN_POINT('Ctrl Pts',(-12.4710550424473,0.731655532172561,
3.64288882194921E-16));
#88457=CARTESIAN_POINT('Ctrl Pts',(-12.5071698359129,0.817978578845512,
1.73303171070469E-14));
#88458=CARTESIAN_POINT('Ctrl Pts',(-12.5476222825399,0.902080078937405,
1.96509475358653E-14));
#88459=CARTESIAN_POINT('Ctrl Pts',(-12.5779616175101,0.965156204006325,
2.14637817750454E-14));
#88460=CARTESIAN_POINT('Ctrl Pts',(-12.6107419363143,1.02698221352591,-5.06122749809775E-15));
#88461=CARTESIAN_POINT('Ctrl Pts',(-12.6459517365208,1.0873663829419,1.00891517362811E-14));
#88462=CARTESIAN_POINT('Ctrl Pts',(-12.6596298565035,1.11082411088935,1.63169981023069E-14));
#88463=CARTESIAN_POINT('Ctrl Pts',(-12.6736747531009,1.13406408087531,4.30095806415684E-15));
#88464=CARTESIAN_POINT('Ctrl Pts',(-12.6880862551922,1.15707437538469,2.73392419813945E-15));
#88465=CARTESIAN_POINT('Ctrl Pts',(-12.6997302261644,1.17566585874512,9.13452452349396E-16));
#88466=CARTESIAN_POINT('Ctrl Pts',(-12.7116130981113,1.19410637782525,-1.36214186568185E-15));
#88467=CARTESIAN_POINT('Ctrl Pts',(-12.723722803297,1.2123723319515,-2.56045185054177E-15));
#88468=CARTESIAN_POINT('Ctrl Pts',(-12.7711778313141,1.28395222192633,-7.25634105945887E-15));
#88469=CARTESIAN_POINT('Ctrl Pts',(-12.8221585037883,1.35292687972583,9.32156199594571E-15));
#88470=CARTESIAN_POINT('Ctrl Pts',(-12.8766328873954,1.41894276037641,4.6525283625698E-15));
#88471=CARTESIAN_POINT('Ctrl Pts',(-12.923917575018,1.47624566291498,5.99728087757576E-16));
#88472=CARTESIAN_POINT('Ctrl Pts',(-12.9738352609869,1.53131901243648,2.71861438742187E-14));
#88473=CARTESIAN_POINT('Ctrl Pts',(-13.0263829703992,1.58390514293349,1.23694457454526E-14));
#88474=CARTESIAN_POINT('Ctrl Pts',(-13.044910806381,1.60244652583416,6.24075109223694E-15));
#88475=CARTESIAN_POINT('Ctrl Pts',(-13.0637657557693,1.62067844062891,7.06479597108194E-15));
#88476=CARTESIAN_POINT('Ctrl Pts',(-13.0829381663571,1.63859681658414,2.10378589549087E-14));
#88477=CARTESIAN_POINT('Ctrl Pts',(-13.0863689594075,1.63579414673148,-0.00127820437379467));
#88478=CARTESIAN_POINT('Ctrl Pts',(-13.094817760828,1.64567796291114,-0.000852136249196398));
#88479=CARTESIAN_POINT('Ctrl Pts',(-13.1033431379554,1.65549632126644,-0.000426068124598269));
#88480=CARTESIAN_POINT('Ctrl Pts',(-13.1119440673944,1.66524804319138,0.));
#88481=CARTESIAN_POINT('Ctrl Pts',(-15.7948103993656,-2.97300505757792,
5.99773971486702));
#88482=CARTESIAN_POINT('Ctrl Pts',(-16.7787773788947,-2.70994893328083,
5.94506465861977));
#88483=CARTESIAN_POINT('Ctrl Pts',(-18.448455143976,-1.13492077598002,5.83971454612528));
#88484=CARTESIAN_POINT('Ctrl Pts',(-17.8337504113313,2.2748462209877,5.68168937738353));
#88485=CARTESIAN_POINT('Ctrl Pts',(-14.6427546314668,3.61313520212619,5.52366420864182));
#88486=CARTESIAN_POINT('Ctrl Pts',(-11.7783282110555,1.6760693608975,5.36563903990007));
#88487=CARTESIAN_POINT('Ctrl Pts',(-11.8362780796478,-1.78375726249727,
5.20761387115834));
#88488=CARTESIAN_POINT('Ctrl Pts',(-14.7658522558612,-3.62396206689039,
5.04958870241659));
#88489=CARTESIAN_POINT('Ctrl Pts',(-17.9075912210902,-2.17597096634872,
4.89156353367486));
#88490=CARTESIAN_POINT('Ctrl Pts',(-18.4109236680194,1.24689956054639,4.73353836493312));
#88491=CARTESIAN_POINT('Ctrl Pts',(-15.8188402958995,3.5381166513751,4.5755131961914));
#88492=CARTESIAN_POINT('Ctrl Pts',(-12.483721745114,2.6186394399734,4.41748802744966));
#88493=CARTESIAN_POINT('Ctrl Pts',(-11.4320438624152,-0.677222756500938,
4.25946285870792));
#88494=CARTESIAN_POINT('Ctrl Pts',(-13.6182125778512,-3.35850501831769,
4.10143768996618));
#88495=CARTESIAN_POINT('Ctrl Pts',(-17.05831473289,-2.99203226502705,3.94341252122444));
#88496=CARTESIAN_POINT('Ctrl Pts',(-18.6305481896681,0.0896429040657021,
3.78538735248272));
#88497=CARTESIAN_POINT('Ctrl Pts',(-16.9081440050834,3.08996706380467,3.62736218374098));
#88498=CARTESIAN_POINT('Ctrl Pts',(-13.4541453022121,3.28622074264122,3.46933701499924));
#88499=CARTESIAN_POINT('Ctrl Pts',(-11.4029725681304,0.500306689286977,
3.3113118462575));
#88500=CARTESIAN_POINT('Ctrl Pts',(-12.6160168715814,-2.7396234933372,3.15328667751578));
#88501=CARTESIAN_POINT('Ctrl Pts',(-15.9924690523316,-3.49341066179973,
2.99526150877404));
#88502=CARTESIAN_POINT('Ctrl Pts',(-18.4682792293058,-1.07701069806446,
2.8372363400323));
#88503=CARTESIAN_POINT('Ctrl Pts',(-17.7967084769259,2.31675086422845,2.67921117129056));
#88504=CARTESIAN_POINT('Ctrl Pts',(-14.5871913202092,3.60811605075546,2.52118600254882));
#88505=CARTESIAN_POINT('Ctrl Pts',(-11.7522882137895,1.62520192058609,2.3631608338071));
#88506=CARTESIAN_POINT('Ctrl Pts',(-11.8646063049427,-1.8325446496698,2.20513566506536));
#88507=CARTESIAN_POINT('Ctrl Pts',(-14.8222195917507,-3.62729983954678,
2.04711049632362));
#88508=CARTESIAN_POINT('Ctrl Pts',(-17.9411643715581,-2.1303680778752,1.88908532758189));
#88509=CARTESIAN_POINT('Ctrl Pts',(-18.3910724434807,1.29982471805251,1.73106015884016));
#88510=CARTESIAN_POINT('Ctrl Pts',(-15.7636629367787,3.55045227500164,1.57303499009842));
#88511=CARTESIAN_POINT('Ctrl Pts',(-12.4432474772716,2.57913904223364,1.41500982135668));
#88512=CARTESIAN_POINT('Ctrl Pts',(-11.4430241205592,-0.732701416452974,
1.25698465261494));
#88513=CARTESIAN_POINT('Ctrl Pts',(-13.6706717561852,-3.3795939532912,1.09895948387321));
#88514=CARTESIAN_POINT('Ctrl Pts',(-17.1046531716412,-2.95966109719462,
0.940934315131468));
#88515=CARTESIAN_POINT('Ctrl Pts',(-18.6287118598364,0.146241559192967,
0.782909146389736));
#88516=CARTESIAN_POINT('Ctrl Pts',(-16.8598009208359,3.11914519751865,0.624883977647998));
#88517=CARTESIAN_POINT('Ctrl Pts',(-13.4031647554911,3.26206124447765,0.466858808906264));
#88518=CARTESIAN_POINT('Ctrl Pts',(-11.3956187510643,0.443636597386532,
0.308833640164527));
#88519=CARTESIAN_POINT('Ctrl Pts',(-12.658963648928,-2.77523315149222,0.150808471422791));
#88520=CARTESIAN_POINT('Ctrl Pts',(-16.0467319118579,-3.47985905282973,
-0.00721669731894459));
#88521=CARTESIAN_POINT('Ctrl Pts',(-18.4847448337578,-1.01805770532123,
-0.16524186606068));
#88522=CARTESIAN_POINT('Ctrl Pts',(-18.0009214582863,1.22570085496208,-0.27059197855517));
#88523=CARTESIAN_POINT('Ctrl Pts',(-17.3390382616395,1.99984565752206,-0.323267034802415));
#88524=CARTESIAN_POINT('Ctrl Pts',(-15.7463046910186,-2.79156843275239,
6.10617103348288));
#88525=CARTESIAN_POINT('Ctrl Pts',(-16.6702221098346,-2.54456610399477,
6.05349597723563));
#88526=CARTESIAN_POINT('Ctrl Pts',(-18.238002739736,-1.06565880331255,5.94814586474115));
#88527=CARTESIAN_POINT('Ctrl Pts',(-17.6608122224375,2.13601685058987,5.7901206959994));
#88528=CARTESIAN_POINT('Ctrl Pts',(-14.6645566104899,3.39263269929958,5.63209552725768));
#88529=CARTESIAN_POINT('Ctrl Pts',(-11.9749404751994,1.57378215925296,5.47407035851593));
#88530=CARTESIAN_POINT('Ctrl Pts',(-12.0293537778045,-1.67489808097969,
5.31604518977421));
#88531=CARTESIAN_POINT('Ctrl Pts',(-14.7801418300746,-3.40279882189813,
5.15802002103245));
#88532=CARTESIAN_POINT('Ctrl Pts',(-17.7301466734657,-2.04317575739126,
4.99999485229074));
#88533=CARTESIAN_POINT('Ctrl Pts',(-18.2027617356052,1.17080374389605,4.84196968354898));
#88534=CARTESIAN_POINT('Ctrl Pts',(-15.7688680904435,3.32219238248486,4.68394451480727));
#88535=CARTESIAN_POINT('Ctrl Pts',(-12.6372852355376,2.45882904866149,4.52591934606551));
#88536=CARTESIAN_POINT('Ctrl Pts',(-11.6497891761942,-0.635893189677169,
4.36789417732379));
#88537=CARTESIAN_POINT('Ctrl Pts',(-13.7025403341938,-3.15354209252986,
4.20986900858204));
#88538=CARTESIAN_POINT('Ctrl Pts',(-16.9326998514042,-2.80943444732343,
4.05184383984032));
#88539=CARTESIAN_POINT('Ctrl Pts',(-18.4089830066151,0.0841721747402409,
3.89381867109857));
#88540=CARTESIAN_POINT('Ctrl Pts',(-16.7916937464197,2.9013924788238,3.73579350235685));
#88541=CARTESIAN_POINT('Ctrl Pts',(-13.5484857602353,3.08566918338413,3.57776833361511));
#88542=CARTESIAN_POINT('Ctrl Pts',(-11.6224920455628,0.469773960507896,
3.41974316487337));
#88543=CARTESIAN_POINT('Ctrl Pts',(-12.7615066518153,-2.57242968427965,
3.26171799613163));
#88544=CARTESIAN_POINT('Ctrl Pts',(-15.9319006269131,-3.28021471112657,
3.1036928273899));
#88545=CARTESIAN_POINT('Ctrl Pts',(-18.2566170003051,-1.01128286303783,
2.94566765864816));
#88546=CARTESIAN_POINT('Ctrl Pts',(-17.626030884104,2.17536413624566,2.78764248990643));
#88547=CARTESIAN_POINT('Ctrl Pts',(-14.6123842183408,3.38791985682055,2.62961732116469));
#88548=CARTESIAN_POINT('Ctrl Pts',(-11.9504896475187,1.52601905832371,2.47159215242296));
#88549=CARTESIAN_POINT('Ctrl Pts',(-12.0559531874784,-1.72070807030351,
2.31356698368122));
#88550=CARTESIAN_POINT('Ctrl Pts',(-14.8330691788211,-3.40593289688381,
2.15554181493948));
#88551=CARTESIAN_POINT('Ctrl Pts',(-17.7616709208919,-2.00035592310254,
1.99751664619775));
#88552=CARTESIAN_POINT('Ctrl Pts',(-18.1841219920795,1.22049898360509,1.83949147745601));
#88553=CARTESIAN_POINT('Ctrl Pts',(-15.7170580965346,3.33377518737326,1.68146630871428));
#88554=CARTESIAN_POINT('Ctrl Pts',(-12.5992810322955,2.4217392821539,1.52344113997254));
#88555=CARTESIAN_POINT('Ctrl Pts',(-11.6600993308776,-0.687986096622873,
1.3654159712308));
#88556=CARTESIAN_POINT('Ctrl Pts',(-13.751798032519,-3.17334401146786,1.20739080248907));
#88557=CARTESIAN_POINT('Ctrl Pts',(-16.9762103467904,-2.77903882790729,
1.04936563374733));
#88558=CARTESIAN_POINT('Ctrl Pts',(-18.4072587443651,0.137316725768431,
0.891340465005602));
#88559=CARTESIAN_POINT('Ctrl Pts',(-16.7463009450912,2.92878992868517,0.733315296263867));
#88560=CARTESIAN_POINT('Ctrl Pts',(-13.5006164555573,3.06298409166098,0.57529012752213));
#88561=CARTESIAN_POINT('Ctrl Pts',(-11.615587017423,0.416562332351654,0.417264958780395));
#88562=CARTESIAN_POINT('Ctrl Pts',(-12.8018324721914,-2.60586615535233,
0.259239790038659));
#88563=CARTESIAN_POINT('Ctrl Pts',(-15.9828519313309,-3.26749013007776,
0.101214621296923));
#88564=CARTESIAN_POINT('Ctrl Pts',(-18.2720777414488,-0.955927654966856,
-0.0568105474448126));
#88565=CARTESIAN_POINT('Ctrl Pts',(-17.8177811506805,1.15089875343075,-0.162160659939302));
#88566=CARTESIAN_POINT('Ctrl Pts',(-17.1962913778265,1.87779902818723,-0.214835716186548));
#88567=CARTESIAN_POINT('Ctrl Pts',(-15.6977989826716,-2.61013180792686,
6.21460235209875));
#88568=CARTESIAN_POINT('Ctrl Pts',(-16.5616668407743,-2.3791832747087,6.16192729585151));
#88569=CARTESIAN_POINT('Ctrl Pts',(-18.0275503354958,-0.996396830645096,
6.05657718335701));
#88570=CARTESIAN_POINT('Ctrl Pts',(-17.4878740335435,1.99718748019203,5.89855201461528));
#88571=CARTESIAN_POINT('Ctrl Pts',(-14.6863585895132,3.17213019647298,5.74052684587355));
#88572=CARTESIAN_POINT('Ctrl Pts',(-12.1715527393434,1.47149495760841,5.5825016771318));
#88573=CARTESIAN_POINT('Ctrl Pts',(-12.2224294759612,-1.56603889946212,
5.42447650839008));
#88574=CARTESIAN_POINT('Ctrl Pts',(-14.7944314042879,-3.18163557690586,
5.26645133964833));
#88575=CARTESIAN_POINT('Ctrl Pts',(-17.5527021258414,-1.9103805484338,5.10842617090661));
#88576=CARTESIAN_POINT('Ctrl Pts',(-17.9945998031909,1.09470792724571,4.95040100216485));
#88577=CARTESIAN_POINT('Ctrl Pts',(-15.7188958849874,3.10626811359462,4.79237583342314));
#88578=CARTESIAN_POINT('Ctrl Pts',(-12.7908487259611,2.29901865734959,4.63435066468138));
#88579=CARTESIAN_POINT('Ctrl Pts',(-11.8675344899732,-0.594563622853398,
4.47632549593967));
#88580=CARTESIAN_POINT('Ctrl Pts',(-13.7868680905366,-2.94857916674204,
4.31830032719791));
#88581=CARTESIAN_POINT('Ctrl Pts',(-16.8070849699184,-2.62683662961979,
4.16027515845619));
#88582=CARTESIAN_POINT('Ctrl Pts',(-18.1874178235621,0.0787014454147784,
4.00224998971444));
#88583=CARTESIAN_POINT('Ctrl Pts',(-16.675243487756,2.71281789384293,3.84422482097272));
#88584=CARTESIAN_POINT('Ctrl Pts',(-13.6428262182586,2.88511762412704,3.68619965223097));
#88585=CARTESIAN_POINT('Ctrl Pts',(-11.8420115229951,0.439241231728813,
3.52817448348925));
#88586=CARTESIAN_POINT('Ctrl Pts',(-12.9069964320492,-2.40523587522208,
3.3701493147475));
#88587=CARTESIAN_POINT('Ctrl Pts',(-15.8713322014946,-3.0670187604534,3.21212414600578));
#88588=CARTESIAN_POINT('Ctrl Pts',(-18.0449547713042,-0.945555028011206,
3.05409897726403));
#88589=CARTESIAN_POINT('Ctrl Pts',(-17.4553532912823,2.03397740826286,2.8960738085223));
#88590=CARTESIAN_POINT('Ctrl Pts',(-14.6375771164722,3.16772366288563,2.73804863978056));
#88591=CARTESIAN_POINT('Ctrl Pts',(-12.1486910812479,1.42683619606133,2.58002347103883));
#88592=CARTESIAN_POINT('Ctrl Pts',(-12.2473000700141,-1.60887149093723,
2.42199830229709));
#88593=CARTESIAN_POINT('Ctrl Pts',(-14.8439187658915,-3.18456595422084,
2.26397313355535));
#88594=CARTESIAN_POINT('Ctrl Pts',(-17.5821774702257,-1.87034376832987,
2.10594796481362));
#88595=CARTESIAN_POINT('Ctrl Pts',(-17.9771715406782,1.14117324915768,1.94792279607189));
#88596=CARTESIAN_POINT('Ctrl Pts',(-15.6704532562904,3.11709809974488,1.78989762733015));
#88597=CARTESIAN_POINT('Ctrl Pts',(-12.7553145873195,2.26433952207416,1.63187245858841));
#88598=CARTESIAN_POINT('Ctrl Pts',(-11.8771745411961,-0.643270776792767,
1.47384728984667));
#88599=CARTESIAN_POINT('Ctrl Pts',(-13.8329243088529,-2.96709406964454,
1.31582212110494));
#88600=CARTESIAN_POINT('Ctrl Pts',(-16.8477675219395,-2.59841655861997,
1.1577969523632));
#88601=CARTESIAN_POINT('Ctrl Pts',(-18.1858056288936,0.128391892343889,
0.999771783621469));
#88602=CARTESIAN_POINT('Ctrl Pts',(-16.6328009693466,2.73843465985169,0.841746614879735));
#88603=CARTESIAN_POINT('Ctrl Pts',(-13.5980681556234,2.8639069388443,0.683721446137999));
#88604=CARTESIAN_POINT('Ctrl Pts',(-11.8355552837818,0.389488067316777,
0.525696277396263));
#88605=CARTESIAN_POINT('Ctrl Pts',(-12.9447012954548,-2.43649915921244,
0.367671108654526));
#88606=CARTESIAN_POINT('Ctrl Pts',(-15.9189719508039,-3.05512120732578,
0.209645939912791));
#88607=CARTESIAN_POINT('Ctrl Pts',(-18.0594106491397,-0.893797604612488,
0.0516207711710548));
#88608=CARTESIAN_POINT('Ctrl Pts',(-17.6346408430749,1.07609665189943,-0.0537293413234345));
#88609=CARTESIAN_POINT('Ctrl Pts',(-17.0535444940135,1.7557523988524,-0.10640439757068));
#88610=CARTESIAN_POINT('Ctrl Pts',(-15.6492932743244,-2.42869518310133,
6.32303367071462));
#88611=CARTESIAN_POINT('Ctrl Pts',(-16.4531115717142,-2.21380044542264,
6.27035861446738));
#88612=CARTESIAN_POINT('Ctrl Pts',(-17.8170979312557,-0.927134857977634,
6.16500850197289));
#88613=CARTESIAN_POINT('Ctrl Pts',(-17.3149358446497,1.85835810979419,6.00698333323115));
#88614=CARTESIAN_POINT('Ctrl Pts',(-14.7081605685364,2.95162769364637,5.84895816448941));
#88615=CARTESIAN_POINT('Ctrl Pts',(-12.3681650034873,1.36920775596387,5.69093299574768));
#88616=CARTESIAN_POINT('Ctrl Pts',(-12.4155051741179,-1.45717971794455,
5.53290782700594));
#88617=CARTESIAN_POINT('Ctrl Pts',(-14.8087209785013,-2.96047233191359,
5.3748826582642));
#88618=CARTESIAN_POINT('Ctrl Pts',(-17.375257578217,-1.77758533947633,5.21685748952248));
#88619=CARTESIAN_POINT('Ctrl Pts',(-17.7864378707766,1.01861211059538,5.05883232078073));
#88620=CARTESIAN_POINT('Ctrl Pts',(-15.6689236795314,2.89034384470437,4.90080715203901));
#88621=CARTESIAN_POINT('Ctrl Pts',(-12.9444122163845,2.1392082660377,4.74278198329726));
#88622=CARTESIAN_POINT('Ctrl Pts',(-12.0852798037522,-0.55323405602963,
4.58475681455553));
#88623=CARTESIAN_POINT('Ctrl Pts',(-13.8711958468793,-2.74361624095422,
4.42673164581379));
#88624=CARTESIAN_POINT('Ctrl Pts',(-16.6814700884327,-2.44423881191615,
4.26870647707206));
#88625=CARTESIAN_POINT('Ctrl Pts',(-17.965852640509,0.0732307160893165,
4.11068130833032));
#88626=CARTESIAN_POINT('Ctrl Pts',(-16.5587932290923,2.52424330886206,3.95265613958859));
#88627=CARTESIAN_POINT('Ctrl Pts',(-13.7371666762818,2.68456606486995,3.79463097084684));
#88628=CARTESIAN_POINT('Ctrl Pts',(-12.0615310004275,0.408708502949732,
3.63660580210512));
#88629=CARTESIAN_POINT('Ctrl Pts',(-13.052486212283,-2.23804206616453,3.47858063336337));
#88630=CARTESIAN_POINT('Ctrl Pts',(-15.8107637760761,-2.85382280978022,
3.32055546462165));
#88631=CARTESIAN_POINT('Ctrl Pts',(-17.8332925423033,-0.879827192984582,
3.1625302958799));
#88632=CARTESIAN_POINT('Ctrl Pts',(-17.2846756984605,1.89259068028007,3.00450512713817));
#88633=CARTESIAN_POINT('Ctrl Pts',(-14.6627700146037,2.94752746895072,2.84647995839643));
#88634=CARTESIAN_POINT('Ctrl Pts',(-12.3468925149772,1.32765333379895,2.6884547896547));
#88635=CARTESIAN_POINT('Ctrl Pts',(-12.4386469525498,-1.49703491157095,
2.53042962091296));
#88636=CARTESIAN_POINT('Ctrl Pts',(-14.8547683529619,-2.96319901155788,
2.37240445217123));
#88637=CARTESIAN_POINT('Ctrl Pts',(-17.4026840195596,-1.74033161355722,
2.21437928342949));
#88638=CARTESIAN_POINT('Ctrl Pts',(-17.7702210892769,1.06184751471027,2.05635411468776));
#88639=CARTESIAN_POINT('Ctrl Pts',(-15.6238484160462,2.9004210121165,1.89832894594602));
#88640=CARTESIAN_POINT('Ctrl Pts',(-12.9113481423434,2.10693976199442,1.74030377720429));
#88641=CARTESIAN_POINT('Ctrl Pts',(-12.0942497515145,-0.598555456962666,
1.58227860846254));
#88642=CARTESIAN_POINT('Ctrl Pts',(-13.9140505851867,-2.7608441278212,1.42425343972081));
#88643=CARTESIAN_POINT('Ctrl Pts',(-16.7193246970888,-2.41779428933264,
1.26622827097907));
#88644=CARTESIAN_POINT('Ctrl Pts',(-17.9643525134221,0.119467058919352,
1.10820310223734));
#88645=CARTESIAN_POINT('Ctrl Pts',(-16.5193009936019,2.54807939101821,0.950177933495602));
#88646=CARTESIAN_POINT('Ctrl Pts',(-13.6955198556895,2.66482978602762,0.792152764753866));
#88647=CARTESIAN_POINT('Ctrl Pts',(-12.0555235501407,0.3624138022819,0.634127596012131));
#88648=CARTESIAN_POINT('Ctrl Pts',(-13.0875701187183,-2.26713216307256,
0.476102427270394));
#88649=CARTESIAN_POINT('Ctrl Pts',(-15.855091970277,-2.84275228457381,0.318077258528659));
#88650=CARTESIAN_POINT('Ctrl Pts',(-17.8467435568307,-0.831667554258123,
0.160052089786923));
#88651=CARTESIAN_POINT('Ctrl Pts',(-17.4515005354693,1.00129455036811,0.0547019772924332));
#88652=CARTESIAN_POINT('Ctrl Pts',(-16.9107976102004,1.63370576951757,0.00202692104518772));
#88653=CARTESIAN_POINT('Ctrl Pts',(-16.913465996665,1.63598720337497,0.));
#88654=CARTESIAN_POINT('Ctrl Pts',(-16.9753029548724,1.57787564687154,-1.79744279815451E-14));
#88655=CARTESIAN_POINT('Ctrl Pts',(-17.0337487686381,1.5165933816238,-6.03303120349772E-15));
#88656=CARTESIAN_POINT('Ctrl Pts',(-17.0888052165326,1.45252874415618,5.55111512312578E-16));
#88657=CARTESIAN_POINT('Ctrl Pts',(-17.1458140481676,1.38619227911315,7.37687959281939E-15));
#88658=CARTESIAN_POINT('Ctrl Pts',(-17.1991893647422,1.31687222639765,2.56418979808053E-15));
#88659=CARTESIAN_POINT('Ctrl Pts',(-17.248906462824,1.2449490318139,4.32986979603811E-15));
#88660=CARTESIAN_POINT('Ctrl Pts',(-17.2986235609058,1.17302583723014,6.09554979399569E-15));
#88661=CARTESIAN_POINT('Ctrl Pts',(-17.3446828102636,1.0984987783709,-1.52152896675314E-14));
#88662=CARTESIAN_POINT('Ctrl Pts',(-17.3870269326305,1.02170734003083,3.60822483003176E-15));
#88663=CARTESIAN_POINT('Ctrl Pts',(-17.4058873037742,0.987503891079739,
1.2409471833211E-14));
#88664=CARTESIAN_POINT('Ctrl Pts',(-17.4240101750898,0.952850740415537,
3.4423633586001E-15));
#88665=CARTESIAN_POINT('Ctrl Pts',(-17.4413881058322,0.917775853446501,
5.38458166943201E-15));
#88666=CARTESIAN_POINT('Ctrl Pts',(-17.4513058511744,0.897758291976046,
5.60200919146819E-15));
#88667=CARTESIAN_POINT('Ctrl Pts',(-17.46098093459,0.877603346645284,-6.31318460618514E-15));
#88668=CARTESIAN_POINT('Ctrl Pts',(-17.4704117404408,0.857316068638549,
9.10382880192628E-15));
#88669=CARTESIAN_POINT('Ctrl Pts',(-17.4789447397411,0.838960126232735,
2.33069113036751E-14));
#88670=CARTESIAN_POINT('Ctrl Pts',(-17.487280152406,0.820490076428732,2.08670932036952E-15));
#88671=CARTESIAN_POINT('Ctrl Pts',(-17.4954030423954,0.801941576312626,
1.94289029309402E-15));
#88672=CARTESIAN_POINT('Ctrl Pts',(-17.5319934072411,0.718388015021337,
5.95226537027127E-15));
#88673=CARTESIAN_POINT('Ctrl Pts',(-17.5643214537022,0.633150687238601,
-2.25382967220231E-15));
#88674=CARTESIAN_POINT('Ctrl Pts',(-17.5923614732256,0.546628042515336,
-3.60822483003176E-16));
#88675=CARTESIAN_POINT('Ctrl Pts',(-17.620946200851,0.45842460061771,1.56895844496494E-15));
#88676=CARTESIAN_POINT('Ctrl Pts',(-17.6450752028303,0.368884674071994,
1.05952475446301E-14));
#88677=CARTESIAN_POINT('Ctrl Pts',(-17.6646817382536,0.27839288405896,-2.4980018054066E-15));
#88678=CARTESIAN_POINT('Ctrl Pts',(-17.6835942516363,0.191104275812135,
-1.51277830599129E-14));
#88679=CARTESIAN_POINT('Ctrl Pts',(-17.6982989201074,0.102929065387191,
2.12943541496529E-15));
#88680=CARTESIAN_POINT('Ctrl Pts',(-17.7086953392783,0.0141907563767871,
1.85129689356245E-14));
#88681=CARTESIAN_POINT('Ctrl Pts',(-17.7130454620842,-0.0229395800818436,
2.51856927009412E-14));
#88682=CARTESIAN_POINT('Ctrl Pts',(-17.7166407888389,-0.0601686928876673,
-1.4138599521916E-14));
#88683=CARTESIAN_POINT('Ctrl Pts',(-17.7194716665222,-0.097473490465065,
-9.43689570931383E-16));
#88684=CARTESIAN_POINT('Ctrl Pts',(-17.7212345778386,-0.120704819105844,
8.3900268464302E-15));
#88685=CARTESIAN_POINT('Ctrl Pts',(-17.7227010007055,-0.143965504348453,
-8.36712539882551E-16));
#88686=CARTESIAN_POINT('Ctrl Pts',(-17.7238683201636,-0.167250001102472,
-1.55431223447522E-15));
#88687=CARTESIAN_POINT('Ctrl Pts',(-17.7245283574458,-0.180415750931591,
-1.24461677816766E-15));
#88688=CARTESIAN_POINT('Ctrl Pts',(-17.7250925403628,-0.193585457009226,
2.21190068117789E-14));
#88689=CARTESIAN_POINT('Ctrl Pts',(-17.725560351488,-0.206749836717094,
1.77913239696181E-14));
#88690=CARTESIAN_POINT('Ctrl Pts',(-17.7290270823131,-0.304304936341103,
-1.4429952586954E-14));
#88691=CARTESIAN_POINT('Ctrl Pts',(-17.727212492657,-0.401699033310844,
1.01779328159474E-14));
#88692=CARTESIAN_POINT('Ctrl Pts',(-17.7200504111944,-0.49850402811495,
1.18793863634892E-14));
#88693=CARTESIAN_POINT('Ctrl Pts',(-17.7128883297318,-0.595309022919056,
1.35808399110309E-14));
#88694=CARTESIAN_POINT('Ctrl Pts',(-17.7003792037265,-0.691525995360089,
-4.23206517640884E-15));
#88695=CARTESIAN_POINT('Ctrl Pts',(-17.6824029088532,-0.786746213105208,
8.96505092384814E-15));
#88696=CARTESIAN_POINT('Ctrl Pts',(-17.6653041049695,-0.877318371632217,
2.12372231272733E-14));
#88697=CARTESIAN_POINT('Ctrl Pts',(-17.6432589215089,-0.966989690521659,
-1.54789734783363E-14));
#88698=CARTESIAN_POINT('Ctrl Pts',(-17.6165424919579,-1.05552049345646,
-7.16093850883226E-15));
#88699=CARTESIAN_POINT('Ctrl Pts',(-17.6075282349669,-1.08539122928037,
-4.33697939639551E-15));
#88700=CARTESIAN_POINT('Ctrl Pts',(-17.597981751549,-1.11513208950027,7.51971478766754E-15));
#88701=CARTESIAN_POINT('Ctrl Pts',(-17.5879123011937,-1.14473368418595,
1.20459198171829E-14));
#88702=CARTESIAN_POINT('Ctrl Pts',(-17.5808648207303,-1.16545146448869,
1.54804001547866E-14));
#88703=CARTESIAN_POINT('Ctrl Pts',(-17.5735611555087,-1.1861010242255,9.98355734190746E-15));
#88704=CARTESIAN_POINT('Ctrl Pts',(-17.5660042990016,-1.20667909739138,
3.21964677141295E-15));
#88705=CARTESIAN_POINT('Ctrl Pts',(-17.5600071842001,-1.22300983849439,
-7.11688844300461E-16));
#88706=CARTESIAN_POINT('Ctrl Pts',(-17.5538497320983,-1.23929751690581,
-1.68476118315156E-14));
#88707=CARTESIAN_POINT('Ctrl Pts',(-17.5475420423564,-1.25551905437909,
-1.72917236085368E-14));
#88708=CARTESIAN_POINT('Ctrl Pts',(-17.5132465490965,-1.34371705584084,
-1.96380407135397E-14));
#88709=CARTESIAN_POINT('Ctrl Pts',(-17.4744646972321,-1.43009866043064,
1.43722529900561E-14));
#88710=CARTESIAN_POINT('Ctrl Pts',(-17.43154004082,-1.51442123477835,-1.56819002228303E-15));
#88711=CARTESIAN_POINT('Ctrl Pts',(-17.3877761877647,-1.60039235397788,
-1.78202759780103E-14));
#88712=CARTESIAN_POINT('Ctrl Pts',(-17.33970567815,-1.68422386311186,1.23918828811253E-14));
#88713=CARTESIAN_POINT('Ctrl Pts',(-17.287637320799,-1.76565556503101,1.47937218031302E-14));
#88714=CARTESIAN_POINT('Ctrl Pts',(-17.2347023313771,-1.84844262609836,
1.72355372241975E-14));
#88715=CARTESIAN_POINT('Ctrl Pts',(-17.1776349430471,-1.92875015855361,
-1.93269493324719E-14));
#88716=CARTESIAN_POINT('Ctrl Pts',(-17.1167080019645,-2.00628981398242,
-3.01147995429574E-15));
#88717=CARTESIAN_POINT('Ctrl Pts',(-17.0750658899882,-2.05928632023397,
8.13975447041079E-15));
#88718=CARTESIAN_POINT('Ctrl Pts',(-17.0316197473168,-2.11098953163262,
1.7035584047563E-14));
#88719=CARTESIAN_POINT('Ctrl Pts',(-16.9864445796982,-2.16130036145114,
-7.91033905045424E-15));
#88720=CARTESIAN_POINT('Ctrl Pts',(-16.9750502370955,-2.1739900505392,-1.38695344460067E-14));
#88721=CARTESIAN_POINT('Ctrl Pts',(-16.9635450746152,-2.18659184950728,
8.43307920884399E-15));
#88722=CARTESIAN_POINT('Ctrl Pts',(-16.9519420608097,-2.19909166493364,
7.02216063075412E-15));
#88723=CARTESIAN_POINT('Ctrl Pts',(-16.8830341001199,-2.27332554972167,
5.36559748977514E-15));
#88724=CARTESIAN_POINT('Ctrl Pts',(-16.8105868818959,-2.34406823608281,
-1.1330177174295E-14));
#88725=CARTESIAN_POINT('Ctrl Pts',(-16.7349149176776,-2.41102639673002,
9.5062846483529E-16));
#88726=CARTESIAN_POINT('Ctrl Pts',(-16.6721146507219,-2.46659506614334,
1.11424859187091E-14));
#88727=CARTESIAN_POINT('Ctrl Pts',(-16.6070922800123,-2.51955717048407,
-1.28803071769255E-14));
#88728=CARTESIAN_POINT('Ctrl Pts',(-16.540004026716,-2.56973135519324,-2.81719092498633E-15));
#88729=CARTESIAN_POINT('Ctrl Pts',(-16.5180621279249,-2.58614133501416,
7.74249547919683E-16));
#88730=CARTESIAN_POINT('Ctrl Pts',(-16.4958990909677,-2.60225297300387,
-1.44049204168221E-14));
#88731=CARTESIAN_POINT('Ctrl Pts',(-16.4735199526406,-2.6180595362301,-9.70751257156621E-15));
#88732=CARTESIAN_POINT('Ctrl Pts',(-16.4507971782547,-2.63410881233516,
-4.9290554849159E-15));
#88733=CARTESIAN_POINT('Ctrl Pts',(-16.4278462339836,-2.6498469795081,-7.75945777818769E-15));
#88734=CARTESIAN_POINT('Ctrl Pts',(-16.4047014060989,-2.665247841993,-4.21190859967169E-15));
#88735=CARTESIAN_POINT('Ctrl Pts',(-16.3197410998749,-2.72178150901134,
4.39253025563897E-15));
#88736=CARTESIAN_POINT('Ctrl Pts',(-16.2321163764551,-2.77381420003328,
7.07843165188934E-15));
#88737=CARTESIAN_POINT('Ctrl Pts',(-16.1421182517312,-2.82103740901375,
4.30211422042248E-15));
#88738=CARTESIAN_POINT('Ctrl Pts',(-16.0583441130202,-2.86499481003348,
3.70832056865613E-15));
#88739=CARTESIAN_POINT('Ctrl Pts',(-15.972512690405,-2.90478523590151,6.95277630882711E-15));
#88740=CARTESIAN_POINT('Ctrl Pts',(-15.8848307375281,-2.94013040334526,
1.80411241501588E-15));
#88741=CARTESIAN_POINT('Ctrl Pts',(-15.8553931216106,-2.95199689844043,
-3.55731478892838E-16));
#88742=CARTESIAN_POINT('Ctrl Pts',(-15.8257467255492,-2.96336206503325,
5.1534732236655E-15));
#88743=CARTESIAN_POINT('Ctrl Pts',(-15.7959031959514,-2.9742292935539,1.50227053019591E-15));
#88744=CARTESIAN_POINT('Origin',(0.,0.,3.));
#88745=CARTESIAN_POINT('',(-11.,1.34711147906209E-15,0.));
#88746=CARTESIAN_POINT('',(-11.,1.34711147906209E-15,3.));
#88747=CARTESIAN_POINT('Origin',(0.,0.,0.));
#88748=CARTESIAN_POINT('Origin',(25.,30.,0.));
#88749=CARTESIAN_POINT('',(25.,30.,0.));
#88750=CARTESIAN_POINT('',(-25.,30.,0.));
#88751=CARTESIAN_POINT('',(25.,30.,0.));
#88752=CARTESIAN_POINT('',(-25.,30.,0.));
#88753=CARTESIAN_POINT('',(25.,30.,0.));
#88754=CARTESIAN_POINT('Origin',(25.,-30.,0.));
#88755=CARTESIAN_POINT('',(25.,-30.,0.));
#88756=CARTESIAN_POINT('',(25.,-30.,0.));
#88757=CARTESIAN_POINT('',(25.,-30.,0.));
#88758=CARTESIAN_POINT('Origin',(-25.,-30.,0.));
#88759=CARTESIAN_POINT('',(-25.,-30.,0.));
#88760=CARTESIAN_POINT('',(-25.,-30.,0.));
#88761=CARTESIAN_POINT('',(-25.,-30.,0.));
#88762=CARTESIAN_POINT('Origin',(-25.,30.,0.));
#88763=CARTESIAN_POINT('',(-25.,30.,0.));
#88764=CARTESIAN_POINT('Origin',(0.,0.,0.));
#88765=CARTESIAN_POINT('',(0.,0.,0.));
#88766=CARTESIAN_POINT('Origin',(0.,0.,201.));
#88767=CARTESIAN_POINT('',(-5.,-6.12323399573677E-16,202.));
#88768=CARTESIAN_POINT('Origin',(0.,0.,202.));
#88769=CARTESIAN_POINT('',(-5.,-6.12323399573677E-16,200.));
#88770=CARTESIAN_POINT('',(-5.,-6.12323399573677E-16,201.));
#88771=CARTESIAN_POINT('Origin',(0.,0.,200.));
#88772=CARTESIAN_POINT('Origin',(9.,0.,200.));
#88773=CARTESIAN_POINT('',(-6.,7.34788079488412E-16,200.));
#88774=CARTESIAN_POINT('Origin',(0.,0.,200.));
#88775=CARTESIAN_POINT('Origin',(5.,0.,202.));
#88776=CARTESIAN_POINT('',(-6.,-7.34788079488412E-16,202.));
#88777=CARTESIAN_POINT('Origin',(0.,0.,202.));
#88778=CARTESIAN_POINT('Origin',(0.,0.,0.));
#88779=CARTESIAN_POINT('',(-6.,-7.34788079488412E-16,203.));
#88780=CARTESIAN_POINT('Origin',(0.,0.,203.));
#88781=CARTESIAN_POINT('',(-6.,-7.34788079488412E-16,0.));
#88782=CARTESIAN_POINT('Origin',(0.,0.,0.));
#88783=CARTESIAN_POINT('',(-8.,-9.79717439317883E-16,0.));
#88784=CARTESIAN_POINT('Origin',(0.,0.,0.));
#88785=CARTESIAN_POINT('',(-6.,-7.34788079488412E-16,0.));
#88786=CARTESIAN_POINT('Origin',(0.,0.,0.));
#88787=CARTESIAN_POINT('Origin',(0.,0.,-2.));
#88788=CARTESIAN_POINT('',(-8.,-9.79717439317883E-16,-2.));
#88789=CARTESIAN_POINT('',(-8.,-9.79717439317883E-16,-2.));
#88790=CARTESIAN_POINT('Origin',(0.,0.,-2.));
#88791=CARTESIAN_POINT('Origin',(0.,0.,-2.));
#88792=CARTESIAN_POINT('Origin',(0.,0.,0.));
#88793=CARTESIAN_POINT('',(-6.,-7.34788079488412E-16,0.));
#88794=CARTESIAN_POINT('Origin',(0.,0.,203.));
#88795=CARTESIAN_POINT('',(0.,0.,0.));
#88796=CARTESIAN_POINT('Origin',(-1.,0.,1.));
#88797=CARTESIAN_POINT('',(-1.,4.89897948556636,0.));
#88798=CARTESIAN_POINT('',(-1.,4.89897948556636,1.));
#88799=CARTESIAN_POINT('',(-1.,4.89897948556636,0.));
#88800=CARTESIAN_POINT('',(-1.,8.94427190999916,0.));
#88801=CARTESIAN_POINT('',(-1.,0.,0.));
#88802=CARTESIAN_POINT('',(-1.,8.94427190999916,1.));
#88803=CARTESIAN_POINT('',(-1.,8.94427190999916,0.));
#88804=CARTESIAN_POINT('',(-1.,0.,1.));
#88805=CARTESIAN_POINT('Origin',(1.,18.,1.));
#88806=CARTESIAN_POINT('',(1.,4.89897948556636,1.));
#88807=CARTESIAN_POINT('',(1.,4.89897948556636,0.));
#88808=CARTESIAN_POINT('',(1.,4.89897948556636,0.));
#88809=CARTESIAN_POINT('',(1.,8.94427190999916,1.));
#88810=CARTESIAN_POINT('',(1.,9.,1.));
#88811=CARTESIAN_POINT('',(1.,8.94427190999916,0.));
#88812=CARTESIAN_POINT('',(1.,8.94427190999916,0.));
#88813=CARTESIAN_POINT('',(1.,9.,0.));
#88814=CARTESIAN_POINT('Origin',(0.,0.,0.));
#88815=CARTESIAN_POINT('Origin',(0.,0.,0.));
#88816=CARTESIAN_POINT('Origin',(0.,0.,0.));
#88817=CARTESIAN_POINT('Origin',(0.,0.,0.));
#88818=CARTESIAN_POINT('Origin',(0.,0.,1.));
#88819=CARTESIAN_POINT('Origin',(0.,0.,0.));
#88820=CARTESIAN_POINT('Origin',(0.,0.,1.));
#88821=CARTESIAN_POINT('Origin',(0.,0.,1.));
#88822=CARTESIAN_POINT('',(0.,0.,0.));
#88823=CARTESIAN_POINT('Origin',(0.,0.,0.));
#88824=CARTESIAN_POINT('',(-6.,-7.34788079488412E-16,0.));
#88825=CARTESIAN_POINT('Origin',(0.,0.,0.));
#88826=CARTESIAN_POINT('',(-6.,-7.34788079488412E-16,20.));
#88827=CARTESIAN_POINT('',(-6.,-7.34788079488412E-16,0.));
#88828=CARTESIAN_POINT('Origin',(0.,0.,20.));
#88829=CARTESIAN_POINT('Origin',(0.,0.,0.));
#88830=CARTESIAN_POINT('',(-8.,-9.79717439317883E-16,20.));
#88831=CARTESIAN_POINT('Origin',(0.,0.,20.));
#88832=CARTESIAN_POINT('',(-8.,-9.79717439317883E-16,0.));
#88833=CARTESIAN_POINT('',(-8.,-9.79717439317883E-16,0.));
#88834=CARTESIAN_POINT('Origin',(0.,0.,0.));
#88835=CARTESIAN_POINT('Origin',(0.,0.,20.));
#88836=CARTESIAN_POINT('Origin',(0.,0.,0.));
#88837=CARTESIAN_POINT('',(0.,0.,0.));
#88838=CARTESIAN_POINT('Origin',(0.,0.,0.));
#88839=CARTESIAN_POINT('',(-5.,-6.12323399573677E-16,0.));
#88840=CARTESIAN_POINT('Origin',(0.,0.,0.));
#88841=CARTESIAN_POINT('',(-5.,-6.12323399573677E-16,2.));
#88842=CARTESIAN_POINT('',(-5.,-6.12323399573677E-16,0.));
#88843=CARTESIAN_POINT('Origin',(0.,0.,2.));
#88844=CARTESIAN_POINT('Origin',(0.,0.,0.));
#88845=CARTESIAN_POINT('',(-10.,-1.22464679914735E-15,2.));
#88846=CARTESIAN_POINT('Origin',(0.,0.,2.));
#88847=CARTESIAN_POINT('',(-10.,-1.22464679914735E-15,0.));
#88848=CARTESIAN_POINT('',(-10.,-1.22464679914735E-15,0.));
#88849=CARTESIAN_POINT('Origin',(0.,0.,0.));
#88850=CARTESIAN_POINT('Origin',(0.,0.,2.));
#88851=CARTESIAN_POINT('Origin',(0.,0.,0.));
#88852=CARTESIAN_POINT('',(0.,0.,0.));
#88853=CARTESIAN_POINT('Origin',(0.,0.,-1.84858989190503));
#88854=CARTESIAN_POINT('',(-2.36542648444351,0.173076888096584,0.838413605944557));
#88855=CARTESIAN_POINT('',(-2.36542649454111,0.173076750093528,0.639821592488593));
#88856=CARTESIAN_POINT('',(-2.36542649454111,0.173076750093529,-1.84858989190503));
#88857=CARTESIAN_POINT('',(-1.35150067398999,-1.94901102888224,-5.43618969284232E-15));
#88858=CARTESIAN_POINT('Ctrl Pts',(-2.36542648444351,0.173076888096584,
0.838413605944556));
#88859=CARTESIAN_POINT('Ctrl Pts',(-2.35882845273757,0.263251602433591,
0.831953464375971));
#88860=CARTESIAN_POINT('Ctrl Pts',(-2.34707785797561,0.352996265264053,
0.825376328096348));
#88861=CARTESIAN_POINT('Ctrl Pts',(-2.30344086365932,0.583117657947324,
0.808270841295367));
#88862=CARTESIAN_POINT('Ctrl Pts',(-2.26386739771479,0.721649711978628,
0.797725648659815));
#88863=CARTESIAN_POINT('Ctrl Pts',(-2.20518235143571,0.873340955132987,
0.786412943593282));
#88864=CARTESIAN_POINT('Ctrl Pts',(-2.19816898024188,0.8908461245749,0.78511146551529));
#88865=CARTESIAN_POINT('Ctrl Pts',(-2.18800275925427,0.91536938434873,0.783295708307795));
#88866=CARTESIAN_POINT('Ctrl Pts',(-2.18502363822882,0.922458068899643,
0.782771737102728));
#88867=CARTESIAN_POINT('Ctrl Pts',(-2.17995655497133,0.934352681901471,
0.781894180782981));
#88868=CARTESIAN_POINT('Ctrl Pts',(-2.17788706398935,0.939166361277973,
0.781539496599892));
#88869=CARTESIAN_POINT('Ctrl Pts',(-2.17363202058509,0.948973980764961,
0.780817837826489));
#88870=CARTESIAN_POINT('Ctrl Pts',(-2.17144517915015,0.953967301624584,
0.780450944257678));
#88871=CARTESIAN_POINT('Ctrl Pts',(-2.16583343935226,0.966661579005291,
0.779519429431435));
#88872=CARTESIAN_POINT('Ctrl Pts',(-2.16238463595257,0.974351983093089,
0.778956250237148));
#88873=CARTESIAN_POINT('Ctrl Pts',(-2.14823818374022,1.00545173545004,0.776682784415733));
#88874=CARTESIAN_POINT('Ctrl Pts',(-2.13720033304501,1.02870567134393,0.774992118228455));
#88875=CARTESIAN_POINT('Ctrl Pts',(-2.03678114929324,1.23166671347637,0.760277761846239));
#88876=CARTESIAN_POINT('Ctrl Pts',(-1.92529086506381,1.39955674033437,0.748342490018322));
#88877=CARTESIAN_POINT('Ctrl Pts',(-1.71647613141014,1.64101857339006,0.728609169452957));
#88878=CARTESIAN_POINT('Ctrl Pts',(-1.63239079233033,1.72468166692776,0.721161418709966));
#88879=CARTESIAN_POINT('Ctrl Pts',(-1.52835819326624,1.81374247090932,0.712216477780571));
#88880=CARTESIAN_POINT('Ctrl Pts',(-1.51416036452442,1.82561191830619,0.711001326633681));
#88881=CARTESIAN_POINT('Ctrl Pts',(-1.4908071680934,1.84467546574982,0.709010763794069));
#88882=CARTESIAN_POINT('Ctrl Pts',(-1.48173497720693,1.85197058170622,0.708239442578538));
#88883=CARTESIAN_POINT('Ctrl Pts',(-1.46543003483459,1.86488518675399,0.706856478940121));
#88884=CARTESIAN_POINT('Ctrl Pts',(-1.45821769512675,1.87053016450956,0.706245870875885));
#88885=CARTESIAN_POINT('Ctrl Pts',(-1.44288154591547,1.88239090967805,0.704949770501894));
#88886=CARTESIAN_POINT('Ctrl Pts',(-1.43474987976872,1.88859616360747,0.704263879562391));
#88887=CARTESIAN_POINT('Ctrl Pts',(-1.41293136818131,1.90502357734161,0.702426922128258));
#88888=CARTESIAN_POINT('Ctrl Pts',(-1.39917400904025,1.91515063302255,0.701272178138156));
#88889=CARTESIAN_POINT('Ctrl Pts',(-1.33085533810299,1.96431227585873,0.695553841641458));
#88890=CARTESIAN_POINT('Ctrl Pts',(-1.27476918107105,2.00116481582797,0.690908081597918));
#88891=CARTESIAN_POINT('Ctrl Pts',(-1.06467100998372,2.12679522624806,0.673664136910677));
#88892=CARTESIAN_POINT('Ctrl Pts',(-0.902386257657863,2.20056026983934,
0.660588977907503));
#88893=CARTESIAN_POINT('Ctrl Pts',(-0.640355477985702,2.2857645632085,0.640556214998197));
#88894=CARTESIAN_POINT('Ctrl Pts',(-0.545495406345934,2.31024116793884,
0.633521162604947));
#88895=CARTESIAN_POINT('Ctrl Pts',(-0.437029945150103,2.33117163427879,
0.625900456969698));
#88896=CARTESIAN_POINT('Ctrl Pts',(-0.424657044275813,2.33345725773121,
0.625037320823393));
#88897=CARTESIAN_POINT('Ctrl Pts',(-0.405925635001334,2.33676355173499,
0.623740524895043));
#88898=CARTESIAN_POINT('Ctrl Pts',(-0.399580439684234,2.33785692303564,
0.623302954475343));
#88899=CARTESIAN_POINT('Ctrl Pts',(-0.388175393850692,2.33977439198356,
0.622519624565479));
#88900=CARTESIAN_POINT('Ctrl Pts',(-0.383117296047,2.34060792971696,0.622173346695847));
#88901=CARTESIAN_POINT('Ctrl Pts',(-0.372030164872043,2.34239810469478,
0.621416781989657));
#88902=CARTESIAN_POINT('Ctrl Pts',(-0.366000136548875,2.34334786718063,
0.621006884778632));
#88903=CARTESIAN_POINT('Ctrl Pts',(-0.348772092038685,2.34599325616917,
0.619840126917685));
#88904=CARTESIAN_POINT('Ctrl Pts',(-0.337565315213134,2.34763199859982,
0.619086378997433));
#88905=CARTESIAN_POINT('Ctrl Pts',(-0.261233449977285,2.35823593739986,
0.613985286134159));
#88906=CARTESIAN_POINT('Ctrl Pts',(-0.195765000908738,2.36457132035811,
0.609772428655903));
#88907=CARTESIAN_POINT('Ctrl Pts',(0.110174716895957,2.38138012782496,0.590488052955399));
#88908=CARTESIAN_POINT('Ctrl Pts',(0.35106720268076,2.35793855776526,0.576305692927121));
#88909=CARTESIAN_POINT('Ctrl Pts',(0.624832421383487,2.28834645913277,0.558176642545399));
#88910=CARTESIAN_POINT('Ctrl Pts',(0.66505986667524,2.2769804787425,0.555464417224489));
#88911=CARTESIAN_POINT('Ctrl Pts',(0.719308968142765,2.26009256154776,0.551730696707469));
#88912=CARTESIAN_POINT('Ctrl Pts',(0.73361076822872,2.25549085606611,0.550739095864994));
#88913=CARTESIAN_POINT('Ctrl Pts',(0.756231382968104,2.24797460700757,0.549158722690731));
#88914=CARTESIAN_POINT('Ctrl Pts',(0.76457949868733,2.24514897611453,0.54857287809079));
#88915=CARTESIAN_POINT('Ctrl Pts',(0.781634695848507,2.23927005935689,0.547370549740896));
#88916=CARTESIAN_POINT('Ctrl Pts',(0.790340086659133,2.2362123646376,0.546753928949542));
#88917=CARTESIAN_POINT('Ctrl Pts',(0.810374353528146,2.22904390027971,0.545327993926065));
#88918=CARTESIAN_POINT('Ctrl Pts',(0.821690101297483,2.22489745164558,0.544517506736585));
#88919=CARTESIAN_POINT('Ctrl Pts',(0.857220114182346,2.21157010968876,0.541956310211719));
#88920=CARTESIAN_POINT('Ctrl Pts',(0.881315191753872,2.20207904360719,0.540195309000516));
#88921=CARTESIAN_POINT('Ctrl Pts',(1.0005066872654,2.15285989296877,0.531360078603607));
#88922=CARTESIAN_POINT('Ctrl Pts',(1.09308567096607,2.10736276147444,0.524093208452545));
#88923=CARTESIAN_POINT('Ctrl Pts',(1.30993455767744,1.98265305703226,0.506098161896216));
#88924=CARTESIAN_POINT('Ctrl Pts',(1.43036384860764,1.89760302833471,0.495243843136743));
#88925=CARTESIAN_POINT('Ctrl Pts',(1.56141150895823,1.78545130440902,0.482770085121858));
#88926=CARTESIAN_POINT('Ctrl Pts',(1.58042934154114,1.76863942826671,0.480942538592971));
#88927=CARTESIAN_POINT('Ctrl Pts',(1.63999568589212,1.7142542764494,0.475171133281602));
#88928=CARTESIAN_POINT('Ctrl Pts',(1.67950573937826,1.67556413927506,0.471271134091533));
#88929=CARTESIAN_POINT('Ctrl Pts',(1.7246894941321,1.62811209320835,0.466759933912571));
#88930=CARTESIAN_POINT('Ctrl Pts',(1.73170022601144,1.62065331763146,0.466058451112532));
#88931=CARTESIAN_POINT('Ctrl Pts',(1.74305505568855,1.60841500916403,0.464920146687879));
#88932=CARTESIAN_POINT('Ctrl Pts',(1.74742821756293,1.60366280615676,0.464481213599434));
#88933=CARTESIAN_POINT('Ctrl Pts',(1.7552192195573,1.59512681330722,0.463698375253306));
#88934=CARTESIAN_POINT('Ctrl Pts',(1.75864434363002,1.5913497836382,0.463353922941777));
#88935=CARTESIAN_POINT('Ctrl Pts',(1.76607254010742,1.58310512213734,0.46260628031285));
#88936=CARTESIAN_POINT('Ctrl Pts',(1.77007085835728,1.57863333396174,0.462203446979245));
#88937=CARTESIAN_POINT('Ctrl Pts',(1.7813879982382,1.56587899441908,0.461061914284783));
#88938=CARTESIAN_POINT('Ctrl Pts',(1.7886660715918,1.55756024659359,0.460326205678364));
#88939=CARTESIAN_POINT('Ctrl Pts',(1.83615320297324,1.50251120150658,0.455513021599716));
#88940=CARTESIAN_POINT('Ctrl Pts',(1.87458942508493,1.45427457315995,0.451555465202916));
#88941=CARTESIAN_POINT('Ctrl Pts',(2.02473002043905,1.24999109880192,0.435573844947295));
#88942=CARTESIAN_POINT('Ctrl Pts',(2.11918051815449,1.0821706007713,0.424169801814584));
#88943=CARTESIAN_POINT('Ctrl Pts',(2.20767374851595,0.867744834740668,0.40968795284765));
#88944=CARTESIAN_POINT('Ctrl Pts',(2.22202163645874,0.830315657834007,0.407165773223575));
#88945=CARTESIAN_POINT('Ctrl Pts',(2.25365109097284,0.741102847970854,0.401145749575422));
#88946=CARTESIAN_POINT('Ctrl Pts',(2.27010617083441,0.689052898042909,0.397626654700763));
#88947=CARTESIAN_POINT('Ctrl Pts',(2.2891817487847,0.620578464971442,0.392965623320821));
#88948=CARTESIAN_POINT('Ctrl Pts',(2.29344660808414,0.604626614392158,0.391877642763972));
#88949=CARTESIAN_POINT('Ctrl Pts',(2.30003944373639,0.578893496662921,0.39011852379195));
#88950=CARTESIAN_POINT('Ctrl Pts',(2.30247244349693,0.56913949503013,0.389450817251523));
#88951=CARTESIAN_POINT('Ctrl Pts',(2.30699117746388,0.550520395889349,0.388174365520821));
#88952=CARTESIAN_POINT('Ctrl Pts',(2.30908800998514,0.541658155390165,0.387565993651542));
#88953=CARTESIAN_POINT('Ctrl Pts',(2.31376685751924,0.521362052308742,0.386170753644772));
#88954=CARTESIAN_POINT('Ctrl Pts',(2.31631523547038,0.509920760324331,0.385382812076915));
#88955=CARTESIAN_POINT('Ctrl Pts',(2.32393240149492,0.474486666160826,0.382937883633644));
#88956=CARTESIAN_POINT('Ctrl Pts',(2.32871383644352,0.450434447535796,0.381271713575045));
#88957=CARTESIAN_POINT('Ctrl Pts',(2.34992725871791,0.334337903573334,0.37319502298379));
#88958=CARTESIAN_POINT('Ctrl Pts',(2.36127769125885,0.241461352893806,0.366625517186806));
#88959=CARTESIAN_POINT('Ctrl Pts',(2.37360181955217,0.0445715376189227,
0.352488068927495));
#88960=CARTESIAN_POINT('Ctrl Pts',(2.3732781772528,-0.0593322762628842,
0.344903769168617));
#88961=CARTESIAN_POINT('Ctrl Pts',(2.35770452936616,-0.285579165871283,
0.328331051913376));
#88962=CARTESIAN_POINT('Ctrl Pts',(2.33972489181835,-0.407455486345739,
0.31936501879041));
#88963=CARTESIAN_POINT('Ctrl Pts',(2.30811900222491,-0.546031135884901,
0.309473923804203));
#88964=CARTESIAN_POINT('Ctrl Pts',(2.30364389567164,-0.5646133106769,0.308154267159724));
#88965=CARTESIAN_POINT('Ctrl Pts',(2.29704910606919,-0.590612303618463,
0.306319206564952));
#88966=CARTESIAN_POINT('Ctrl Pts',(2.29511728484466,-0.598075364753959,
0.305793765318625));
#88967=CARTESIAN_POINT('Ctrl Pts',(2.29193500142203,-0.610126728461225,
0.304947560987187));
#88968=CARTESIAN_POINT('Ctrl Pts',(2.29070708362945,-0.614720858579664,
0.304625514646067));
#88969=CARTESIAN_POINT('Ctrl Pts',(2.28807190141162,-0.62446257965839,0.303943810009646));
#88970=CARTESIAN_POINT('Ctrl Pts',(2.28666106761748,-0.629609166638432,
0.303584362816388));
#88971=CARTESIAN_POINT('Ctrl Pts',(2.28312684153687,-0.642333099951298,
0.302697332886097));
#88972=CARTESIAN_POINT('Ctrl Pts',(2.28098306636702,-0.649904793966007,
0.302170920000501));
#88973=CARTESIAN_POINT('Ctrl Pts',(2.2728571536084,-0.678069517800896,0.300217675204858));
#88974=CARTESIAN_POINT('Ctrl Pts',(2.26663328099306,-0.698592557584431,
0.298804115327949));
#88975=CARTESIAN_POINT('Ctrl Pts',(2.22090970768154,-0.842315911662801,
0.28895511550237));
#88976=CARTESIAN_POINT('Ctrl Pts',(2.17166027737835,-0.962204067261257,
0.280993437826904));
#88977=CARTESIAN_POINT('Ctrl Pts',(2.02930351392623,-1.24135426858414,0.261780269272243));
#88978=CARTESIAN_POINT('Ctrl Pts',(1.92697114560946,-1.39492141482945,0.250579747106606));
#88979=CARTESIAN_POINT('Ctrl Pts',(1.78956967640727,-1.55674119882285,0.236813504223705));
#88980=CARTESIAN_POINT('Ctrl Pts',(1.77082288055304,-1.57803326969538,0.234959336828218));
#88981=CARTESIAN_POINT('Ctrl Pts',(1.74389545159007,-1.60753248998782,0.232326356996511));
#88982=CARTESIAN_POINT('Ctrl Pts',(1.73602919827401,-1.61602433991634,0.231560708771867));
#88983=CARTESIAN_POINT('Ctrl Pts',(1.72221465838979,-1.63072026991237,0.230221975230984));
#88984=CARTESIAN_POINT('Ctrl Pts',(1.71629417530401,-1.63695028292761,0.229650082047395));
#88985=CARTESIAN_POINT('Ctrl Pts',(1.70382807447056,-1.64992615144839,0.22844966545211));
#88986=CARTESIAN_POINT('Ctrl Pts',(1.69727596715171,-1.65666553641231,0.227820866844937));
#88987=CARTESIAN_POINT('Ctrl Pts',(1.6815714904615,-1.67262793607172,0.22631865812438));
#88988=CARTESIAN_POINT('Ctrl Pts',(1.67238313005619,-1.68181495554965,0.225443679232295));
#88989=CARTESIAN_POINT('Ctrl Pts',(1.64091038779628,-1.71277015315762,0.222459499243495));
#88990=CARTESIAN_POINT('Ctrl Pts',(1.61827362684124,-1.73417381100087,0.220334677545939));
#88991=CARTESIAN_POINT('Ctrl Pts',(1.56289211756675,-1.78450975125133,0.215184630203508));
#88992=CARTESIAN_POINT('Ctrl Pts',(1.52975757961476,-1.81299425027077,0.212142169107271));
#88993=CARTESIAN_POINT('Ctrl Pts',(1.295593761634,-2.0033049568681,0.190900568318592));
#88994=CARTESIAN_POINT('Ctrl Pts',(1.07015773753808,-2.13225727392394,0.171479134689879));
#88995=CARTESIAN_POINT('Ctrl Pts',(0.804987994816205,-2.23110228262024,
0.151681448966647));
#88996=CARTESIAN_POINT('Ctrl Pts',(0.781424686826433,-2.23946392045831,
0.149948750330738));
#88997=CARTESIAN_POINT('Ctrl Pts',(0.749661120413222,-2.25017306405519,
0.147652428160719));
#88998=CARTESIAN_POINT('Ctrl Pts',(0.74157506083843,-2.25285087131227,0.147071243707183));
#88999=CARTESIAN_POINT('Ctrl Pts',(0.728260020849596,-2.25718086823613,
0.146119989156702));
#89000=CARTESIAN_POINT('Ctrl Pts',(0.723039488203981,-2.2588585681277,0.145748474576035));
#89001=CARTESIAN_POINT('Ctrl Pts',(0.712766643234138,-2.26212064423224,
0.14502032287958));
#89002=CARTESIAN_POINT('Ctrl Pts',(0.707714805397492,-2.26370622042107,
0.144663612332407));
#89003=CARTESIAN_POINT('Ctrl Pts',(0.697498787849602,-2.26687509092163,
0.143944942793365));
#89004=CARTESIAN_POINT('Ctrl Pts',(0.692334423965896,-2.26845768831963,
0.14358302475386));
#89005=CARTESIAN_POINT('Ctrl Pts',(0.673757270738551,-2.27408122813314,
0.14228594615369));
#89006=CARTESIAN_POINT('Ctrl Pts',(0.660313820056548,-2.27802106529962,
0.141356294878642));
#89007=CARTESIAN_POINT('Ctrl Pts',(0.531945423148506,-2.31440977868095,
0.132557624836019));
#89008=CARTESIAN_POINT('Ctrl Pts',(0.414742458143056,-2.33825900818764,
0.125115973224835));
#89009=CARTESIAN_POINT('Ctrl Pts',(0.102061160892701,-2.37762055134687,
0.105654159096787));
#89010=CARTESIAN_POINT('Ctrl Pts',(-0.0943608051712325,-2.37793690014678,
0.0937590278414453));
#89011=CARTESIAN_POINT('Ctrl Pts',(-0.315165659561377,-2.35086916583635,
0.0793014817004178));
#89012=CARTESIAN_POINT('Ctrl Pts',(-0.341688623976874,-2.34716084218601,
0.0775482835218531));
#89013=CARTESIAN_POINT('Ctrl Pts',(-0.380179456179028,-2.3411130076066,
0.0749772556349703));
#89014=CARTESIAN_POINT('Ctrl Pts',(-0.39220169013825,-2.33912897428847,
0.074170410657453));
#89015=CARTESIAN_POINT('Ctrl Pts',(-0.413456569779718,-2.3354528091372,
0.0727369375012271));
#89016=CARTESIAN_POINT('Ctrl Pts',(-0.422695529542975,-2.33379832972636,
0.0721114937516175));
#89017=CARTESIAN_POINT('Ctrl Pts',(-0.441880640723978,-2.33024507093785,
0.0708077251933305));
#89018=CARTESIAN_POINT('Ctrl Pts',(-0.451824921733991,-2.32833735226487,
0.0701291322535876));
#89019=CARTESIAN_POINT('Ctrl Pts',(-0.477568297848316,-2.3232275920694,
0.0683649695055473));
#89020=CARTESIAN_POINT('Ctrl Pts',(-0.493347290089823,-2.31992809219195,
0.0672763598045879));
#89021=CARTESIAN_POINT('Ctrl Pts',(-0.562269321199218,-2.30478107048403,
0.0624884294285706));
#89022=CARTESIAN_POINT('Ctrl Pts',(-0.615025227240541,-2.29126727035618,
0.0587370028246758));
#89023=CARTESIAN_POINT('Ctrl Pts',(-0.757823346299244,-2.24940155808092,
0.0483345334727881));
#89024=CARTESIAN_POINT('Ctrl Pts',(-0.846705737141405,-2.21747367686783,
0.0415806383145637));
#89025=CARTESIAN_POINT('Ctrl Pts',(-1.08025369384199,-2.11748770243054,
0.0231531306418185));
#89026=CARTESIAN_POINT('Ctrl Pts',(-1.22031304748997,-2.03998032716046,
0.0113379304209554));
#89027=CARTESIAN_POINT('Ctrl Pts',(-1.35150067398999,-1.94901102888224,
-5.43618969284232E-15));
#89028=CARTESIAN_POINT('',(1.37702479013102,-1.93106208855765,0.));
#89029=CARTESIAN_POINT('Origin',(0.,0.,0.));
#89030=CARTESIAN_POINT('Ctrl Pts',(1.377024790131,-1.93106208855766,8.88178419700125E-16));
#89031=CARTESIAN_POINT('Ctrl Pts',(1.44323442930785,-1.88384852922553,0.00545688894094474));
#89032=CARTESIAN_POINT('Ctrl Pts',(1.50706076889383,-1.83319246581089,0.0109137778818887));
#89033=CARTESIAN_POINT('Ctrl Pts',(1.56814231099797,-1.77936161444434,0.0163706668228325));
#89034=CARTESIAN_POINT('Ctrl Pts',(1.62918664869343,-1.7255635511333,0.0218242320047606));
#89035=CARTESIAN_POINT('Ctrl Pts',(1.68748918816346,-1.66859483606143,0.0272777971866886));
#89036=CARTESIAN_POINT('Ctrl Pts',(1.74272158951512,-1.60876335237284,0.0327313623686167));
#89037=CARTESIAN_POINT('Ctrl Pts',(1.79794854973166,-1.54893776289089,0.0381843903009549));
#89038=CARTESIAN_POINT('Ctrl Pts',(1.85010566943635,-1.48625027976053,0.0436374182332935));
#89039=CARTESIAN_POINT('Ctrl Pts',(1.89890209573401,-1.42104500045459,0.0490904461656316));
#89040=CARTESIAN_POINT('Ctrl Pts',(1.94769763273321,-1.35584090949293,0.0545433747183692));
#89041=CARTESIAN_POINT('Ctrl Pts',(1.99313233564526,-1.28811946349422,0.0599963032711064));
#89042=CARTESIAN_POINT('Ctrl Pts',(2.03495704214576,-1.218256089302,0.065449231823844));
#89043=CARTESIAN_POINT('Ctrl Pts',(2.07679126035066,-1.14837682689872,0.0709034004724213));
#89044=CARTESIAN_POINT('Ctrl Pts',(2.11501362448989,-1.07635504271482,0.0763575691209986));
#89045=CARTESIAN_POINT('Ctrl Pts',(2.1494200941166,-1.00259230074232,0.081811737769576));
#89046=CARTESIAN_POINT('Ctrl Pts',(2.18384284291776,-0.928794658457252,
0.0872684870189499));
#89047=CARTESIAN_POINT('Ctrl Pts',(2.21444592129525,-0.853254816187775,
0.0927252362683234));
#89048=CARTESIAN_POINT('Ctrl Pts',(2.24107318383604,-0.776394904150594,
0.0981819855176973));
#89049=CARTESIAN_POINT('Ctrl Pts',(2.26774034407289,-0.699419826936176,
0.103646911038391));
#89050=CARTESIAN_POINT('Ctrl Pts',(2.29041964825811,-0.621121144024271,
0.109111836559085));
#89051=CARTESIAN_POINT('Ctrl Pts',(2.30900469105276,-0.541936711430734,
0.114576762079779));
#89052=CARTESIAN_POINT('Ctrl Pts',(2.32760431554601,-0.462690151268103,
0.120045975343995));
#89053=CARTESIAN_POINT('Ctrl Pts',(2.34210319909487,-0.382556886917718,
0.125515188608211));
#89054=CARTESIAN_POINT('Ctrl Pts',(2.35244643305339,-0.301983181840315,
0.130984401872427));
#89055=CARTESIAN_POINT('Ctrl Pts',(2.3628098942255,-0.221251906939983,0.136464310722315));
#89056=CARTESIAN_POINT('Ctrl Pts',(2.36900143325511,-0.140078906893982,
0.141944219572203));
#89057=CARTESIAN_POINT('Ctrl Pts',(2.3710181814828,-0.0589138827273241,
0.147424128422091));
#89058=CARTESIAN_POINT('Ctrl Pts',(2.37242499804373,-0.00229585842526928,
0.151246730776019));
#89059=CARTESIAN_POINT('Ctrl Pts',(2.37180146375247,0.0543182630853344,
0.155069333129946));
#89060=CARTESIAN_POINT('Ctrl Pts',(2.36916154938288,0.110777323607845,0.158891935483873));
#89061=CARTESIAN_POINT('Ctrl Pts',(2.36551681281839,0.188726216440715,0.164169522791762));
#89062=CARTESIAN_POINT('Ctrl Pts',(2.35801245769879,0.266674309576874,0.169447110099651));
#89063=CARTESIAN_POINT('Ctrl Pts',(2.34664078348069,0.344202114759797,0.17472469740754));
#89064=CARTESIAN_POINT('Ctrl Pts',(2.33528742825447,0.421605027934216,0.179993782882088));
#89065=CARTESIAN_POINT('Ctrl Pts',(2.32007918549393,0.498588527466604,0.185262868356636));
#89066=CARTESIAN_POINT('Ctrl Pts',(2.30106032801871,0.5747342249409,0.190531953831185));
#89067=CARTESIAN_POINT('Ctrl Pts',(2.28192207585617,0.651357942283229,0.195834117045208));
#89068=CARTESIAN_POINT('Ctrl Pts',(2.25892520061864,0.727132808352569,0.201136280259231));
#89069=CARTESIAN_POINT('Ctrl Pts',(2.23216780058896,0.801638929015961,0.206438443473254));
#89070=CARTESIAN_POINT('Ctrl Pts',(2.20563356521996,0.875523646511697,0.211696385071828));
#89071=CARTESIAN_POINT('Ctrl Pts',(2.17540145399492,0.948160240731734,0.216954326670403));
#89072=CARTESIAN_POINT('Ctrl Pts',(2.14161761336225,1.01915261891268,0.222212268268977));
#89073=CARTESIAN_POINT('Ctrl Pts',(2.10784804477187,1.09011500623988,0.227467988640969));
#89074=CARTESIAN_POINT('Ctrl Pts',(2.07052992972339,1.1594341230509,0.232723709012963));
#89075=CARTESIAN_POINT('Ctrl Pts',(2.02985724532268,1.22673453775094,0.237979429384955));
#89076=CARTESIAN_POINT('Ctrl Pts',(1.98918841914434,1.29402856831458,0.243234651197824));
#89077=CARTESIAN_POINT('Ctrl Pts',(1.94516590451668,1.35930386698306,0.248489873010692));
#89078=CARTESIAN_POINT('Ctrl Pts',(1.89802843584865,1.42221169985693,0.25374509482356));
#89079=CARTESIAN_POINT('Ctrl Pts',(1.8501613506344,1.48609325060424,0.259081659502242));
#89080=CARTESIAN_POINT('Ctrl Pts',(1.79908234605505,1.54753299939798,0.264418224180925));
#89081=CARTESIAN_POINT('Ctrl Pts',(1.74508434773943,1.60620007526299,0.269754788859607));
#89082=CARTESIAN_POINT('Ctrl Pts',(1.6918351201776,1.66405363596099,0.275017353321953));
#89083=CARTESIAN_POINT('Ctrl Pts',(1.63574774002439,1.719210645093,0.280279917784299));
#89084=CARTESIAN_POINT('Ctrl Pts',(1.57713928335961,1.77139203548619,0.285542482246645));
#89085=CARTESIAN_POINT('Ctrl Pts',(1.51729463134653,1.8246740587188,0.290916047033495));
#89086=CARTESIAN_POINT('Ctrl Pts',(1.45482174846241,1.87485317119378,0.296289611820345));
#89087=CARTESIAN_POINT('Ctrl Pts',(1.39009065932477,1.92167791821576,0.301663176607196));
#89088=CARTESIAN_POINT('Ctrl Pts',(1.32535957018712,1.96850266523773,0.307036741394046));
#89089=CARTESIAN_POINT('Ctrl Pts',(1.25837075515963,2.01197282475023,0.312410306180897));
#89090=CARTESIAN_POINT('Ctrl Pts',(1.18952013501392,2.05188691474371,0.317783870967748));
#89091=CARTESIAN_POINT('Ctrl Pts',(1.12110087339485,2.09155093751898,0.323123769638238));
#89092=CARTESIAN_POINT('Ctrl Pts',(1.05056820942786,2.12786295700445,0.328463668308728));
#89093=CARTESIAN_POINT('Ctrl Pts',(0.97828367652601,2.16059230553632,0.333803566979218));
#89094=CARTESIAN_POINT('Ctrl Pts',(0.906103429712095,2.19327443489721,0.339135761689816));
#89095=CARTESIAN_POINT('Ctrl Pts',(0.832176755690867,2.22238396760182,0.344467956400415));
#89096=CARTESIAN_POINT('Ctrl Pts',(0.756891277378829,2.2477352283416,0.349800151111013));
#89097=CARTESIAN_POINT('Ctrl Pts',(0.681693782616492,2.27305686193469,0.355126114269008));
#89098=CARTESIAN_POINT('Ctrl Pts',(0.605141080097607,2.29462880434646,0.360452077427004));
#89099=CARTESIAN_POINT('Ctrl Pts',(0.527640948372251,2.31231336373356,0.365778040584999));
#89100=CARTESIAN_POINT('Ctrl Pts',(0.45019049891151,2.32998658625014,0.371100589478978));
#89101=CARTESIAN_POINT('Ctrl Pts',(0.371794280151321,2.34377726891592,0.376423138372958));
#89102=CARTESIAN_POINT('Ctrl Pts',(0.292874274958876,2.35359782494107,0.381745687266938));
#89103=CARTESIAN_POINT('Ctrl Pts',(0.213980483290613,2.36341511903811,0.387066468259816));
#89104=CARTESIAN_POINT('Ctrl Pts',(0.134563713958973,2.36926484766798,0.392387249252693));
#89105=CARTESIAN_POINT('Ctrl Pts',(0.0550537088996654,2.37111095304214,
0.397708030245571));
#89106=CARTESIAN_POINT('Ctrl Pts',(-0.0244544470979098,2.37295701548381,
0.403028687499902));
#89107=CARTESIAN_POINT('Ctrl Pts',(-0.104055367419461,2.37079963020706,
0.408349344754232));
#89108=CARTESIAN_POINT('Ctrl Pts',(-0.183318127710723,2.36465484300619,
0.413670002008563));
#89109=CARTESIAN_POINT('Ctrl Pts',(-0.26265795540767,2.35850408121137,0.418995832552968));
#89110=CARTESIAN_POINT('Ctrl Pts',(-0.341658499354637,2.34835820866443,
0.424321663097373));
#89111=CARTESIAN_POINT('Ctrl Pts',(-0.419893374233965,2.33428524751677,
0.429647493641779));
#89112=CARTESIAN_POINT('Ctrl Pts',(-0.498164825645014,2.32020570694899,
0.434975814129578));
#89113=CARTESIAN_POINT('Ctrl Pts',(-0.575669438982421,2.30219552530526,
0.440304134617377));
#89114=CARTESIAN_POINT('Ctrl Pts',(-0.651992935900375,2.28037349441621,
0.445632455105176));
#89115=CARTESIAN_POINT('Ctrl Pts',(-0.728452664517911,2.25851251284387,
0.450970286244154));
#89116=CARTESIAN_POINT('Ctrl Pts',(-0.803726620498811,2.23282623700074,
0.456308117383132));
#89117=CARTESIAN_POINT('Ctrl Pts',(-0.877417743213549,2.20348273566961,
0.46164594852211));
#89118=CARTESIAN_POINT('Ctrl Pts',(-0.94658235809367,2.17594167110125,0.466655901165276));
#89119=CARTESIAN_POINT('Ctrl Pts',(-1.01435252431405,2.14517947154205,0.471665853808442));
#89120=CARTESIAN_POINT('Ctrl Pts',(-1.08042043865333,2.1113715301292,0.476675806451608));
#89121=CARTESIAN_POINT('Ctrl Pts',(-1.15085759099418,2.07532778418321,0.482017079913562));
#89122=CARTESIAN_POINT('Ctrl Pts',(-1.21961720760008,2.03568988249139,0.487358353375516));
#89123=CARTESIAN_POINT('Ctrl Pts',(-1.28630969075306,1.99263781003342,0.492699626837469));
#89124=CARTESIAN_POINT('Ctrl Pts',(-1.35290829972811,1.94964633627741,0.498033382095997));
#89125=CARTESIAN_POINT('Ctrl Pts',(-1.417445164947,1.90325048760995,0.503367137354524));
#89126=CARTESIAN_POINT('Ctrl Pts',(-1.47955450671666,1.85367648853688,0.508700892613051));
#89127=CARTESIAN_POINT('Ctrl Pts',(-1.54159448650848,1.8041578523211,0.514028691282705));
#89128=CARTESIAN_POINT('Ctrl Pts',(-1.60121196736101,1.75146840916292,0.519356489952359));
#89129=CARTESIAN_POINT('Ctrl Pts',(-1.6580706854012,1.69587725520251,0.524684288622014));
#89130=CARTESIAN_POINT('Ctrl Pts',(-1.71489474473583,1.6403199872934,0.530008839687576));
#89131=CARTESIAN_POINT('Ctrl Pts',(-1.76896304640341,1.58186484532476,0.535333390753139));
#89132=CARTESIAN_POINT('Ctrl Pts',(-1.81997385675543,1.52081991807931,0.540657941818702));
#89133=CARTESIAN_POINT('Ctrl Pts',(-1.8709693038848,1.4597933760899,0.54598088925823));
#89134=CARTESIAN_POINT('Ctrl Pts',(-1.9189087892869,1.39617895589138,0.551303836697758));
#89135=CARTESIAN_POINT('Ctrl Pts',(-1.96352978159866,1.33031908175261,0.556626784137286));
#89136=CARTESIAN_POINT('Ctrl Pts',(-2.00815109504782,1.26445873362016,0.56194976988608));
#89137=CARTESIAN_POINT('Ctrl Pts',(-2.04945360726806,1.19635328678691,0.567272755634874));
#89138=CARTESIAN_POINT('Ctrl Pts',(-2.08721801761038,1.12637427592368,0.572595741383668));
#89139=CARTESIAN_POINT('Ctrl Pts',(-2.12502084240226,1.0563240815001,0.577924141742823));
#89140=CARTESIAN_POINT('Ctrl Pts',(-2.15927815392128,0.984396927969013,
0.583252542101979));
#89141=CARTESIAN_POINT('Ctrl Pts',(-2.18981685108996,0.910988595528203,
0.588580942461134));
#89142=CARTESIAN_POINT('Ctrl Pts',(-2.22037059747506,0.837544088070657,
0.593911968611746));
#89143=CARTESIAN_POINT('Ctrl Pts',(-2.24720192115811,0.762617387700967,
0.599242994762358));
#89144=CARTESIAN_POINT('Ctrl Pts',(-2.27018699839248,0.686621478567161,
0.60457402091297));
#89145=CARTESIAN_POINT('Ctrl Pts',(-2.293213949893,0.610487119912694,0.609914759139188));
#89146=CARTESIAN_POINT('Ctrl Pts',(-2.31238054031918,0.533280114454326,
0.615255497365405));
#89147=CARTESIAN_POINT('Ctrl Pts',(-2.32761371816615,0.455425560882073,
0.620596235591622));
#89148=CARTESIAN_POINT('Ctrl Pts',(-2.34184793131004,0.38267657042831,0.625586737706242));
#89149=CARTESIAN_POINT('Ctrl Pts',(-2.35264818505678,0.309362574879414,
0.630577239820862));
#89150=CARTESIAN_POINT('Ctrl Pts',(-2.35999596812134,0.235832764795321,
0.635567741935482));
#89151=CARTESIAN_POINT('Ctrl Pts',(-2.36208369198396,0.214940757263645,
0.636985692119852));
#89152=CARTESIAN_POINT('Ctrl Pts',(-2.36389406907271,0.194020289892537,
0.638403642304223));
#89153=CARTESIAN_POINT('Ctrl Pts',(-2.36542649454111,0.173076750093528,
0.639821592488593));
#89154=CARTESIAN_POINT('Origin',(0.,0.,-1.84858989190503));
#89155=CARTESIAN_POINT('',(-2.36542648301433,0.173076907629062,1.83854786047046));
#89156=CARTESIAN_POINT('',(-2.36542650134106,0.173076657159213,1.63877486397391));
#89157=CARTESIAN_POINT('',(-2.36542649454111,0.173076750093529,-1.84858989190503));
#89158=CARTESIAN_POINT('Ctrl Pts',(-2.36542648301433,0.173076907629062,
1.83854786047046));
#89159=CARTESIAN_POINT('Ctrl Pts',(-2.36078946920551,0.236450557041656,
1.8345366875538));
#89160=CARTESIAN_POINT('Ctrl Pts',(-2.35360599959298,0.29963333287273,1.83046499197252));
#89161=CARTESIAN_POINT('Ctrl Pts',(-2.34163874790418,0.377018108149751,
1.82535131063931));
#89162=CARTESIAN_POINT('Ctrl Pts',(-2.33925412049139,0.391541598455056,
1.82438608712068));
#89163=CARTESIAN_POINT('Ctrl Pts',(-2.33499820758016,0.416034006121167,
1.82274857644167));
#89164=CARTESIAN_POINT('Ctrl Pts',(-2.33319784448188,0.426014949010509,
1.82207852454145));
#89165=CARTESIAN_POINT('Ctrl Pts',(-2.32975839799822,0.444406675857587,
1.82083860890605));
#89166=CARTESIAN_POINT('Ctrl Pts',(-2.32813763609304,0.452820748977882,
1.82026933439943));
#89167=CARTESIAN_POINT('Ctrl Pts',(-2.32469467624383,0.470187401195334,
1.81909007778314));
#89168=CARTESIAN_POINT('Ctrl Pts',(-2.32286627614208,0.479138590730262,
1.81847990664027));
#89169=CARTESIAN_POINT('Ctrl Pts',(-2.31862843843171,0.499290994858359,
1.81710076874745));
#89170=CARTESIAN_POINT('Ctrl Pts',(-2.31618947377455,0.51048569676617,1.81633086850144));
#89171=CARTESIAN_POINT('Ctrl Pts',(-2.30973066525293,0.539131726326424,
1.81435084913924));
#89172=CARTESIAN_POINT('Ctrl Pts',(-2.30559416500161,0.556555729359762,
1.81313701525027));
#89173=CARTESIAN_POINT('Ctrl Pts',(-2.27703296145798,0.671076118074422,
1.80509474436746));
#89174=CARTESIAN_POINT('Ctrl Pts',(-2.24668163386356,0.766576103238891,
1.7980760022881));
#89175=CARTESIAN_POINT('Ctrl Pts',(-2.17711251585113,0.945412934733576,
1.78433365041024));
#89176=CARTESIAN_POINT('Ctrl Pts',(-2.13889589125223,1.02895429625545,1.77764627994544));
#89177=CARTESIAN_POINT('Ctrl Pts',(-2.05640439074153,1.18470813939627,1.76477140616635));
#89178=CARTESIAN_POINT('Ctrl Pts',(-2.01291108543624,1.2571883049359,1.7585962317565));
#89179=CARTESIAN_POINT('Ctrl Pts',(-1.93002190020279,1.37995125326647,1.74795549229346));
#89180=CARTESIAN_POINT('Ctrl Pts',(-1.89228839017556,1.431256898583,1.74344846149813));
#89181=CARTESIAN_POINT('Ctrl Pts',(-1.84546732484836,1.48982429587284,1.73828626527198));
#89182=CARTESIAN_POINT('Ctrl Pts',(-1.83833892869344,1.49861138251134,1.73751130188896));
#89183=CARTESIAN_POINT('Ctrl Pts',(-1.82728026725469,1.51204560728817,1.73632621798991));
#89184=CARTESIAN_POINT('Ctrl Pts',(-1.82339466620307,1.51672904205132,1.73591302280914));
#89185=CARTESIAN_POINT('Ctrl Pts',(-1.81621265750569,1.52531825037258,1.73515522855756));
#89186=CARTESIAN_POINT('Ctrl Pts',(-1.8129216648719,1.52922830873908,1.73481026226366));
#89187=CARTESIAN_POINT('Ctrl Pts',(-1.80547096310068,1.53802269854776,1.73403435786301));
#89188=CARTESIAN_POINT('Ctrl Pts',(-1.8013040663673,1.54290080134626,1.73360395471793));
#89189=CARTESIAN_POINT('Ctrl Pts',(-1.78896062672022,1.55723285602097,1.7323391399935));
#89190=CARTESIAN_POINT('Ctrl Pts',(-1.78072892657754,1.56663933272245,1.73150865772511));
#89191=CARTESIAN_POINT('Ctrl Pts',(-1.71086348463299,1.64521334697599,1.7245640790034));
#89192=CARTESIAN_POINT('Ctrl Pts',(-1.64529200704371,1.71078913814569,1.71871835763982));
#89193=CARTESIAN_POINT('Ctrl Pts',(-1.41156096440522,1.91862999146322,1.69931285419988));
#89194=CARTESIAN_POINT('Ctrl Pts',(-1.22753265730542,2.04127618589842,1.68619121536536));
#89195=CARTESIAN_POINT('Ctrl Pts',(-1.00671123389437,2.14763948570874,1.6704010962321));
#89196=CARTESIAN_POINT('Ctrl Pts',(-0.984021977492536,2.15812963990116,
1.66877980845074));
#89197=CARTESIAN_POINT('Ctrl Pts',(-0.942982730400442,2.17632200945155,
1.66584648732082));
#89198=CARTESIAN_POINT('Ctrl Pts',(-0.924693377660703,2.18415568037977,
1.66453895848046));
#89199=CARTESIAN_POINT('Ctrl Pts',(-0.896338233776443,2.19588074060702,
1.66251036777533));
#89200=CARTESIAN_POINT('Ctrl Pts',(-0.886340513137628,2.19993521371126,
1.66179483627105));
#89201=CARTESIAN_POINT('Ctrl Pts',(-0.876224236830244,2.203957612787,1.66107045510289));
#89202=CARTESIAN_POINT('Ctrl Pts',(-0.876132854440562,2.20399394135745,
1.66106391159001));
#89203=CARTESIAN_POINT('Ctrl Pts',(-0.875948293566478,2.20406729923371,
1.6610506958929));
#89204=CARTESIAN_POINT('Ctrl Pts',(-0.875855114987727,2.20410432831643,
1.66104402370074));
#89205=CARTESIAN_POINT('Ctrl Pts',(-0.875666914997403,2.20417910500324,
1.66103054729461));
#89206=CARTESIAN_POINT('Ctrl Pts',(-0.875571893499305,2.20421685236911,
1.6610237430732));
#89207=CARTESIAN_POINT('Ctrl Pts',(-0.875379959564238,2.20429308390839,
1.66100999915995));
#89208=CARTESIAN_POINT('Ctrl Pts',(-0.875283047018924,2.20433156783963,
1.66100305945903));
#89209=CARTESIAN_POINT('Ctrl Pts',(-0.875087281387327,2.20440929134447,
1.66098904103077));
#89210=CARTESIAN_POINT('Ctrl Pts',(-0.874988428197988,2.20444853066051,
1.66098196229468));
#89211=CARTESIAN_POINT('Ctrl Pts',(-0.874788730188428,2.20452778431258,
1.66096766213328));
#89212=CARTESIAN_POINT('Ctrl Pts',(-0.874687885262558,2.20456779837812,
1.66096044069897));
#89213=CARTESIAN_POINT('Ctrl Pts',(-0.874516479199353,2.20463579665004,
1.66094816636857));
#89214=CARTESIAN_POINT('Ctrl Pts',(-0.874445919459017,2.2046637843906,1.66094311359132));
#89215=CARTESIAN_POINT('Ctrl Pts',(-0.874298124993661,2.20472239931375,
1.66093253000387));
#89216=CARTESIAN_POINT('Ctrl Pts',(-0.874220890016408,2.20475302581993,
1.66092699917204));
#89217=CARTESIAN_POINT('Ctrl Pts',(-0.87405909559096,2.20481717341567,1.66091541295426));
#89218=CARTESIAN_POINT('Ctrl Pts',(-0.873974535816569,2.204850693702,1.66090935754066));
#89219=CARTESIAN_POINT('Ctrl Pts',(-0.873797376069789,2.20492090969152,
1.66089667089196));
#89220=CARTESIAN_POINT('Ctrl Pts',(-0.873704775706758,2.20495760442883,
1.6608900396237));
#89221=CARTESIAN_POINT('Ctrl Pts',(-0.873510745645776,2.20503447856122,
1.66087614473807));
#89222=CARTESIAN_POINT('Ctrl Pts',(-0.873409315489886,2.20507465679007,
1.66086888108166));
#89223=CARTESIAN_POINT('Ctrl Pts',(-0.873196755344978,2.20515883855136,
1.66085365906175));
#89224=CARTESIAN_POINT('Ctrl Pts',(-0.873085624804296,2.20520284068071,
1.6608457006512));
#89225=CARTESIAN_POINT('Ctrl Pts',(-0.872852703142428,2.20529504562849,
1.66082902029729));
#89226=CARTESIAN_POINT('Ctrl Pts',(-0.872730911358362,2.20534324675688,
1.66082029829735));
#89227=CARTESIAN_POINT('Ctrl Pts',(-0.872475606378897,2.20544426349637,
1.6608020147658));
#89228=CARTESIAN_POINT('Ctrl Pts',(-0.872342092385068,2.20549707707095,
1.66079245316602));
#89229=CARTESIAN_POINT('Ctrl Pts',(-0.872062171201412,2.20560777493306,
1.66077240648304));
#89230=CARTESIAN_POINT('Ctrl Pts',(-0.871915763045639,2.20566565676627,
1.66076192131738));
#89231=CARTESIAN_POINT('Ctrl Pts',(-0.871608758801001,2.20578699422658,
1.66073993473703));
#89232=CARTESIAN_POINT('Ctrl Pts',(-0.871448161551489,2.20585044689032,
1.66072843322314));
#89233=CARTESIAN_POINT('Ctrl Pts',(-0.871111346273246,2.20598348153119,
1.66070431127949));
#89234=CARTESIAN_POINT('Ctrl Pts',(-0.870935126838851,2.20605305993026,
1.66069169072928));
#89235=CARTESIAN_POINT('Ctrl Pts',(-0.870565498262388,2.20619895271629,
1.66066521828813));
#89236=CARTESIAN_POINT('Ctrl Pts',(-0.870372081269755,2.20627526521112,
1.66065136581131));
#89237=CARTESIAN_POINT('Ctrl Pts',(-0.861654597737763,2.2097134154118,1.66002701550167));
#89238=CARTESIAN_POINT('Ctrl Pts',(-0.853111241095542,2.21302580877359,
1.65941486439869));
#89239=CARTESIAN_POINT('Ctrl Pts',(-0.833602346320865,2.22045995697617,
1.6580162805502));
#89240=CARTESIAN_POINT('Ctrl Pts',(-0.82262510588512,2.2245501160716,1.65722880643304));
#89241=CARTESIAN_POINT('Ctrl Pts',(-0.793991863493191,2.2349780486938,1.65517316846091));
#89242=CARTESIAN_POINT('Ctrl Pts',(-0.776290462273415,2.24118786366923,
1.65390079528855));
#89243=CARTESIAN_POINT('Ctrl Pts',(-0.610447408566426,2.29716669274774,
1.6419630319133));
#89244=CARTESIAN_POINT('Ctrl Pts',(-0.457829257236879,2.3323798346759,1.63081220241945));
#89245=CARTESIAN_POINT('Ctrl Pts',(-0.190713177547464,2.36677375944278,
1.61120713032582));
#89246=CARTESIAN_POINT('Ctrl Pts',(-0.0776495612631143,2.37317526241946,
1.60289350109526));
#89247=CARTESIAN_POINT('Ctrl Pts',(0.104411712666428,2.37045446012087,1.58978273650796));
#89248=CARTESIAN_POINT('Ctrl Pts',(0.173312923810354,2.36641518660472,1.58488721040152));
#89249=CARTESIAN_POINT('Ctrl Pts',(0.253306797740341,2.35821206335886,1.57935022432202));
#89250=CARTESIAN_POINT('Ctrl Pts',(0.264658543276269,2.35696506937642,1.5785679660727));
#89251=CARTESIAN_POINT('Ctrl Pts',(0.282067453334594,2.35492533211052,1.57737410250882));
#89252=CARTESIAN_POINT('Ctrl Pts',(0.28813110208817,2.35419112185069,1.57695935292082));
#89253=CARTESIAN_POINT('Ctrl Pts',(0.299262419565145,2.35279964687085,1.57620004898276));
#89254=CARTESIAN_POINT('Ctrl Pts',(0.304330783839253,2.35214943171765,1.57585511726128));
#89255=CARTESIAN_POINT('Ctrl Pts',(0.315732224892021,2.3506492831538,1.57508095693518));
#89256=CARTESIAN_POINT('Ctrl Pts',(0.322063981448061,2.34979013626968,1.57465225185626));
#89257=CARTESIAN_POINT('Ctrl Pts',(0.338309633588639,2.34751888822697,1.57355526580704));
#89258=CARTESIAN_POINT('Ctrl Pts',(0.348218321895944,2.34606955307509,1.57288901637182));
#89259=CARTESIAN_POINT('Ctrl Pts',(0.408757211352561,2.3368225838086,1.56883414380662));
#89260=CARTESIAN_POINT('Ctrl Pts',(0.459137310044456,2.32744840920093,1.56552686046377));
#89261=CARTESIAN_POINT('Ctrl Pts',(0.539307523466072,2.30982620105871,1.56031487896943));
#89262=CARTESIAN_POINT('Ctrl Pts',(0.569305596630838,2.30261611072903,1.55837627227424));
#89263=CARTESIAN_POINT('Ctrl Pts',(0.806769121196318,2.24061673541437,1.54306315222918));
#89264=CARTESIAN_POINT('Ctrl Pts',(1.00606045543149,2.15849173842311,1.53031226461131));
#89265=CARTESIAN_POINT('Ctrl Pts',(1.23636181296534,2.02466989643282,1.51332260638178));
#89266=CARTESIAN_POINT('Ctrl Pts',(1.28026129344819,1.99720031575992,1.50997648385924));
#89267=CARTESIAN_POINT('Ctrl Pts',(1.33623241912281,1.95957308264996,1.50554833987802));
#89268=CARTESIAN_POINT('Ctrl Pts',(1.34915320767797,1.95069970693627,1.50451451250084));
#89269=CARTESIAN_POINT('Ctrl Pts',(1.37010328722942,1.93600448926739,1.50281867490047));
#89270=CARTESIAN_POINT('Ctrl Pts',(1.37818583151874,1.9302591040672,1.50215959124514));
#89271=CARTESIAN_POINT('Ctrl Pts',(1.39372866385759,1.91906326993115,1.50088266602632));
#89272=CARTESIAN_POINT('Ctrl Pts',(1.40119361331933,1.91361957459484,1.50026509325537));
#89273=CARTESIAN_POINT('Ctrl Pts',(1.41832747823791,1.90097096861113,1.49883757703691));
#89274=CARTESIAN_POINT('Ctrl Pts',(1.42797356639931,1.89373571105629,1.49802645876315));
#89275=CARTESIAN_POINT('Ctrl Pts',(1.45883677398842,1.87021620795255,1.49540683272591));
#89276=CARTESIAN_POINT('Ctrl Pts',(1.47983310342644,1.85364702176488,1.49358713373708));
#89277=CARTESIAN_POINT('Ctrl Pts',(1.65962779041565,1.70676081712812,1.47766829828814));
#89278=CARTESIAN_POINT('Ctrl Pts',(1.80112210429016,1.55670177420236,1.46270789923479));
#89279=CARTESIAN_POINT('Ctrl Pts',(1.99182340855291,1.2931479144705,1.43896385083393));
#89280=CARTESIAN_POINT('Ctrl Pts',(2.05468641772583,1.19074043538516,1.43025887009652));
#89281=CARTESIAN_POINT('Ctrl Pts',(2.11583771251502,1.07173646831121,1.42101465012874));
#89282=CARTESIAN_POINT('Ctrl Pts',(2.12203441110386,1.05941411364828,1.4200674690894));
#89283=CARTESIAN_POINT('Ctrl Pts',(2.13103254406417,1.04112524826161,1.41867716107195));
#89284=CARTESIAN_POINT('Ctrl Pts',(2.13391703052254,1.03520026852153,1.4182291317618));
#89285=CARTESIAN_POINT('Ctrl Pts',(2.13897989649594,1.02468962931504,1.41743866117201));
#89286=CARTESIAN_POINT('Ctrl Pts',(2.14116828377551,1.02010892378651,1.4170956091862));
#89287=CARTESIAN_POINT('Ctrl Pts',(2.14588324857263,1.01015759706576,1.41635350112827));
#89288=CARTESIAN_POINT('Ctrl Pts',(2.1484043787382,1.00478451162321,1.41595478125966));
#89289=CARTESIAN_POINT('Ctrl Pts',(2.15526194882771,0.990025700850975,1.41486481842168));
#89290=CARTESIAN_POINT('Ctrl Pts',(2.15955729328035,0.980620856009067,1.41417604623083));
#89291=CARTESIAN_POINT('Ctrl Pts',(2.18107486487989,0.932680056254436,1.41069289709984));
#89292=CARTESIAN_POINT('Ctrl Pts',(2.19732891832583,0.893714618238608,1.40795284046196));
#89293=CARTESIAN_POINT('Ctrl Pts',(2.29901066351523,0.63038123066438,1.3899025210155));
#89294=CARTESIAN_POINT('Ctrl Pts',(2.35099110175549,0.394584735383903,1.3758382498165));
#89295=CARTESIAN_POINT('Ctrl Pts',(2.37092947700188,0.0901015995568576,
1.35652774570403));
#89296=CARTESIAN_POINT('Ctrl Pts',(2.37250804637827,0.0250845980826749,
1.35234969097489));
#89297=CARTESIAN_POINT('Ctrl Pts',(2.37112964660744,-0.0568168608126222,
1.3469792015065));
#89298=CARTESIAN_POINT('Ctrl Pts',(2.37066434685687,-0.0737189700969752,
1.34586518855255));
#89299=CARTESIAN_POINT('Ctrl Pts',(2.36962920091126,-0.100793227308003,
1.34407097712792));
#89300=CARTESIAN_POINT('Ctrl Pts',(2.36917445765771,-0.110969401803757,
1.3433943926132));
#89301=CARTESIAN_POINT('Ctrl Pts',(2.36818631869682,-0.130290163147333,
1.34210547398921));
#89302=CARTESIAN_POINT('Ctrl Pts',(2.36766547034975,-0.139435229124785,
1.34149354507675));
#89303=CARTESIAN_POINT('Ctrl Pts',(2.36635893524258,-0.160250628796372,
1.34009639716961));
#89304=CARTESIAN_POINT('Ctrl Pts',(2.3655398701337,-0.171918552513906,1.33931014376602));
#89305=CARTESIAN_POINT('Ctrl Pts',(2.36318695089678,-0.202225782935935,
1.33725960078347));
#89306=CARTESIAN_POINT('Ctrl Pts',(2.36151889844341,-0.220853547448027,
1.33599113472671));
#89307=CARTESIAN_POINT('Ctrl Pts',(2.3434832057252,-0.398577263587962,1.32380854990065));
#89308=CARTESIAN_POINT('Ctrl Pts',(2.31128595077761,-0.555622095833425,
1.31238418157411));
#89309=CARTESIAN_POINT('Ctrl Pts',(2.22568147377741,-0.82922891150625,1.29150236552574));
#89310=CARTESIAN_POINT('Ctrl Pts',(2.1781704149492,-0.947023880515805,1.28217169300353));
#89311=CARTESIAN_POINT('Ctrl Pts',(2.09775985342188,-1.10788681887603,1.2693257546231));
#89312=CARTESIAN_POINT('Ctrl Pts',(2.07246563938949,-1.1545115019453,1.26559126242188));
#89313=CARTESIAN_POINT('Ctrl Pts',(2.04022070762839,-1.20946751382153,1.2612089611619));
#89314=CARTESIAN_POINT('Ctrl Pts',(2.0347517882203,-1.21864571310415,1.26047775507982));
#89315=CARTESIAN_POINT('Ctrl Pts',(2.02614118893451,-1.23287685423037,1.25934543186852));
#89316=CARTESIAN_POINT('Ctrl Pts',(2.0230422877164,-1.23795531393218,1.25894164405185));
#89317=CARTESIAN_POINT('Ctrl Pts',(2.01723926112892,-1.24738529425189,1.25819248220313));
#89318=CARTESIAN_POINT('Ctrl Pts',(2.01454016861473,-1.25173967691547,1.25784680447665));
#89319=CARTESIAN_POINT('Ctrl Pts',(2.00833414714447,-1.2616796386663,1.25705825432367));
#89320=CARTESIAN_POINT('Ctrl Pts',(2.00481801740971,-1.26725935662109,1.25661599498647));
#89321=CARTESIAN_POINT('Ctrl Pts',(1.99553869541549,-1.28184935684369,1.25546037829484));
#89322=CARTESIAN_POINT('Ctrl Pts',(1.9897376692077,-1.2908355731592,1.25474943525184));
#89323=CARTESIAN_POINT('Ctrl Pts',(1.94833654444581,-1.35402668219223,1.24975357531829));
#89324=CARTESIAN_POINT('Ctrl Pts',(1.91058357049398,-1.40679625713357,1.24559968142671));
#89325=CARTESIAN_POINT('Ctrl Pts',(1.76734723253114,-1.59058344953836,1.23094002278382));
#89326=CARTESIAN_POINT('Ctrl Pts',(1.65016865711554,-1.71184752180714,1.22086508850055));
#89327=CARTESIAN_POINT('Ctrl Pts',(1.4461511635487,-1.88239169538279,1.20435936797207));
#89328=CARTESIAN_POINT('Ctrl Pts',(1.36736387498747,-1.94037736599113,1.19819308032981));
#89329=CARTESIAN_POINT('Ctrl Pts',(1.26407760998354,-2.00697267912134,1.19020050705911));
#89330=CARTESIAN_POINT('Ctrl Pts',(1.24270933223078,-2.02027349011524,1.18855192986346));
#89331=CARTESIAN_POINT('Ctrl Pts',(1.2109357731743,-2.03935630449554,1.18610573772215));
#89332=CARTESIAN_POINT('Ctrl Pts',(1.20069168525949,-2.04540437362625,1.18531784267427));
#89333=CARTESIAN_POINT('Ctrl Pts',(1.18245774542269,-2.05598543787751,1.18391658698031));
#89334=CARTESIAN_POINT('Ctrl Pts',(1.17448618471124,-2.06054959617885,1.18330437004523));
#89335=CARTESIAN_POINT('Ctrl Pts',(1.15770870808564,-2.07002663946857,1.18201656193481));
#89336=CARTESIAN_POINT('Ctrl Pts',(1.14889759114437,-2.07492989291094,1.18134064005603));
#89337=CARTESIAN_POINT('Ctrl Pts',(1.12564259485237,-2.08767740949748,1.17955759492487));
#89338=CARTESIAN_POINT('Ctrl Pts',(1.11114818601917,-2.09542785664514,1.17844716024833));
#89339=CARTESIAN_POINT('Ctrl Pts',(1.049360698672,-2.12764551254143,1.17371647218485));
#89340=CARTESIAN_POINT('Ctrl Pts',(1.00133464037768,-2.15066535028755,1.17004613274108));
#89341=CARTESIAN_POINT('Ctrl Pts',(0.743327201315127,-2.26381761734797,
1.15034802259969));
#89342=CARTESIAN_POINT('Ctrl Pts',(0.521925415414737,-2.32485798124351,
1.13335238799741));
#89343=CARTESIAN_POINT('Ctrl Pts',(0.230791534347974,-2.36138916194391,
1.11226318756905));
#89344=CARTESIAN_POINT('Ctrl Pts',(0.165981409199571,-2.36682813887218,
1.10765836584278));
#89345=CARTESIAN_POINT('Ctrl Pts',(0.0897706055122537,-2.37007724721254,
1.10240729187704));
#89346=CARTESIAN_POINT('Ctrl Pts',(0.078514193344609,-2.37047684095977,
1.10163590066085));
#89347=CARTESIAN_POINT('Ctrl Pts',(0.0611824109264023,-2.37096851141382,
1.10045506284741));
#89348=CARTESIAN_POINT('Ctrl Pts',(0.0551090122691025,-2.37111745141414,
1.10004257632034));
#89349=CARTESIAN_POINT('Ctrl Pts',(0.0439220309175732,-2.37134878741136,
1.09928527165299));
#89350=CARTESIAN_POINT('Ctrl Pts',(0.0388087791932072,-2.37143798062947,
1.09894009233226));
#89351=CARTESIAN_POINT('Ctrl Pts',(0.0272613420224132,-2.37160204999804,
1.09816270906982));
#89352=CARTESIAN_POINT('Ctrl Pts',(0.0208271249187241,-2.37166728224456,
1.0977310472707));
#89353=CARTESIAN_POINT('Ctrl Pts',(0.00181701753952309,-2.37178264448879,
1.09645989411048));
#89354=CARTESIAN_POINT('Ctrl Pts',(-0.0107593420243934,-2.37175893970204,
1.09562438529971));
#89355=CARTESIAN_POINT('Ctrl Pts',(-0.121277569906074,-2.37067151636503,
1.08832521448204));
#89356=CARTESIAN_POINT('Ctrl Pts',(-0.219079821903782,-2.3636414361208,
1.08216168954137));
#89357=CARTESIAN_POINT('Ctrl Pts',(-0.483043320752052,-2.32813548884667,
1.06566907232984));
#89358=CARTESIAN_POINT('Ctrl Pts',(-0.647038750826236,-2.28798749469019,
1.05554603311277));
#89359=CARTESIAN_POINT('Ctrl Pts',(-0.876155866956401,-2.20526814717473,
1.04021323313317));
#89360=CARTESIAN_POINT('Ctrl Pts',(-0.945647848826268,-2.1763742870372,
1.03539900093213));
#89361=CARTESIAN_POINT('Ctrl Pts',(-1.02963222535785,-2.13667224048885,
1.02931351886025));
#89362=CARTESIAN_POINT('Ctrl Pts',(-1.0455343238144,-2.12893605642434,1.02814913830386));
#89363=CARTESIAN_POINT('Ctrl Pts',(-1.0706132522976,-2.11638670019131,1.02629277940939));
#89364=CARTESIAN_POINT('Ctrl Pts',(-1.07984782311123,-2.11168986213796,
1.0256048711188));
#89365=CARTESIAN_POINT('Ctrl Pts',(-1.09716813447094,-2.1027371767555,1.02430625645085));
#89366=CARTESIAN_POINT('Ctrl Pts',(-1.1052606555503,-2.09849480081972,1.02369603413449));
#89367=CARTESIAN_POINT('Ctrl Pts',(-1.12341901413624,-2.08884139642988,
1.02231884017649));
#89368=CARTESIAN_POINT('Ctrl Pts',(-1.13347060393941,-2.0834041957356,1.02155094916313));
#89369=CARTESIAN_POINT('Ctrl Pts',(-1.15907935536975,-2.0693114911521,1.01958012934961));
#89370=CARTESIAN_POINT('Ctrl Pts',(-1.17457883687511,-2.06055320853583,
1.01837354805827));
#89371=CARTESIAN_POINT('Ctrl Pts',(-1.27414616094219,-2.00280234377696,
1.01053150551717));
#89372=CARTESIAN_POINT('Ctrl Pts',(-1.35521890737835,-1.9488567920097,1.0037167884491));
#89373=CARTESIAN_POINT('Ctrl Pts',(-1.57855936091099,-1.77955863673795,
0.983669897191608));
#89374=CARTESIAN_POINT('Ctrl Pts',(-1.71108144236095,-1.65253458391559,
0.970092985407875));
#89375=CARTESIAN_POINT('Ctrl Pts',(-1.86630449524888,-1.46484758807362,
0.952624710264361));
#89376=CARTESIAN_POINT('Ctrl Pts',(-1.90312816625077,-1.41667765377752,
0.948340471879313));
#89377=CARTESIAN_POINT('Ctrl Pts',(-1.94445010363024,-1.3580995539869,0.94340711967876));
#89378=CARTESIAN_POINT('Ctrl Pts',(-1.95076783510353,-1.34900906952627,
0.94264913413746));
#89379=CARTESIAN_POINT('Ctrl Pts',(-1.96043036731073,-1.33489596632093,
0.941484449330477));
#89380=CARTESIAN_POINT('Ctrl Pts',(-1.96381993225245,-1.32990441074984,
0.941074835692234));
#89381=CARTESIAN_POINT('Ctrl Pts',(-1.97004587104733,-1.32066023512288,
0.9403205921403));
#89382=CARTESIAN_POINT('Ctrl Pts',(-1.97288753236756,-1.31641140084742,
0.939975617425657));
#89383=CARTESIAN_POINT('Ctrl Pts',(-1.97929720234882,-1.30676032981454,
0.939195822797598));
#89384=CARTESIAN_POINT('Ctrl Pts',(-1.98285683729383,-1.30135265786273,
0.938761564612629));
#89385=CARTESIAN_POINT('Ctrl Pts',(-1.992024799152,-1.28730006092161,0.937639809005604));
#89386=CARTESIAN_POINT('Ctrl Pts',(-1.99759908221054,-1.27863292762991,
0.936954507167876));
#89387=CARTESIAN_POINT('Ctrl Pts',(-2.0335349882673,-1.22194961132857,0.93251322097085));
#89388=CARTESIAN_POINT('Ctrl Pts',(-2.06222240129705,-1.1728876292401,0.928857675183559));
#89389=CARTESIAN_POINT('Ctrl Pts',(-2.09539630956863,-1.11116514935026,
0.924426345993814));
#89390=CARTESIAN_POINT('Ctrl Pts',(-2.10157234166695,-1.09943957850797,
0.923591766862014));
#89391=CARTESIAN_POINT('Ctrl Pts',(-2.15892055163134,-0.988311423760099,
0.915744570409303));
#89392=CARTESIAN_POINT('Ctrl Pts',(-2.20310484075919,-0.885454186833194,
0.908944597628195));
#89393=CARTESIAN_POINT('Ctrl Pts',(-2.29138478011646,-0.63190122933475,
0.892478253612548));
#89394=CARTESIAN_POINT('Ctrl Pts',(-2.32810564990069,-0.479225872352841,
0.882776773069896));
#89395=CARTESIAN_POINT('Ctrl Pts',(-2.35206623302021,-0.305504894988578,
0.871326184600345));
#89396=CARTESIAN_POINT('Ctrl Pts',(-2.3544052013262,-0.28692319567133,0.870096731533758));
#89397=CARTESIAN_POINT('Ctrl Pts',(-2.35784734632995,-0.256692082399001,
0.868088023005161));
#89398=CARTESIAN_POINT('Ctrl Pts',(-2.35908483082418,-0.245058536702408,
0.867313000083297));
#89399=CARTESIAN_POINT('Ctrl Pts',(-2.36113700084134,-0.224307620635848,
0.865926754975572));
#89400=CARTESIAN_POINT('Ctrl Pts',(-2.36198507628958,-0.21519372843047,
0.865316597329193));
#89401=CARTESIAN_POINT('Ctrl Pts',(-2.36366401397413,-0.195943669444697,
0.864024967808889));
#89402=CARTESIAN_POINT('Ctrl Pts',(-2.36448247638349,-0.185806635575639,
0.86334311835523));
#89403=CARTESIAN_POINT('Ctrl Pts',(-2.36648445926961,-0.158850969118815,
0.861525369690516));
#89404=CARTESIAN_POINT('Ctrl Pts',(-2.36755386077973,-0.142024705494687,
0.860385911937931));
#89405=CARTESIAN_POINT('Ctrl Pts',(-2.37185064482659,-0.0607339844925643,
0.854856836730944));
#89406=CARTESIAN_POINT('Ctrl Pts',(-2.37262471810026,0.00382708308958538,
0.850391297016508));
#89407=CARTESIAN_POINT('Ctrl Pts',(-2.36975766244938,0.103295683469262,
0.843391208767397));
#89408=CARTESIAN_POINT('Ctrl Pts',(-2.36797705995664,0.138218398695283,
0.840910877802362));
#89409=CARTESIAN_POINT('Ctrl Pts',(-2.36542648444351,0.173076888096584,
0.838413605944556));
#89410=CARTESIAN_POINT('',(-2.37174952154217,0.00150650738259589,0.651410108094974));
#89411=CARTESIAN_POINT('Ctrl Pts',(-2.36542649454111,0.173076750093528,
0.639821592488593));
#89412=CARTESIAN_POINT('Ctrl Pts',(-2.36960119137977,0.116021492795841,
0.643684431024054));
#89413=CARTESIAN_POINT('Ctrl Pts',(-2.37171313261937,0.0587949158190506,
0.647547269559515));
#89414=CARTESIAN_POINT('Ctrl Pts',(-2.37174952154217,0.00150650738259589,
0.651410108094975));
#89415=CARTESIAN_POINT('Ctrl Pts',(-2.37174945202138,0.00161224572303678,
0.653084671769645));
#89416=CARTESIAN_POINT('Ctrl Pts',(-2.37190019934435,-0.220149781945233,
0.667087663185996));
#89417=CARTESIAN_POINT('Ctrl Pts',(-2.34095033112989,-0.440855449603671,
0.680174251846229));
#89418=CARTESIAN_POINT('Ctrl Pts',(-2.26803542871565,-0.695000945652463,
0.696904420974021));
#89419=CARTESIAN_POINT('Ctrl Pts',(-2.25519376496381,-0.735602998464327,
0.699626122806353));
#89420=CARTESIAN_POINT('Ctrl Pts',(-2.23126906427678,-0.804717684726376,
0.704359803829371));
#89421=CARTESIAN_POINT('Ctrl Pts',(-2.22071433456381,-0.833402599367388,
0.706354868725316));
#89422=CARTESIAN_POINT('Ctrl Pts',(-2.20491777535979,-0.873900622561888,
0.709218881062143));
#89423=CARTESIAN_POINT('Ctrl Pts',(-2.20012887739718,-0.885888032356933,
0.710072601531635));
#89424=CARTESIAN_POINT('Ctrl Pts',(-2.19168555197582,-0.906532287564808,
0.711553480751627));
#89425=CARTESIAN_POINT('Ctrl Pts',(-2.18807705833341,-0.915207697490257,
0.712179067489534));
#89426=CARTESIAN_POINT('Ctrl Pts',(-2.1810549556744,-0.931811056687275,
0.713382739602757));
#89427=CARTESIAN_POINT('Ctrl Pts',(-2.17764942411063,-0.93974227704877,
0.713960540291353));
#89428=CARTESIAN_POINT('Ctrl Pts',(-2.16953133285275,-0.958367585308325,
0.715324167136951));
#89429=CARTESIAN_POINT('Ctrl Pts',(-2.164782911702,-0.969045700377584,0.716111218095771));
#89430=CARTESIAN_POINT('Ctrl Pts',(-2.14795354818637,-1.00615004130597,
0.718864773368497));
#89431=CARTESIAN_POINT('Ctrl Pts',(-2.13546647825305,-1.03238807584507,
0.720845254770805));
#89432=CARTESIAN_POINT('Ctrl Pts',(-2.04878050945216,-1.2062287334226,0.734197410158997));
#89433=CARTESIAN_POINT('Ctrl Pts',(-1.95982950152917,-1.34593395505048,
0.74609990990669));
#89434=CARTESIAN_POINT('Ctrl Pts',(-1.79132296328342,-1.55805861808975,
0.765890965173791));
#89435=CARTESIAN_POINT('Ctrl Pts',(-1.72006701784822,-1.63638501540437,
0.77364993904509));
#89436=CARTESIAN_POINT('Ctrl Pts',(-1.61682357753721,-1.73565028426971,
0.783902046849395));
#89437=CARTESIAN_POINT('Ctrl Pts',(-1.58921656430365,-1.76096321164395,
0.786557065683813));
#89438=CARTESIAN_POINT('Ctrl Pts',(-1.54897649959918,-1.79614191254435,
0.790292824397852));
#89439=CARTESIAN_POINT('Ctrl Pts',(-1.5368262808448,-1.80654891481901,0.791404002870828));
#89440=CARTESIAN_POINT('Ctrl Pts',(-1.51783483534004,-1.82248533867831,
0.793113786790275));
#89441=CARTESIAN_POINT('Ctrl Pts',(-1.51106684033085,-1.82810076502783,
0.793717874523316));
#89442=CARTESIAN_POINT('Ctrl Pts',(-1.49850413807854,-1.83840664264008,
0.794829312550551));
#89443=CARTESIAN_POINT('Ctrl Pts',(-1.49271827740694,-1.84310764299804,
0.795337375969917));
#89444=CARTESIAN_POINT('Ctrl Pts',(-1.48280103164723,-1.85108805379323,
0.796201584216745));
#89445=CARTESIAN_POINT('Ctrl Pts',(-1.4786807259983,-1.85438108143118,0.796558696021009));
#89446=CARTESIAN_POINT('Ctrl Pts',(-1.47075912240844,-1.86066898825736,
0.797241513427998));
#89447=CARTESIAN_POINT('Ctrl Pts',(-1.46695963052574,-1.86366599032622,
0.797567379194729));
#89448=CARTESIAN_POINT('Ctrl Pts',(-1.45700536702365,-1.87146851321087,
0.798416919920881));
#89449=CARTESIAN_POINT('Ctrl Pts',(-1.45083592425455,-1.87625535594329,
0.798939280585641));
#89450=CARTESIAN_POINT('Ctrl Pts',(-1.42945187967792,-1.89267859590599,
0.800735954687388));
#89451=CARTESIAN_POINT('Ctrl Pts',(-1.41411954130577,-1.90416147541205,
0.802000054202724));
#89452=CARTESIAN_POINT('Ctrl Pts',(-1.28904322366006,-1.99549102025476,
0.812134204340709));
#89453=CARTESIAN_POINT('Ctrl Pts',(-1.17275377297891,-2.06598059179946,
0.820469858355212));
#89454=CARTESIAN_POINT('Ctrl Pts',(-0.935135019537183,-2.1834474356548,
0.836719936389383));
#89455=CARTESIAN_POINT('Ctrl Pts',(-0.81472756750881,-2.23117374801227,
0.844611975351883));
#89456=CARTESIAN_POINT('Ctrl Pts',(-0.626287275787845,-2.28856798794186,
0.857060353877867));
#89457=CARTESIAN_POINT('Ctrl Pts',(-0.560730850375216,-2.30550618002345,
0.861405122693557));
#89458=CARTESIAN_POINT('Ctrl Pts',(-0.477612661246062,-2.32322704923897,
0.86697526467404));
#89459=CARTESIAN_POINT('Ctrl Pts',(-0.460642315188279,-2.32665132917977,
0.868115618744511));
#89460=CARTESIAN_POINT('Ctrl Pts',(-0.433432762114011,-2.33183232493086,
0.869949616303167));
#89461=CARTESIAN_POINT('Ctrl Pts',(-0.42321664310937,-2.33370812614228,
0.870639466603019));
#89462=CARTESIAN_POINT('Ctrl Pts',(-0.40381592610359,-2.33713874865389,
0.871952040370887));
#89463=CARTESIAN_POINT('Ctrl Pts',(-0.394633821963965,-2.33870668852129,
0.872574334551565));
#89464=CARTESIAN_POINT('Ctrl Pts',(-0.373738321697926,-2.34214825347425,
0.873993018764612));
#89465=CARTESIAN_POINT('Ctrl Pts',(-0.362019703088027,-2.34398816124571,
0.874790458893769));
#89466=CARTESIAN_POINT('Ctrl Pts',(-0.331587823052923,-2.34853253566632,
0.876866245566565));
#89467=CARTESIAN_POINT('Ctrl Pts',(-0.312855452614087,-2.35110122819033,
0.8781488246241));
#89468=CARTESIAN_POINT('Ctrl Pts',(-0.14081865159366,-2.37259955144097,
0.889974655290919));
#89469=CARTESIAN_POINT('Ctrl Pts',(0.01393223192626,-2.37673044150717,0.900989036229827));
#89470=CARTESIAN_POINT('Ctrl Pts',(0.278971995363583,-2.35791408269947,
0.92031441702774));
#89471=CARTESIAN_POINT('Ctrl Pts',(0.389293736889757,-2.34222868082347,
0.928487732465121));
#89472=CARTESIAN_POINT('Ctrl Pts',(0.566921254213198,-2.30407296062881,
0.941572026516472));
#89473=CARTESIAN_POINT('Ctrl Pts',(0.635050844897255,-2.28623368806033,
0.946569421408522));
#89474=CARTESIAN_POINT('Ctrl Pts',(0.713393317430371,-2.26194675144873,
0.952217861868752));
#89475=CARTESIAN_POINT('Ctrl Pts',(0.724468899589216,-2.25842377757426,
0.953014056132335));
#89476=CARTESIAN_POINT('Ctrl Pts',(0.741431981247928,-2.25289044805436,
0.954229401872169));
#89477=CARTESIAN_POINT('Ctrl Pts',(0.747338019425586,-2.25093816901379,
0.954651784849289));
#89478=CARTESIAN_POINT('Ctrl Pts',(0.758167016164119,-2.24731125486395,
0.955424751406431));
#89479=CARTESIAN_POINT('Ctrl Pts',(0.763092151157998,-2.24564366513496,
0.955775727035633));
#89480=CARTESIAN_POINT('Ctrl Pts',(0.77416779464427,-2.24185294388493,0.956563714468716));
#89481=CARTESIAN_POINT('Ctrl Pts',(0.780315064556629,-2.23972069661643,
0.95700018466537));
#89482=CARTESIAN_POINT('Ctrl Pts',(0.798386795140658,-2.233368886105,0.958280932031745));
#89483=CARTESIAN_POINT('Ctrl Pts',(0.810286598367615,-2.2290791152583,0.959121205456315));
#89484=CARTESIAN_POINT('Ctrl Pts',(0.909203606115786,-2.1925236199448,0.96608484339345));
#89485=CARTESIAN_POINT('Ctrl Pts',(0.994303796470286,-2.15526690220199,
0.971940235128547));
#89486=CARTESIAN_POINT('Ctrl Pts',(1.24714665948801,-2.02639802979163,0.989548746400151));
#89487=CARTESIAN_POINT('Ctrl Pts',(1.40618086426479,-1.91945816567038,1.00098286634381));
#89488=CARTESIAN_POINT('Ctrl Pts',(1.58051329611421,-1.76882192714282,1.01560935133936));
#89489=CARTESIAN_POINT('Ctrl Pts',(1.60970406700244,-1.74229900959039,1.018137045335));
#89490=CARTESIAN_POINT('Ctrl Pts',(1.65908363214104,-1.69513188391543,1.02256446757721));
#89491=CARTESIAN_POINT('Ctrl Pts',(1.67958218262384,-1.67482362527024,1.02445031393656));
#89492=CARTESIAN_POINT('Ctrl Pts',(1.70854439430026,-1.64506375809287,1.02718815613796));
#89493=CARTESIAN_POINT('Ctrl Pts',(1.71731123647221,-1.63590978420207,1.02802691111613));
#89494=CARTESIAN_POINT('Ctrl Pts',(1.73245994703098,-1.61983616266004,1.02949409910292));
#89495=CARTESIAN_POINT('Ctrl Pts',(1.73887483423045,-1.61294791249619,1.03012109510505));
#89496=CARTESIAN_POINT('Ctrl Pts',(1.75119421061471,-1.59956056399419,1.03133639233605));
#89497=CARTESIAN_POINT('Ctrl Pts',(1.75710395476042,-1.59306649257013,1.0319244556718));
#89498=CARTESIAN_POINT('Ctrl Pts',(1.77107018243296,-1.57754709383758,1.03332642563169));
#89499=CARTESIAN_POINT('Ctrl Pts',(1.779093872831,-1.56849271805066,1.03414168943855));
#89500=CARTESIAN_POINT('Ctrl Pts',(1.80749742536801,-1.53594222495514,1.03706338754893));
#89501=CARTESIAN_POINT('Ctrl Pts',(1.82748317151552,-1.51210798508983,1.03918590478852));
#89502=CARTESIAN_POINT('Ctrl Pts',(2.00726799425765,-1.28893171373883,1.05891737124993));
#89503=CARTESIAN_POINT('Ctrl Pts',(2.13432091598966,-1.06540269509682,1.07791407339119));
#89504=CARTESIAN_POINT('Ctrl Pts',(2.24652140572883,-0.763414152816783,
1.10108988173988));
#89505=CARTESIAN_POINT('Ctrl Pts',(2.26713165456713,-0.699839653650499,
1.10582608471784));
#89506=CARTESIAN_POINT('Ctrl Pts',(2.28809913041615,-0.624444929267538,
1.11121472490217));
#89507=CARTESIAN_POINT('Ctrl Pts',(2.29108641721762,-0.613393953721566,
1.11199889659272));
#89508=CARTESIAN_POINT('Ctrl Pts',(2.29555942119889,-0.596358130423177,
1.11319859336554));
#89509=CARTESIAN_POINT('Ctrl Pts',(2.29710195584187,-0.590388586143888,
1.11361725757825));
#89510=CARTESIAN_POINT('Ctrl Pts',(2.29989826776665,-0.579390093938672,
1.11438536481693));
#89511=CARTESIAN_POINT('Ctrl Pts',(2.30115883630344,-0.574363068285223,
1.11473518284833));
#89512=CARTESIAN_POINT('Ctrl Pts',(2.30396753918112,-0.563004549516923,
1.11552278262396));
#89513=CARTESIAN_POINT('Ctrl Pts',(2.30550605654453,-0.556670791572006,
1.11596000904311));
#89514=CARTESIAN_POINT('Ctrl Pts',(2.30940601757654,-0.54032192621445,1.11708374140538));
#89515=CARTESIAN_POINT('Ctrl Pts',(2.31172846324525,-0.530297520000732,
1.11776808399291));
#89516=CARTESIAN_POINT('Ctrl Pts',(2.32597930071005,-0.466913146234204,
1.12206752539788));
#89517=CARTESIAN_POINT('Ctrl Pts',(2.33612582332861,-0.413164409637929,
1.12558995646478));
#89518=CARTESIAN_POINT('Ctrl Pts',(2.37566296653211,-0.155049719209109,
1.14212772190332));
#89519=CARTESIAN_POINT('Ctrl Pts',(2.38014721162845,0.052225095872193,1.1543618853275));
#89520=CARTESIAN_POINT('Ctrl Pts',(2.34886528777714,0.338677239461878,1.17243915997578));
#89521=CARTESIAN_POINT('Ctrl Pts',(2.33580962194246,0.419358512665458,1.17765242157147));
#89522=CARTESIAN_POINT('Ctrl Pts',(2.31477686546005,0.517048826088778,1.18419451420769));
#89523=CARTESIAN_POINT('Ctrl Pts',(2.31072803220957,0.534852648535692,1.18539614662353));
#89524=CARTESIAN_POINT('Ctrl Pts',(2.30401136974957,0.562886663600749,1.18730383391873));
#89525=CARTESIAN_POINT('Ctrl Pts',(2.30147994542172,0.573149057969203,1.18800549655524));
#89526=CARTESIAN_POINT('Ctrl Pts',(2.29660534685727,0.592357545578668,1.18932520790242));
#89527=CARTESIAN_POINT('Ctrl Pts',(2.29427827567475,0.601307550761481,1.18994272527489));
#89528=CARTESIAN_POINT('Ctrl Pts',(2.28894762795982,0.621327925757816,1.19133002635045));
#89529=CARTESIAN_POINT('Ctrl Pts',(2.2859159797053,0.632390512696399,1.19210070835192));
#89530=CARTESIAN_POINT('Ctrl Pts',(2.27800522657661,0.660456792871386,1.19406663020587));
#89531=CARTESIAN_POINT('Ctrl Pts',(2.27301598474208,0.677428439775392,1.19526542502308));
#89532=CARTESIAN_POINT('Ctrl Pts',(2.24118225912961,0.781402685033221,1.20267280526242));
#89533=CARTESIAN_POINT('Ctrl Pts',(2.20953944962569,0.86684468595643,1.20903741614421));
#89534=CARTESIAN_POINT('Ctrl Pts',(2.08956404200462,1.14120970025995,1.23040210042115));
#89535=CARTESIAN_POINT('Ctrl Pts',(1.98126506448331,1.3203083178078,1.24594997852642));
#89536=CARTESIAN_POINT('Ctrl Pts',(1.83292444535077,1.50546297717635,1.26279472511943));
#89537=CARTESIAN_POINT('Ctrl Pts',(1.81447101068959,1.52765372860108,1.26482590178007));
#89538=CARTESIAN_POINT('Ctrl Pts',(1.78284419706529,1.56430394082163,1.26819413674651));
#89539=CARTESIAN_POINT('Ctrl Pts',(1.76988906733138,1.57894680160847,1.26954360469841));
#89540=CARTESIAN_POINT('Ctrl Pts',(1.75161927047042,1.59908924169789,1.27140317389021));
#89541=CARTESIAN_POINT('Ctrl Pts',(1.74645728007169,1.60472534864904,1.27192386700856));
#89542=CARTESIAN_POINT('Ctrl Pts',(1.73764415443683,1.61425504260885,1.27280473822091));
#89543=CARTESIAN_POINT('Ctrl Pts',(1.73400698250907,1.61816140631649,1.27316595449202));
#89544=CARTESIAN_POINT('Ctrl Pts',(1.72699344772756,1.6256432191736,1.27385799371603));
#89545=CARTESIAN_POINT('Ctrl Pts',(1.72361913166181,1.62922046839549,1.27418897268696));
#89546=CARTESIAN_POINT('Ctrl Pts',(1.71550618610293,1.63776791525224,1.2749801205559));
#89547=CARTESIAN_POINT('Ctrl Pts',(1.7107570146786,1.64272811459033,1.27543948715198));
#89548=CARTESIAN_POINT('Ctrl Pts',(1.69350193061568,1.66059393607221,1.27709528267932));
#89549=CARTESIAN_POINT('Ctrl Pts',(1.68087059228491,1.67337835221554,1.27828247997792));
#89550=CARTESIAN_POINT('Ctrl Pts',(1.55151292539915,1.8013608426658,1.29020707135639));
#89551=CARTESIAN_POINT('Ctrl Pts',(1.42326367688259,1.90431886829479,1.30015100712979));
#89552=CARTESIAN_POINT('Ctrl Pts',(1.15016341902545,2.08043646260925,1.3200744672154));
#89553=CARTESIAN_POINT('Ctrl Pts',(1.00642616440537,2.15364530483014,1.33000947438913));
#89554=CARTESIAN_POINT('Ctrl Pts',(0.835369327703635,2.21987940513822,1.34196775509124));
#89555=CARTESIAN_POINT('Ctrl Pts',(0.814227880787186,2.22772067092529,1.34344717641525));
#89556=CARTESIAN_POINT('Ctrl Pts',(0.782154198812306,2.23909910039529,1.34569528351832));
#89557=CARTESIAN_POINT('Ctrl Pts',(0.771302379492129,2.24286036204504,1.34645653451253));
#89558=CARTESIAN_POINT('Ctrl Pts',(0.7516516964297,2.24951184848982,1.34783634828496));
#89559=CARTESIAN_POINT('Ctrl Pts',(0.742862356425267,2.25242965361046,1.34845398598422));
#89560=CARTESIAN_POINT('Ctrl Pts',(0.723988858100967,2.25857262125769,1.34978137707116));
#89561=CARTESIAN_POINT('Ctrl Pts',(0.713899773765236,2.26178187694073,1.35049163825368));
#89562=CARTESIAN_POINT('Ctrl Pts',(0.686763633164498,2.27021400999783,1.35240401233554));
#89563=CARTESIAN_POINT('Ctrl Pts',(0.669678889897915,2.2753123067269,1.35361016286553));
#89564=CARTESIAN_POINT('Ctrl Pts',(0.587382568876115,2.2988633654662,1.35943155263109));
#89565=CARTESIAN_POINT('Ctrl Pts',(0.521463526818901,2.31470629694618,1.36413005784406));
#89566=CARTESIAN_POINT('Ctrl Pts',(0.267800401144007,2.36428609419862,1.38235710521474));
#89567=CARTESIAN_POINT('Ctrl Pts',(0.0769230484837968,2.37815697464309,
1.39644633071298));
#89568=CARTESIAN_POINT('Ctrl Pts',(-0.170214055682804,2.36631516694071,
1.41435916701414));
#89569=CARTESIAN_POINT('Ctrl Pts',(-0.226802027086609,2.36156347236873,
1.41843164725273));
#89570=CARTESIAN_POINT('Ctrl Pts',(-0.304292437948064,2.35224506487116,
1.42392533183133));
#89571=CARTESIAN_POINT('Ctrl Pts',(-0.325382024273615,2.34942063989615,
1.42541190361973));
#89572=CARTESIAN_POINT('Ctrl Pts',(-0.361760298662337,2.3440494110431,1.42795816395798));
#89573=CARTESIAN_POINT('Ctrl Pts',(-0.377067004165928,2.34163589429986,
1.42902400952776));
#89574=CARTESIAN_POINT('Ctrl Pts',(-0.399222753271042,2.33791955104351,
1.43055768759882));
#89575=CARTESIAN_POINT('Ctrl Pts',(-0.406091044918971,2.33673633520323,
1.43103185873806));
#89576=CARTESIAN_POINT('Ctrl Pts',(-0.418105702324698,2.33461197044672,
1.4318589811803));
#89577=CARTESIAN_POINT('Ctrl Pts',(-0.423254303472963,2.33368404623458,
1.43221266720454));
#89578=CARTESIAN_POINT('Ctrl Pts',(-0.434180675578784,2.33167745354801,
1.43296161530433));
#89579=CARTESIAN_POINT('Ctrl Pts',(-0.439957525235858,2.33059434143513,
1.43335662325605));
#89580=CARTESIAN_POINT('Ctrl Pts',(-0.455664815203087,2.32758886946662,
1.43442816983229));
#89581=CARTESIAN_POINT('Ctrl Pts',(-0.465587223293734,2.32562441416782,
1.4351023696552));
#89582=CARTESIAN_POINT('Ctrl Pts',(-0.512023495830056,2.31612177139858,
1.43824619974959));
#89583=CARTESIAN_POINT('Ctrl Pts',(-0.548371213900686,2.3077862799206,1.44067397929807));
#89584=CARTESIAN_POINT('Ctrl Pts',(-0.820004876912631,2.23871260792112,
1.4586716819596));
#89585=CARTESIAN_POINT('Ctrl Pts',(-1.04491825131775,2.14299262869263,1.47288826058656));
#89586=CARTESIAN_POINT('Ctrl Pts',(-1.30821181642694,1.97945826629906,1.49248231528067));
#89587=CARTESIAN_POINT('Ctrl Pts',(-1.36351544968512,1.94177689001353,1.49677766855442));
#89588=CARTESIAN_POINT('Ctrl Pts',(-1.43095670604976,1.89152252922257,1.50229038128703));
#89589=CARTESIAN_POINT('Ctrl Pts',(-1.44465154991784,1.88108384886257,1.50342465932356));
#89590=CARTESIAN_POINT('Ctrl Pts',(-1.46639317180412,1.86413417801869,1.50525003912168));
#89591=CARTESIAN_POINT('Ctrl Pts',(-1.47451327519083,1.85771789124956,1.5059373877947));
#89592=CARTESIAN_POINT('Ctrl Pts',(-1.4898439540602,1.84544016425115,1.50724592915649));
#89593=CARTESIAN_POINT('Ctrl Pts',(-1.49706260214114,1.83958907593791,1.50786669876694));
#89594=CARTESIAN_POINT('Ctrl Pts',(-1.51340658001697,1.82618152318832,1.50928289069435));
#89595=CARTESIAN_POINT('Ctrl Pts',(-1.52250998605765,1.81859884679442,1.51007936756823));
#89596=CARTESIAN_POINT('Ctrl Pts',(-1.54599657544538,1.79873575837169,1.51215453977213));
#89597=CARTESIAN_POINT('Ctrl Pts',(-1.56029012488012,1.7863511496179,1.51343749040584));
#89598=CARTESIAN_POINT('Ctrl Pts',(-1.69096482546408,1.67036345598563,1.52535607241086));
#89599=CARTESIAN_POINT('Ctrl Pts',(-1.79699694451576,1.55571872582698,1.5364732521844));
#89600=CARTESIAN_POINT('Ctrl Pts',(-1.95912979380173,1.34154624215709,1.55602500011903));
#89601=CARTESIAN_POINT('Ctrl Pts',(-2.02074112783512,1.24681268843549,1.56432013105911));
#89602=CARTESIAN_POINT('Ctrl Pts',(-2.10880660932832,1.08761354906334,1.57742079317095));
#89603=CARTESIAN_POINT('Ctrl Pts',(-2.13958722590301,1.02573734574186,1.5823232036035));
#89604=CARTESIAN_POINT('Ctrl Pts',(-2.17230802171485,0.952055160998176,
1.58787530815811));
#89605=CARTESIAN_POINT('Ctrl Pts',(-2.17691365760954,0.941476559308161,
1.58866571460658));
#89606=CARTESIAN_POINT('Ctrl Pts',(-2.18386957156493,0.925175665865188,
1.58987293352133));
#89607=CARTESIAN_POINT('Ctrl Pts',(-2.1862748838328,0.919477271531227,1.59029294423025));
#89608=CARTESIAN_POINT('Ctrl Pts',(-2.19065525371491,0.908985422420414,
1.59106250204987));
#89609=CARTESIAN_POINT('Ctrl Pts',(-2.19263688087375,0.904194917318299,
1.59141243187071));
#89610=CARTESIAN_POINT('Ctrl Pts',(-2.19706796319036,0.893382720664257,
1.59219899774017));
#89611=CARTESIAN_POINT('Ctrl Pts',(-2.19950837527459,0.887357442133621,
1.59263508730703));
#89612=CARTESIAN_POINT('Ctrl Pts',(-2.20662459883719,0.869578036253152,
1.59391553795137));
#89613=CARTESIAN_POINT('Ctrl Pts',(-2.21123127437524,0.857796217109768,
1.59475588428019));
#89614=CARTESIAN_POINT('Ctrl Pts',(-2.24963888490191,0.757200884133428,
1.60186625241047));
#89615=CARTESIAN_POINT('Ctrl Pts',(-2.27817269073683,0.666454957687184,
1.60785450222644));
#89616=CARTESIAN_POINT('Ctrl Pts',(-2.33405985860222,0.442491303857375,
1.62216303430729));
#89617=CARTESIAN_POINT('Ctrl Pts',(-2.35553379466809,0.308279583528868,
1.63036049649394));
#89618=CARTESIAN_POINT('Ctrl Pts',(-2.36542650134105,0.173076657159373,
1.6387748639739));
#89619=CARTESIAN_POINT('Origin',(0.,0.,-1.84858989190503));
#89620=CARTESIAN_POINT('',(-2.36542649402054,0.173076757208175,2.83502806412758));
#89621=CARTESIAN_POINT('',(-2.36542650247982,0.173076641595803,2.63790316127816));
#89622=CARTESIAN_POINT('',(-2.36542649454111,0.173076750093529,-1.84858989190503));
#89623=CARTESIAN_POINT('',(-2.37174916735844,-0.00198736875130605,1.84947704601095));
#89624=CARTESIAN_POINT('Ctrl Pts',(-2.36542649402054,0.173076757208175,
2.83502806412758));
#89625=CARTESIAN_POINT('Ctrl Pts',(-2.35062081331563,0.375424836559319,
2.82209801839282));
#89626=CARTESIAN_POINT('Ctrl Pts',(-2.30990985923019,0.57508075576675,2.81006493442228));
#89627=CARTESIAN_POINT('Ctrl Pts',(-2.21435099249438,0.854630846330757,
2.7916303956933));
#89628=CARTESIAN_POINT('Ctrl Pts',(-2.17936365792477,0.940273970300902,
2.78575936514911));
#89629=CARTESIAN_POINT('Ctrl Pts',(-2.13187396907725,1.03952936624924,2.77856555361437));
#89630=CARTESIAN_POINT('Ctrl Pts',(-2.12410018256202,1.05532284642277,2.77740884225984));
#89631=CARTESIAN_POINT('Ctrl Pts',(-2.11101960895563,1.08116761947343,2.77549531335063));
#89632=CARTESIAN_POINT('Ctrl Pts',(-2.10581499890869,1.09127008276156,2.77474207227732));
#89633=CARTESIAN_POINT('Ctrl Pts',(-2.09629936250158,1.10941893269071,2.77337917708499));
#89634=CARTESIAN_POINT('Ctrl Pts',(-2.09201407875898,1.11747862426932,2.77277044258954));
#89635=CARTESIAN_POINT('Ctrl Pts',(-2.08274928435277,1.13466362669319,2.77146490022835));
#89636=CARTESIAN_POINT('Ctrl Pts',(-2.07775610554488,1.143781310873,2.77076761449222));
#89637=CARTESIAN_POINT('Ctrl Pts',(-2.06402338411574,1.16847096434277,2.76886668025715));
#89638=CARTESIAN_POINT('Ctrl Pts',(-2.0551678075032,1.18397727055729,2.76765888766045));
#89639=CARTESIAN_POINT('Ctrl Pts',(-2.00676312582322,1.26655537258809,2.76115041054048));
#89640=CARTESIAN_POINT('Ctrl Pts',(-1.96410850220163,1.33174176550113,2.75573742120935));
#89641=CARTESIAN_POINT('Ctrl Pts',(-1.81115241140593,1.54212307468216,2.73730964331619));
#89642=CARTESIAN_POINT('Ctrl Pts',(-1.68734476134249,1.67668428328827,2.72384076927719));
#89643=CARTESIAN_POINT('Ctrl Pts',(-1.48747566683035,1.849134708769,2.70473155581573));
#89644=CARTESIAN_POINT('Ctrl Pts',(-1.4228433826762,1.89931641364159,2.69889204304126));
#89645=CARTESIAN_POINT('Ctrl Pts',(-1.34563152556959,1.95310666895128,2.69240238160787));
#89646=CARTESIAN_POINT('Ctrl Pts',(-1.3354671407645,1.96007076283614,2.6915573427475));
#89647=CARTESIAN_POINT('Ctrl Pts',(-1.31995994152628,1.970518836045,2.69028268012245));
#89648=CARTESIAN_POINT('Ctrl Pts',(-1.31465677815963,1.97406086241314,2.68984932718709));
#89649=CARTESIAN_POINT('Ctrl Pts',(-1.30507933980531,1.98040200006651,2.68907138424483));
#89650=CARTESIAN_POINT('Ctrl Pts',(-1.30081027544932,1.98320871162198,2.68872629486574));
#89651=CARTESIAN_POINT('Ctrl Pts',(-1.29140929748524,1.98934600201504,2.68797003593557));
#89652=CARTESIAN_POINT('Ctrl Pts',(-1.28627356241031,1.99267052323071,2.68755926929789));
#89653=CARTESIAN_POINT('Ctrl Pts',(-1.27147493704341,2.00216908228728,2.68638228085509));
#89654=CARTESIAN_POINT('Ctrl Pts',(-1.26177989149606,2.00829307329571,2.68561928890724));
#89655=CARTESIAN_POINT('Ctrl Pts',(-1.19237782366946,2.05143073482997,2.6802119084379));
#89656=CARTESIAN_POINT('Ctrl Pts',(-1.1310901639791,2.085849983014,2.67572216380749));
#89657=CARTESIAN_POINT('Ctrl Pts',(-0.968736177501661,2.16776364535339,
2.66431135084394));
#89658=CARTESIAN_POINT('Ctrl Pts',(-0.865686114569203,2.21093626346685,
2.65752338993734));
#89659=CARTESIAN_POINT('Ctrl Pts',(-0.611756271118086,2.29683145976531,
2.64107986378301));
#89660=CARTESIAN_POINT('Ctrl Pts',(-0.458962915100539,2.33217142389709,
2.63138910592421));
#89661=CARTESIAN_POINT('Ctrl Pts',(-0.285229359811498,2.35461110655365,
2.61995046272885));
#89662=CARTESIAN_POINT('Ctrl Pts',(-0.266616384671434,2.35679123408781,
2.61872019165903));
#89663=CARTESIAN_POINT('Ctrl Pts',(-0.236335264165208,2.35997474627779,
2.61671000396813));
#89664=CARTESIAN_POINT('Ctrl Pts',(-0.224681844158692,2.36111270817905,
2.61593431964769));
#89665=CARTESIAN_POINT('Ctrl Pts',(-0.203895270850146,2.36298724727675,
2.61454679027975));
#89666=CARTESIAN_POINT('Ctrl Pts',(-0.194765311181239,2.36375728063889,
2.61393600986113));
#89667=CARTESIAN_POINT('Ctrl Pts',(-0.175480590673122,2.36527129422841,
2.61264294912869));
#89668=CARTESIAN_POINT('Ctrl Pts',(-0.16532506705863,2.36600282112872,2.61196029022927));
#89669=CARTESIAN_POINT('Ctrl Pts',(-0.13831748613817,2.36777351195848,2.6101400969242));
#89670=CARTESIAN_POINT('Ctrl Pts',(-0.121458766433615,2.36869813889126,
2.60899899669715));
#89671=CARTESIAN_POINT('Ctrl Pts',(-0.03995370405994,2.37229593697193,2.60345751955741));
#89672=CARTESIAN_POINT('Ctrl Pts',(0.0247682367854278,2.37250277940886,
2.59898092228217));
#89673=CARTESIAN_POINT('Ctrl Pts',(0.215265930670928,2.36531609832025,2.58556982924745));
#89674=CARTESIAN_POINT('Ctrl Pts',(0.340526931628984,2.3505518795912,2.57643685893082));
#89675=CARTESIAN_POINT('Ctrl Pts',(0.604265445461789,2.29793735776597,2.55679686752159));
#89676=CARTESIAN_POINT('Ctrl Pts',(0.741716841050238,2.25732514175687,2.54630939780244));
#89677=CARTESIAN_POINT('Ctrl Pts',(0.892238477155408,2.19760445527891,2.53504622392181));
#89678=CARTESIAN_POINT('Ctrl Pts',(0.909712530380675,2.19042872758904,2.53374253691056));
#89679=CARTESIAN_POINT('Ctrl Pts',(0.934185709619427,2.18003541035256,2.53192395898065));
#89680=CARTESIAN_POINT('Ctrl Pts',(0.941257182833415,2.17699155956425,2.53139935011336));
#89681=CARTESIAN_POINT('Ctrl Pts',(0.953120984368067,2.17181628084528,2.53052082432183));
#89682=CARTESIAN_POINT('Ctrl Pts',(0.957921244220867,2.16970331158631,2.5301658060735));
#89683=CARTESIAN_POINT('Ctrl Pts',(0.967697065993907,2.16536144182146,2.52944377180796));
#89684=CARTESIAN_POINT('Ctrl Pts',(0.97267201264778,2.1631312818722,2.52907683547195));
#89685=CARTESIAN_POINT('Ctrl Pts',(0.985318148235508,2.15740984599261,2.52814528409324));
#89686=CARTESIAN_POINT('Ctrl Pts',(0.992978580523133,2.15389476086213,2.52758211071458));
#89687=CARTESIAN_POINT('Ctrl Pts',(1.02394872638793,2.13948337850417,2.52530915710261));
#89688=CARTESIAN_POINT('Ctrl Pts',(1.04710019543511,2.12824844347747,2.52361898167136));
#89689=CARTESIAN_POINT('Ctrl Pts',(1.24937448612338,2.02598878461525,2.50889115926759));
#89690=CARTESIAN_POINT('Ctrl Pts',(1.41646280776033,1.91290981479908,2.49694374947774));
#89691=CARTESIAN_POINT('Ctrl Pts',(1.65580116804072,1.70218177847199,2.47722798843879));
#89692=CARTESIAN_POINT('Ctrl Pts',(1.73835111036047,1.61778554900491,2.46981392460874));
#89693=CARTESIAN_POINT('Ctrl Pts',(1.8261812897705,1.51347331686101,2.46090714208561));
#89694=CARTESIAN_POINT('Ctrl Pts',(1.83791826507087,1.49919845352564,2.45969366402645));
#89695=CARTESIAN_POINT('Ctrl Pts',(1.85676816633963,1.4757185752457,2.45770551259056));
#89696=CARTESIAN_POINT('Ctrl Pts',(1.8639824473826,1.46659563770402,2.45693491744183));
#89697=CARTESIAN_POINT('Ctrl Pts',(1.87675406868395,1.4501986131215,2.45555304184385));
#89698=CARTESIAN_POINT('Ctrl Pts',(1.88233698611168,1.44294466924186,2.45494279309596));
#89699=CARTESIAN_POINT('Ctrl Pts',(1.89406793249607,1.42751858466975,2.45364723152288));
#89700=CARTESIAN_POINT('Ctrl Pts',(1.90020536178318,1.41933865579932,2.45296151895348));
#89701=CARTESIAN_POINT('Ctrl Pts',(1.91645555549108,1.39738617219141,2.45112450922611));
#89702=CARTESIAN_POINT('Ctrl Pts',(1.926472554029,1.38354381291824,2.44996952880264));
#89703=CARTESIAN_POINT('Ctrl Pts',(1.97514433440288,1.31473144210644,2.44424328049535));
#89704=CARTESIAN_POINT('Ctrl Pts',(2.01159681321878,1.25824901956538,2.43958948434016));
#89705=CARTESIAN_POINT('Ctrl Pts',(2.1284803081641,1.0590514697767,2.42331889086194));
#89706=CARTESIAN_POINT('Ctrl Pts',(2.19649950927833,0.909612717007057,2.41131412795717));
#89707=CARTESIAN_POINT('Ctrl Pts',(2.284130618943,0.648413228828248,2.391228778403));
#89708=CARTESIAN_POINT('Ctrl Pts',(2.31215262685408,0.5400452827606,2.3831486763035));
#89709=CARTESIAN_POINT('Ctrl Pts',(2.33472179274567,0.417650904454418,2.37456136314503));
#89710=CARTESIAN_POINT('Ctrl Pts',(2.3369165204411,0.405190475947076,2.37369331304474));
#89711=CARTESIAN_POINT('Ctrl Pts',(2.34007915481195,0.386353709549208,2.372390983812));
#89712=CARTESIAN_POINT('Ctrl Pts',(2.34112089563768,0.379990255382738,2.37195273511217));
#89713=CARTESIAN_POINT('Ctrl Pts',(2.34294207326737,0.368573794852299,2.37116963887605));
#89714=CARTESIAN_POINT('Ctrl Pts',(2.34373113217126,0.363522465128319,2.37082426045647));
#89715=CARTESIAN_POINT('Ctrl Pts',(2.34541965613234,0.352478952600832,2.37007160591892));
#89716=CARTESIAN_POINT('Ctrl Pts',(2.34631249411381,0.346485869046732,2.36966470594815));
#89717=CARTESIAN_POINT('Ctrl Pts',(2.34878900711256,0.329413887988917,2.36850984522781));
#89718=CARTESIAN_POINT('Ctrl Pts',(2.35031727441194,0.318326925452593,2.36776492818652));
#89719=CARTESIAN_POINT('Ctrl Pts',(2.35997274440637,0.244416601982731,2.3628302789541));
#89720=CARTESIAN_POINT('Ctrl Pts',(2.36565953936341,0.181293752952874,2.35876597869869));
#89721=CARTESIAN_POINT('Ctrl Pts',(2.37918314435107,-0.0901588441511683,
2.34164038455785));
#89722=CARTESIAN_POINT('Ctrl Pts',(2.36206988193449,-0.298793572045404,
2.32928465013728));
#89723=CARTESIAN_POINT('Ctrl Pts',(2.30271240836311,-0.572585419331684,
2.31163056069565));
#89724=CARTESIAN_POINT('Ctrl Pts',(2.28435356803838,-0.641923431926614,
2.30703919982841));
#89725=CARTESIAN_POINT('Ctrl Pts',(2.25750139053517,-0.727467235907128,
2.30116901131475));
#89726=CARTESIAN_POINT('Ctrl Pts',(2.25192386609037,-0.744553543674305,
2.29998612991807));
#89727=CARTESIAN_POINT('Ctrl Pts',(2.24277310909129,-0.77154236815718,2.29810042182438));
#89728=CARTESIAN_POINT('Ctrl Pts',(2.2393271379669,-0.781487560874939,2.29740180172756));
#89729=CARTESIAN_POINT('Ctrl Pts',(2.2330776115169,-0.799143134136172,2.29615471620873));
#89730=CARTESIAN_POINT('Ctrl Pts',(2.2303000134326,-0.806862575076773,2.29560712167823));
#89731=CARTESIAN_POINT('Ctrl Pts',(2.22377733787605,-0.824699215634724,
2.29433633777904));
#89732=CARTESIAN_POINT('Ctrl Pts',(2.22000319464273,-0.834805518552139,
2.29361218701013));
#89733=CARTESIAN_POINT('Ctrl Pts',(2.20915229016338,-0.863267767433512,
2.29156091095236));
#89734=CARTESIAN_POINT('Ctrl Pts',(2.20191604539839,-0.881561550692104,
2.29022846541761));
#89735=CARTESIAN_POINT('Ctrl Pts',(2.15071883403685,-1.00642767758,2.28103487349744));
#89736=CARTESIAN_POINT('Ctrl Pts',(2.09927293223996,-1.10974495264606,2.27291904803231));
#89737=CARTESIAN_POINT('Ctrl Pts',(1.97749088074027,-1.31530350736038,2.25571784087368));
#89738=CARTESIAN_POINT('Ctrl Pts',(1.90622855021484,-1.41660987756806,2.24662961200988));
#89739=CARTESIAN_POINT('Ctrl Pts',(1.76418956046454,-1.58829007632479,2.23042270751757));
#89740=CARTESIAN_POINT('Ctrl Pts',(1.69624396525468,-1.66065994285745,2.22329002653166));
#89741=CARTESIAN_POINT('Ctrl Pts',(1.61478580231013,-1.73718832831345,2.21557902892978));
#89742=CARTESIAN_POINT('Ctrl Pts',(1.60554405013478,-1.74573331181411,2.21471553119767));
#89743=CARTESIAN_POINT('Ctrl Pts',(1.59147566477693,-1.75853480720565,2.21341867076947));
#89744=CARTESIAN_POINT('Ctrl Pts',(1.58669919720094,-1.76284574476228,2.21298138657661));
#89745=CARTESIAN_POINT('Ctrl Pts',(1.57809650949775,-1.77054669506712,2.21219931310642));
#89746=CARTESIAN_POINT('Ctrl Pts',(1.57427683625649,-1.77394380889891,2.21185399913475));
#89747=CARTESIAN_POINT('Ctrl Pts',(1.56589717107805,-1.78134807393061,2.21110066730268));
#89748=CARTESIAN_POINT('Ctrl Pts',(1.56133277452735,-1.78535007216217,2.21069303072267));
#89749=CARTESIAN_POINT('Ctrl Pts',(1.54827034845832,-1.79671461595299,2.20953396468365));
#89750=CARTESIAN_POINT('Ctrl Pts',(1.53973511612032,-1.80403444196131,2.20878561392358));
#89751=CARTESIAN_POINT('Ctrl Pts',(1.481832939209,-1.85298112029766,2.20376665137196));
#89752=CARTESIAN_POINT('Ctrl Pts',(1.43083071762854,-1.89264182771465,2.19962644643547));
#89753=CARTESIAN_POINT('Ctrl Pts',(1.1969838308649,-2.05962342461504,2.18153456650361));
#89754=CARTESIAN_POINT('Ctrl Pts',(0.998367222239815,-2.16289007118117,
2.168372080254));
#89755=CARTESIAN_POINT('Ctrl Pts',(0.733203815247222,-2.25632804369121,
2.150522682491));
#89756=CARTESIAN_POINT('Ctrl Pts',(0.677467091254764,-2.27368456931606,
2.14676435216336));
#89757=CARTESIAN_POINT('Ctrl Pts',(0.604762121050798,-2.29341430949082,
2.1418255507741));
#89758=CARTESIAN_POINT('Ctrl Pts',(0.588326865706808,-2.29768533357595,
2.14070681513311));
#89759=CARTESIAN_POINT('Ctrl Pts',(0.561945301404778,-2.30423949417779,
2.13890674021568));
#89760=CARTESIAN_POINT('Ctrl Pts',(0.552027451498906,-2.30663561394877,
2.13822905617417));
#89761=CARTESIAN_POINT('Ctrl Pts',(0.533178927643971,-2.31106083086407,
2.13693917022092));
#89762=CARTESIAN_POINT('Ctrl Pts',(0.524251336081692,-2.31310234650119,
2.13632738093875));
#89763=CARTESIAN_POINT('Ctrl Pts',(0.503920125714679,-2.3176278346579,2.1349321189594));
#89764=CARTESIAN_POINT('Ctrl Pts',(0.492509619106658,-2.32007942529672,
2.13414762321001));
#89765=CARTESIAN_POINT('Ctrl Pts',(0.457583893943007,-2.32731409124368,
2.13174177912825));
#89766=CARTESIAN_POINT('Ctrl Pts',(0.434014400223242,-2.33182446288757,
2.13011179381475));
#89767=CARTESIAN_POINT('Ctrl Pts',(0.247163100869148,-2.36465025509908,
2.11713495678288));
#89768=CARTESIAN_POINT('Ctrl Pts',(0.081421367215168,-2.37613357769856,
2.10524532297555));
#89769=CARTESIAN_POINT('Ctrl Pts',(-0.24078672014201,-2.36469696014912,
2.08172600016612));
#89770=CARTESIAN_POINT('Ctrl Pts',(-0.396517831685705,-2.34361942114607,
2.07018478833533));
#89771=CARTESIAN_POINT('Ctrl Pts',(-0.566813667614349,-2.30309663461945,
2.05801790885964));
#89772=CARTESIAN_POINT('Ctrl Pts',(-0.584538278609191,-2.29866197916364,
2.05675757471618));
#89773=CARTESIAN_POINT('Ctrl Pts',(-0.60883021444775,-2.29228503294966,
2.05504017565372));
#89774=CARTESIAN_POINT('Ctrl Pts',(-0.615442436888273,-2.29051861204719,
2.05457371798211));
#89775=CARTESIAN_POINT('Ctrl Pts',(-0.626743874510441,-2.28744701976707,
2.05377830879206));
#89776=CARTESIAN_POINT('Ctrl Pts',(-0.631436839247676,-2.28615600334246,
2.05344855895873));
#89777=CARTESIAN_POINT('Ctrl Pts',(-0.641181736044021,-2.28344292400903,
2.0527650218046));
#89778=CARTESIAN_POINT('Ctrl Pts',(-0.646232952666576,-2.28201853133619,
2.0524113840728));
#89779=CARTESIAN_POINT('Ctrl Pts',(-0.658437109372578,-2.27853331025056,
2.05155850187604));
#89780=CARTESIAN_POINT('Ctrl Pts',(-0.665585237920955,-2.27645552729718,
2.05106023482164));
#89781=CARTESIAN_POINT('Ctrl Pts',(-0.690615007887174,-2.2690520228246,
2.04931960577326));
#89782=CARTESIAN_POINT('Ctrl Pts',(-0.708444054436159,-2.2635488170332,
2.04808707765989));
#89783=CARTESIAN_POINT('Ctrl Pts',(-0.752117415395505,-2.24950178005459,
2.04508176292201));
#89784=CARTESIAN_POINT('Ctrl Pts',(-0.77788369401656,-2.24072219656346,
2.04332071290167));
#89785=CARTESIAN_POINT('Ctrl Pts',(-0.979353671698342,-2.16817909300825,
2.02960367271257));
#89786=CARTESIAN_POINT('Ctrl Pts',(-1.14712811172788,-2.08428559385173,
2.01845457026305));
#89787=CARTESIAN_POINT('Ctrl Pts',(-1.39866341320645,-1.91884358646531,
1.99981857520511));
#89788=CARTESIAN_POINT('Ctrl Pts',(-1.48934132143161,-1.84934508542921,
1.99263234211975));
#89789=CARTESIAN_POINT('Ctrl Pts',(-1.58839601014194,-1.76140104583153,
1.98397943805746));
#89790=CARTESIAN_POINT('Ctrl Pts',(-1.60199082627184,-1.74904570854021,
1.98277307534447));
#89791=CARTESIAN_POINT('Ctrl Pts',(-1.62393190348548,-1.72863464610982,
1.9807942629888));
#89792=CARTESIAN_POINT('Ctrl Pts',(-1.63236518286793,-1.72067326025132,
1.98002582700524));
#89793=CARTESIAN_POINT('Ctrl Pts',(-1.64734697982213,-1.70632051974592,
1.97864633423306));
#89794=CARTESIAN_POINT('Ctrl Pts',(-1.65391758477715,-1.69995247191225,
1.97803629515263));
#89795=CARTESIAN_POINT('Ctrl Pts',(-1.66656174174637,-1.68755540894127,
1.97685247814919));
#89796=CARTESIAN_POINT('Ctrl Pts',(-1.67263984433204,-1.68153122038186,
1.97627891777883));
#89797=CARTESIAN_POINT('Ctrl Pts',(-1.68882848120876,-1.66531156031195,
1.97473908075235));
#89798=CARTESIAN_POINT('Ctrl Pts',(-1.69887912232864,-1.65505708171102,
1.97377018700507));
#89799=CARTESIAN_POINT('Ctrl Pts',(-1.7395503242715,-1.61280019994762,1.9697957019647));
#89800=CARTESIAN_POINT('Ctrl Pts',(-1.76936292228399,-1.58003614038908,
1.96675575715211));
#89801=CARTESIAN_POINT('Ctrl Pts',(-1.84435648524047,-1.49283279205689,
1.95876454216031));
#89802=CARTESIAN_POINT('Ctrl Pts',(-1.88804782304586,-1.43717583196341,
1.95375879449328));
#89803=CARTESIAN_POINT('Ctrl Pts',(-1.97607022494181,-1.31409326855003,
1.94289981546531));
#89804=CARTESIAN_POINT('Ctrl Pts',(-2.0195814065101,-1.24618790615456,1.93703226972127));
#89805=CARTESIAN_POINT('Ctrl Pts',(-2.12991662313723,-1.05298929952,1.92078355393102));
#89806=CARTESIAN_POINT('Ctrl Pts',(-2.18909162317828,-0.923697420941236,
1.91038241703514));
#89807=CARTESIAN_POINT('Ctrl Pts',(-2.24265835185452,-0.772036079430949,
1.89919481253991));
#89808=CARTESIAN_POINT('Ctrl Pts',(-2.24874729671578,-0.75411659808541,
1.89788862536016));
#89809=CARTESIAN_POINT('Ctrl Pts',(-2.25701261235393,-0.72880140648472,
1.89606717479653));
#89810=CARTESIAN_POINT('Ctrl Pts',(-2.25936822820612,-0.72146561664592,
1.89554215352828));
#89811=CARTESIAN_POINT('Ctrl Pts',(-2.26326757594523,-0.709115971272732,
1.89466313509022));
#89812=CARTESIAN_POINT('Ctrl Pts',(-2.26483048032696,-0.704108285893273,
1.89430803391391));
#89813=CARTESIAN_POINT('Ctrl Pts',(-2.26798326299849,-0.693887372182228,
1.89358603075452));
#89814=CARTESIAN_POINT('Ctrl Pts',(-2.26957180670773,-0.688673785077757,
1.89321920737618));
#89815=CARTESIAN_POINT('Ctrl Pts',(-2.27356891667768,-0.675391257562155,
1.89228827019927));
#89816=CARTESIAN_POINT('Ctrl Pts',(-2.27595253453937,-0.667314794982954,
1.89172559438466));
#89817=CARTESIAN_POINT('Ctrl Pts',(-2.2854279574098,-0.634567600332631,
1.88945716464447));
#89818=CARTESIAN_POINT('Ctrl Pts',(-2.29216236482781,-0.609794076340319,
1.88777091797322));
#89819=CARTESIAN_POINT('Ctrl Pts',(-2.34697257601765,-0.394410731675212,
1.87332845728201));
#89820=CARTESIAN_POINT('Ctrl Pts',(-2.37158441769536,-0.198601548167095,
1.86161808344996));
#89821=CARTESIAN_POINT('Ctrl Pts',(-2.37174916735844,-0.00198736875130605,
1.84947704601095));
#89822=CARTESIAN_POINT('Ctrl Pts',(-2.37174916921441,-0.00198515257602363,
1.84947690916085));
#89823=CARTESIAN_POINT('Ctrl Pts',(-2.37179808021083,0.056450967917035,
1.84586844475866));
#89824=CARTESIAN_POINT('Ctrl Pts',(-2.36968731411222,0.114844513390865,
1.84223362268876));
#89825=CARTESIAN_POINT('Ctrl Pts',(-2.36542648301433,0.173076907629062,
1.83854786047046));
#89826=CARTESIAN_POINT('Ctrl Pts',(-2.36542650134104,0.173076657159373,
1.6387748639739));
#89827=CARTESIAN_POINT('Ctrl Pts',(-2.36960866311417,0.115919346327277,
1.64233205486039));
#89828=CARTESIAN_POINT('Ctrl Pts',(-2.3717210489944,0.0585847397316989,
1.64592561797024));
#89829=CARTESIAN_POINT('Ctrl Pts',(-2.37177718696143,-0.0538671038640167,
1.65307890001155));
#89830=CARTESIAN_POINT('Ctrl Pts',(-2.36988797458106,-0.108898665586173,
1.65662887810539));
#89831=CARTESIAN_POINT('Ctrl Pts',(-2.36492762284214,-0.180545786629185,
1.661338529028));
#89832=CARTESIAN_POINT('Ctrl Pts',(-2.36359158010639,-0.197266978274198,
1.66244389580054));
#89833=CARTESIAN_POINT('Ctrl Pts',(-2.36115356912776,-0.224180622973592,
1.6642336739387));
#89834=CARTESIAN_POINT('Ctrl Pts',(-2.36016267298024,-0.234382764222406,
1.66491458962881));
#89835=CARTESIAN_POINT('Ctrl Pts',(-2.35814538825979,-0.253840717673803,
1.66621811164116));
#89836=CARTESIAN_POINT('Ctrl Pts',(-2.35713055506391,-0.263097556494081,
1.66684034261606));
#89837=CARTESIAN_POINT('Ctrl Pts',(-2.35468027003334,-0.284294775500551,
1.66827011588567));
#89838=CARTESIAN_POINT('Ctrl Pts',(-2.35320847105944,-0.296230612731584,
1.66907878953395));
#89839=CARTESIAN_POINT('Ctrl Pts',(-2.34835554719776,-0.333265142479105,
1.67159938964166));
#89840=CARTESIAN_POINT('Ctrl Pts',(-2.34466324693694,-0.358320530915857,
1.67332106147969));
#89841=CARTESIAN_POINT('Ctrl Pts',(-2.32475587553721,-0.479878710264843,
1.68175676352726));
#89842=CARTESIAN_POINT('Ctrl Pts',(-2.30298229721019,-0.575362019405487,
1.68864375829141));
#89843=CARTESIAN_POINT('Ctrl Pts',(-2.22805682500464,-0.830112927903093,
1.70770542951043));
#89844=CARTESIAN_POINT('Ctrl Pts',(-2.16380798862314,-0.985522392842536,
1.72012008919406));
#89845=CARTESIAN_POINT('Ctrl Pts',(-2.05290309707372,-1.18951539834122,
1.73681252166438));
#89846=CARTESIAN_POINT('Ctrl Pts',(-2.01979431203779,-1.24490587947179,
1.74138379174626));
#89847=CARTESIAN_POINT('Ctrl Pts',(-1.97856176638615,-1.30790198260453,
1.74657210707806));
#89848=CARTESIAN_POINT('Ctrl Pts',(-1.97259685623466,-1.31688113104749,
1.74731134604191));
#89849=CARTESIAN_POINT('Ctrl Pts',(-1.96284318392614,-1.33134862602584,
1.74850158332934));
#89850=CARTESIAN_POINT('Ctrl Pts',(-1.95909221363581,-1.33686208336675,
1.74895497253596));
#89851=CARTESIAN_POINT('Ctrl Pts',(-1.95237735076523,-1.3466431366851,1.74975883545705));
#89852=CARTESIAN_POINT('Ctrl Pts',(-1.94942264367262,-1.35091687958915,
1.75010991136192));
#89853=CARTESIAN_POINT('Ctrl Pts',(-1.9429926839962,-1.36015226547633,1.75086819954687));
#89854=CARTESIAN_POINT('Ctrl Pts',(-1.93951246334868,-1.36511031127238,
1.75127506757081));
#89855=CARTESIAN_POINT('Ctrl Pts',(-1.92969355646658,-1.37898532588265,
1.75241322610954));
#89856=CARTESIAN_POINT('Ctrl Pts',(-1.92331201055418,-1.38787199426419,
1.75314166310371));
#89857=CARTESIAN_POINT('Ctrl Pts',(-1.88400681211253,-1.44181496092983,
1.75756224076753));
#89858=CARTESIAN_POINT('Ctrl Pts',(-1.84955995273617,-1.48574600793919,
1.7611577073597));
#89859=CARTESIAN_POINT('Ctrl Pts',(-1.71758436786876,-1.64234507337006,
1.77412607853238));
#89860=CARTESIAN_POINT('Ctrl Pts',(-1.61104992035398,-1.74697402619156,
1.78311157905132));
#89861=CARTESIAN_POINT('Ctrl Pts',(-1.39149335244066,-1.92532163242049,
1.80052847758672));
#89862=CARTESIAN_POINT('Ctrl Pts',(-1.28064751275175,-2.00076276880269,
1.80889252556014));
#89863=CARTESIAN_POINT('Ctrl Pts',(-1.14753597617226,-2.0757451907461,1.81886663680873));
#89864=CARTESIAN_POINT('Ctrl Pts',(-1.13092069824292,-2.08484417969762,
1.8201100759378));
#89865=CARTESIAN_POINT('Ctrl Pts',(-1.10373114491279,-2.09931327301803,
1.82214330128084));
#89866=CARTESIAN_POINT('Ctrl Pts',(-1.09322223253599,-2.10480493161774,
1.8229287781269));
#89867=CARTESIAN_POINT('Ctrl Pts',(-1.07440395123258,-2.11445987972742,
1.82433487949348));
#89868=CARTESIAN_POINT('Ctrl Pts',(-1.06611039875946,-2.11865359292916,
1.8249544187976));
#89869=CARTESIAN_POINT('Ctrl Pts',(-1.04853385295497,-2.12741200283253,
1.82626719428472));
#89870=CARTESIAN_POINT('Ctrl Pts',(-1.03924523799089,-2.13196491528773,
1.82696082617108));
#89871=CARTESIAN_POINT('Ctrl Pts',(-1.01443641358905,-2.14392456919899,
1.82881327156069));
#89872=CARTESIAN_POINT('Ctrl Pts',(-0.998865171384125,-2.15122340490828,
1.8299757898895));
#89873=CARTESIAN_POINT('Ctrl Pts',(-0.922597474088439,-2.18596641186419,
1.83567011632628));
#89874=CARTESIAN_POINT('Ctrl Pts',(-0.860848042614488,-2.2110120693348,
1.84028272111396));
#89875=CARTESIAN_POINT('Ctrl Pts',(-0.55161147521398,-2.32152016902032,
1.86341125685316));
#89876=CARTESIAN_POINT('Ctrl Pts',(-0.292265328172684,-2.3681796462979,
1.88315671105829));
#89877=CARTESIAN_POINT('Ctrl Pts',(-0.00805945332513304,-2.37184314805694,
1.90300287202571));
#89878=CARTESIAN_POINT('Ctrl Pts',(0.0144551904437281,-2.37181281189842,
1.904561106136));
#89879=CARTESIAN_POINT('Ctrl Pts',(0.0453074398984561,-2.3713318785506,
1.90667422344017));
#89880=CARTESIAN_POINT('Ctrl Pts',(0.0536472955290461,-2.37115786385569,
1.90724321209398));
#89881=CARTESIAN_POINT('Ctrl Pts',(0.0669243505919645,-2.3708107464807,
1.90814532348815));
#89882=CARTESIAN_POINT('Ctrl Pts',(0.0718621270061494,-2.37066621441762,
1.90848000221215));
#89883=CARTESIAN_POINT('Ctrl Pts',(0.0821216854233761,-2.37033382605763,
1.90917363489297));
#89884=CARTESIAN_POINT('Ctrl Pts',(0.0874433193823489,-2.3701434734459,
1.90953243528803));
#89885=CARTESIAN_POINT('Ctrl Pts',(0.100315498453076,-2.36963962894656,
1.91039801822529));
#89886=CARTESIAN_POINT('Ctrl Pts',(0.107865361284689,-2.36930796607062,
1.91090379380933));
#89887=CARTESIAN_POINT('Ctrl Pts',(0.134361159951856,-2.36801710336895,
1.91267248061633));
#89888=CARTESIAN_POINT('Ctrl Pts',(0.153297668416236,-2.36686666386296,
1.91392524257181));
#89889=CARTESIAN_POINT('Ctrl Pts',(0.270708846490515,-2.35831856107061,
1.92163378137981));
#89890=CARTESIAN_POINT('Ctrl Pts',(0.368667254409959,-2.34500296920853,
1.92780970694033));
#89891=CARTESIAN_POINT('Ctrl Pts',(0.623485683637577,-2.29399575005869,
1.94385026179236));
#89892=CARTESIAN_POINT('Ctrl Pts',(0.77781166374246,-2.24636568389503,1.95356615447729));
#89893=CARTESIAN_POINT('Ctrl Pts',(0.991785427209705,-2.15560843666167,
1.96821505579086));
#89894=CARTESIAN_POINT('Ctrl Pts',(1.05615719325343,-2.1248097545131,1.97278325831184));
#89895=CARTESIAN_POINT('Ctrl Pts',(1.13499087013338,-2.08262361320781,1.97863674111826));
#89896=CARTESIAN_POINT('Ctrl Pts',(1.15084407995003,-2.07390531682452,1.97982736881521));
#89897=CARTESIAN_POINT('Ctrl Pts',(1.17586370069562,-2.0597708443004,1.98172878532738));
#89898=CARTESIAN_POINT('Ctrl Pts',(1.18509627619574,-2.05447272639503,1.98243533726153));
#89899=CARTESIAN_POINT('Ctrl Pts',(1.2022852473987,-2.04445440795957,1.9837601368272));
#89900=CARTESIAN_POINT('Ctrl Pts',(1.21025032576496,-2.03974944224587,1.98437782339233));
#89901=CARTESIAN_POINT('Ctrl Pts',(1.22796466447456,-2.02914531055221,1.98576017204667));
#89902=CARTESIAN_POINT('Ctrl Pts',(1.23769929297568,-2.02322227172872,1.9865256962754));
#89903=CARTESIAN_POINT('Ctrl Pts',(1.26620401986214,-2.00559585223416,1.9887848843073));
#89904=CARTESIAN_POINT('Ctrl Pts',(1.28485307724654,-1.99370004123265,1.99028560297049));
#89905=CARTESIAN_POINT('Ctrl Pts',(1.42704076453219,-1.90017817445824,2.00190693758804));
#89906=CARTESIAN_POINT('Ctrl Pts',(1.54283433512278,-1.80742073632707,2.01245598405812));
#89907=CARTESIAN_POINT('Ctrl Pts',(1.76550242867467,-1.59197487330605,2.03498243151264));
#89908=CARTESIAN_POINT('Ctrl Pts',(1.86997795541834,-1.4678453320116,2.04694403924147));
#89909=CARTESIAN_POINT('Ctrl Pts',(1.9778778492428,-1.30923539062315,2.06043308706646));
#89910=CARTESIAN_POINT('Ctrl Pts',(1.99428112798441,-1.28411101093527,2.0625203676908));
#89911=CARTESIAN_POINT('Ctrl Pts',(2.01515941361527,-1.25076687813245,2.06521975799979));
#89912=CARTESIAN_POINT('Ctrl Pts',(2.02006796429726,-1.24282366918957,2.06585763806313));
#89913=CARTESIAN_POINT('Ctrl Pts',(2.02789948908344,-1.22998140756852,2.06688038601462));
#89914=CARTESIAN_POINT('Ctrl Pts',(2.03085185959194,-1.22510053748358,2.06726712099598));
#89915=CARTESIAN_POINT('Ctrl Pts',(2.03650595413957,-1.21567656017414,2.06800996259131));
#89916=CARTESIAN_POINT('Ctrl Pts',(2.03921011884692,-1.21113504281481,2.06836621867915));
#89917=CARTESIAN_POINT('Ctrl Pts',(2.04563202130727,-1.2002672775886,2.06921469604775));
#89918=CARTESIAN_POINT('Ctrl Pts',(2.0493356654387,-1.19393267742906,2.06970600890315));
#89919=CARTESIAN_POINT('Ctrl Pts',(2.06183417112514,-1.17232610189998,2.07137116293955));
#89920=CARTESIAN_POINT('Ctrl Pts',(2.0704884552349,-1.15697287819407,2.07253636998755));
#89921=CARTESIAN_POINT('Ctrl Pts',(2.11986367385172,-1.06704954035079,2.07926526456413));
#89922=CARTESIAN_POINT('Ctrl Pts',(2.15672970114372,-0.99042263836784,2.08462047719697));
#89923=CARTESIAN_POINT('Ctrl Pts',(2.22726789245448,-0.821079263496044,
2.09600422192559));
#89924=CARTESIAN_POINT('Ctrl Pts',(2.25943296622754,-0.727912820277594,
2.1019954441008));
#89925=CARTESIAN_POINT('Ctrl Pts',(2.32431094794245,-0.493648901755764,
2.11693155945737));
#89926=CARTESIAN_POINT('Ctrl Pts',(2.35007550830609,-0.351065642441476,
2.12592863611524));
#89927=CARTESIAN_POINT('Ctrl Pts',(2.36436023085634,-0.18804802703086,2.13661065817768));
#89928=CARTESIAN_POINT('Ctrl Pts',(2.36579506824295,-0.169041480099765,
2.13786165827944));
#89929=CARTESIAN_POINT('Ctrl Pts',(2.3677528348711,-0.138152063751828,2.13990476592596));
#89930=CARTESIAN_POINT('Ctrl Pts',(2.36841575047315,-0.126278675743689,
2.14069249265964));
#89931=CARTESIAN_POINT('Ctrl Pts',(2.3694377699601,-0.105114930825181,2.14210105298806));
#89932=CARTESIAN_POINT('Ctrl Pts',(2.36983159409495,-0.0958264357804435,
2.14272078625121));
#89933=CARTESIAN_POINT('Ctrl Pts',(2.37054746237549,-0.0762192142190349,
2.14403233757156));
#89934=CARTESIAN_POINT('Ctrl Pts',(2.37085676323617,-0.0659002455208639,
2.14472454165748));
#89935=CARTESIAN_POINT('Ctrl Pts',(2.37149951559256,-0.0384796487041291,
2.14656929693222));
#89936=CARTESIAN_POINT('Ctrl Pts',(2.37171534331981,-0.0213761388779025,
2.14772549964854));
#89937=CARTESIAN_POINT('Ctrl Pts',(2.37186413371387,0.0612265397337218,
2.15333734299061));
#89938=CARTESIAN_POINT('Ctrl Pts',(2.36926884517759,0.126695860115009,2.15787097884521));
#89939=CARTESIAN_POINT('Ctrl Pts',(2.34412911014829,0.436275167414346,2.17973302915143));
#89940=CARTESIAN_POINT('Ctrl Pts',(2.28654803409132,0.675974835079976,2.19811804365447));
#89941=CARTESIAN_POINT('Ctrl Pts',(2.17923234400931,0.936755134417593,2.21805908819881));
#89942=CARTESIAN_POINT('Ctrl Pts',(2.16437082333313,0.970599355541919,2.22064125488903));
#89943=CARTESIAN_POINT('Ctrl Pts',(2.14445520943913,1.01321841682862,2.22387331363644));
#89944=CARTESIAN_POINT('Ctrl Pts',(2.14012876240169,1.02232509263733,2.22456276599095));
#89945=CARTESIAN_POINT('Ctrl Pts',(2.13319184158391,1.03668948080599,2.22564810929301));
#89946=CARTESIAN_POINT('Ctrl Pts',(2.13061975664414,1.04196543470679,2.22604628475393));
#89947=CARTESIAN_POINT('Ctrl Pts',(2.12571867051075,1.0519246894908,2.22679695187334));
#89948=CARTESIAN_POINT('Ctrl Pts',(2.1233937899295,1.05660978226665,2.22714967323411));
#89949=CARTESIAN_POINT('Ctrl Pts',(2.11793147937511,1.06752657395764,2.22797065054157));
#89950=CARTESIAN_POINT('Ctrl Pts',(2.11478203029549,1.07375216176969,2.22843815152538));
#89951=CARTESIAN_POINT('Ctrl Pts',(2.10452396727163,1.09380929425726,2.22994239552722));
#89952=CARTESIAN_POINT('Ctrl Pts',(2.09730659357699,1.10758520460344,2.23097260674337));
#89953=CARTESIAN_POINT('Ctrl Pts',(2.03090970681291,1.23134131729201,2.24020983144616));
#89954=CARTESIAN_POINT('Ctrl Pts',(1.96325598583339,1.33657421394242,2.24794287603437));
#89955=CARTESIAN_POINT('Ctrl Pts',(1.76903805169605,1.59187311075522,2.26764663079275));
#89956=CARTESIAN_POINT('Ctrl Pts',(1.63162442350609,1.73243996059345,2.27951338710829));
#89957=CARTESIAN_POINT('Ctrl Pts',(1.45672768822789,1.87187554817997,2.29402701187766));
#89958=CARTESIAN_POINT('Ctrl Pts',(1.4346488056877,1.88885052957419,2.29584816668067));
#89959=CARTESIAN_POINT('Ctrl Pts',(1.40234856569355,1.91279096742626,2.29849951871082));
#89960=CARTESIAN_POINT('Ctrl Pts',(1.39236304498143,1.9200718543782,2.2993174331287));
#89961=CARTESIAN_POINT('Ctrl Pts',(1.37468846992077,1.93274879455816,2.30076235588069));
#89962=CARTESIAN_POINT('Ctrl Pts',(1.36702334408375,1.93817787227381,2.30138807618843));
#89963=CARTESIAN_POINT('Ctrl Pts',(1.35112354801326,1.94929818600801,2.30268424053735));
#89964=CARTESIAN_POINT('Ctrl Pts',(1.34288470595795,1.95498309996488,2.30335490899979));
#89965=CARTESIAN_POINT('Ctrl Pts',(1.32165372898751,1.96943523371533,2.30508085482682));
#89966=CARTESIAN_POINT('Ctrl Pts',(1.30861039832795,1.97812601316198,2.30613898681733));
#89967=CARTESIAN_POINT('Ctrl Pts',(1.25319502978267,2.01426136415358,2.31062604048716));
#89968=CARTESIAN_POINT('Ctrl Pts',(1.21004134444709,2.04047687902,2.31409992764073));
#89969=CARTESIAN_POINT('Ctrl Pts',(1.09238945039114,2.1069043838649,2.32352501594766));
#89970=CARTESIAN_POINT('Ctrl Pts',(1.01652511643256,2.14453604655934,2.32955733007252));
#89971=CARTESIAN_POINT('Ctrl Pts',(0.819760225371631,2.22934965965042,2.34504151968247));
#89972=CARTESIAN_POINT('Ctrl Pts',(0.69669892548546,2.27081829646661,2.35458844850216));
#89973=CARTESIAN_POINT('Ctrl Pts',(0.537286379423254,2.31035029855108,2.36647375759433));
#89974=CARTESIAN_POINT('Ctrl Pts',(0.503525002569843,2.31794260275288,2.3689633315658));
#89975=CARTESIAN_POINT('Ctrl Pts',(0.421715986099231,2.33446802564574,2.37491317167566));
#89976=CARTESIAN_POINT('Ctrl Pts',(0.373531839123247,2.34266090513998,2.3783494841183));
#89977=CARTESIAN_POINT('Ctrl Pts',(0.314304128349166,2.35085735705827,2.38246405929072));
#89978=CARTESIAN_POINT('Ctrl Pts',(0.303472679759252,2.3522801156695,2.38321207156198));
#89979=CARTESIAN_POINT('Ctrl Pts',(0.286557972724072,2.35438315680863,2.38437284754635));
#89980=CARTESIAN_POINT('Ctrl Pts',(0.280481430386411,2.35511479341488,2.38478837612026));
#89981=CARTESIAN_POINT('Ctrl Pts',(0.269247261819074,2.35642332926689,2.38555378563432));
#89982=CARTESIAN_POINT('Ctrl Pts',(0.264090603257937,2.3570068198735,2.38590401845155));
#89983=CARTESIAN_POINT('Ctrl Pts',(0.25238769815482,2.35829214805742,2.3866963951548));
#89984=CARTESIAN_POINT('Ctrl Pts',(0.245840425121376,2.35898365695781,2.38713795626461));
#89985=CARTESIAN_POINT('Ctrl Pts',(0.225881602952458,2.36100766727362,2.38847895365899));
#89986=CARTESIAN_POINT('Ctrl Pts',(0.212461211775942,2.36225315283245,2.38937368273893));
#89987=CARTESIAN_POINT('Ctrl Pts',(0.0670993162521076,2.37449469074952,
2.39899667922873));
#89988=CARTESIAN_POINT('Ctrl Pts',(-0.0655520068355683,2.37454017721609,
2.40717757634515));
#89989=CARTESIAN_POINT('Ctrl Pts',(-0.387716209696517,2.34761524772513,
2.42702233789465));
#89990=CARTESIAN_POINT('Ctrl Pts',(-0.575263906429226,2.30882726396974,
2.43860850260362));
#89991=CARTESIAN_POINT('Ctrl Pts',(-0.780276063690914,2.23986970219647,
2.45263828936978));
#89992=CARTESIAN_POINT('Ctrl Pts',(-0.804288192889097,2.23135999779909,
2.45430245736106));
#89993=CARTESIAN_POINT('Ctrl Pts',(-0.841002332520498,2.2176791985312,2.45688162814132));
#89994=CARTESIAN_POINT('Ctrl Pts',(-0.853804833542295,2.21278178857598,
2.45778756799049));
#89995=CARTESIAN_POINT('Ctrl Pts',(-0.874604653098438,2.2046177393872,2.45927047383288));
#89996=CARTESIAN_POINT('Ctrl Pts',(-0.882627970853697,2.20141784714506,
2.45984519114634));
#89997=CARTESIAN_POINT('Ctrl Pts',(-0.899454174854711,2.19460037953907,
2.461056248504));
#89998=CARTESIAN_POINT('Ctrl Pts',(-0.908253105723912,2.19097351191484,
2.4616928938984));
#89999=CARTESIAN_POINT('Ctrl Pts',(-0.929040267897562,2.18225842839452,
2.46320501506593));
#90000=CARTESIAN_POINT('Ctrl Pts',(-0.94100878454581,2.17712427832885,2.46408203803548));
#90001=CARTESIAN_POINT('Ctrl Pts',(-0.981558555028009,2.15933275601394,
2.46707563419829));
#90002=CARTESIAN_POINT('Ctrl Pts',(-1.00993056256718,2.14620950610422,2.46920802572197));
#90003=CARTESIAN_POINT('Ctrl Pts',(-1.07767154971281,2.11323579100419,2.47439374838691));
#90004=CARTESIAN_POINT('Ctrl Pts',(-1.11676128292594,2.092841436974,2.47746495517489));
#90005=CARTESIAN_POINT('Ctrl Pts',(-1.27098798403305,2.00682515200285,2.48990337888791));
#90006=CARTESIAN_POINT('Ctrl Pts',(-1.38109234372028,1.9327011873576,2.49953657173183));
#90007=CARTESIAN_POINT('Ctrl Pts',(-1.5882657024881,1.76644810497361,2.51893916695932));
#90008=CARTESIAN_POINT('Ctrl Pts',(-1.68492071811759,1.67450774250247,2.52867240873933));
#90009=CARTESIAN_POINT('Ctrl Pts',(-1.78609983330084,1.56058124554427,2.53927389283346));
#90010=CARTESIAN_POINT('Ctrl Pts',(-1.7986706465424,1.54607580761492,2.54059895501348));
#90011=CARTESIAN_POINT('Ctrl Pts',(-1.81610960099893,1.52545240199469,2.54244650263615));
#90012=CARTESIAN_POINT('Ctrl Pts',(-1.82112530082274,1.51946100860762,2.5429790002577));
#90013=CARTESIAN_POINT('Ctrl Pts',(-1.82950673886376,1.50934802717908,2.54387055359561));
#90014=CARTESIAN_POINT('Ctrl Pts',(-1.83288834822098,1.50523974156532,2.54423074264525));
#90015=CARTESIAN_POINT('Ctrl Pts',(-1.8397582844834,1.49683604134153,2.54496340982437));
#90016=CARTESIAN_POINT('Ctrl Pts',(-1.84324544983761,1.49253974595222,2.5453358052255));
#90017=CARTESIAN_POINT('Ctrl Pts',(-1.85209113095659,1.48156330988285,2.54628182071857));
#90018=CARTESIAN_POINT('Ctrl Pts',(-1.85742861932592,1.47486620692848,2.54685395242977));
#90019=CARTESIAN_POINT('Ctrl Pts',(-1.87896812733793,1.44753756110674,2.54916882430191));
#90020=CARTESIAN_POINT('Ctrl Pts',(-1.89486435107056,1.4266658501725,2.55089122107487));
#90021=CARTESIAN_POINT('Ctrl Pts',(-2.01761659093699,1.25982008788307,2.56434300730369));
#90022=CARTESIAN_POINT('Ctrl Pts',(-2.10781327456002,1.10229981245227,2.57519302598397));
#90023=CARTESIAN_POINT('Ctrl Pts',(-2.20487199990845,0.876333053352151,
2.59032852451187));
#90024=CARTESIAN_POINT('Ctrl Pts',(-2.22805070696789,0.815603780212274,
2.59435328726515));
#90025=CARTESIAN_POINT('Ctrl Pts',(-2.27263976342893,0.682623132077742,
2.60317515425029));
#90026=CARTESIAN_POINT('Ctrl Pts',(-2.29315914998258,0.610151739996926,
2.6079888559906));
#90027=CARTESIAN_POINT('Ctrl Pts',(-2.31435896754865,0.518920793631756,
2.61411862348711));
#90028=CARTESIAN_POINT('Ctrl Pts',(-2.31831267809239,0.500961591130818,
2.61532850041726));
#90029=CARTESIAN_POINT('Ctrl Pts',(-2.3242384920234,0.472470376827446,2.61725376837726));
#90030=CARTESIAN_POINT('Ctrl Pts',(-2.3263488025736,0.461967603992343,2.6179647378172));
#90031=CARTESIAN_POINT('Ctrl Pts',(-2.33014774546769,0.442374310960973,
2.61929357177407));
#90032=CARTESIAN_POINT('Ctrl Pts',(-2.33185451964203,0.433287481653748,
2.61991084460867));
#90033=CARTESIAN_POINT('Ctrl Pts',(-2.33509298476828,0.415472430566613,
2.62112307619704));
#90034=CARTESIAN_POINT('Ctrl Pts',(-2.33662897736577,0.406745137039638,
2.62171788683566));
#90035=CARTESIAN_POINT('Ctrl Pts',(-2.33997165757585,0.3871084869775,2.62305846729474));
#90036=CARTESIAN_POINT('Ctrl Pts',(-2.34175102017584,0.376194751720824,
2.62380509119799));
#90037=CARTESIAN_POINT('Ctrl Pts',(-2.34604114327896,0.348670646471449,
2.62569211847097));
#90038=CARTESIAN_POINT('Ctrl Pts',(-2.34845183229614,0.332045526566707,
2.62683564431836));
#90039=CARTESIAN_POINT('Ctrl Pts',(-2.35703167715799,0.268098989516441,
2.63124902139752));
#90040=CARTESIAN_POINT('Ctrl Pts',(-2.3619465149035,0.220637391362148,2.63455631919237));
#90041=CARTESIAN_POINT('Ctrl Pts',(-2.36542650247982,0.173076641595803,
2.63790316127816));
#90042=CARTESIAN_POINT('Origin',(0.,0.,-1.84858989190503));
#90043=CARTESIAN_POINT('',(-2.36542646296203,0.17307718168185,3.83677864400945));
#90044=CARTESIAN_POINT('',(-2.36847158556395,0.173320321679478,3.63969887294137));
#90045=CARTESIAN_POINT('',(-2.36542649454111,0.173076750093529,-1.84858989190503));
#90046=CARTESIAN_POINT('Ctrl Pts',(-2.36542646296204,0.173077181681802,
3.83677864400945));
#90047=CARTESIAN_POINT('Ctrl Pts',(-2.35656887892582,0.29413279093999,3.82791154518428));
#90048=CARTESIAN_POINT('Ctrl Pts',(-2.33842529469647,0.414417477642174,
3.81903475289074));
#90049=CARTESIAN_POINT('Ctrl Pts',(-2.30685655361473,0.551334760411727,
3.80917456728547));
#90050=CARTESIAN_POINT('Ctrl Pts',(-2.30237760527083,0.569749587144351,
3.80785386742358));
#90051=CARTESIAN_POINT('Ctrl Pts',(-2.29522651061167,0.597688121299326,
3.805860428478));
#90052=CARTESIAN_POINT('Ctrl Pts',(-2.29271483377461,0.607251615593695,
3.80517991262023));
#90053=CARTESIAN_POINT('Ctrl Pts',(-2.2879480781524,0.624950327913153,3.80392429428456));
#90054=CARTESIAN_POINT('Ctrl Pts',(-2.28570924283121,0.633089711975873,
3.80334834234869));
#90055=CARTESIAN_POINT('Ctrl Pts',(-2.28195222982755,0.646468744496542,
3.80240427745691));
#90056=CARTESIAN_POINT('Ctrl Pts',(-2.28045937203958,0.65171532961237,3.80203473584951));
#90057=CARTESIAN_POINT('Ctrl Pts',(-2.27749625386085,0.661994230146577,
3.80131212978613));
#90058=CARTESIAN_POINT('Ctrl Pts',(-2.27602739088326,0.667026883975227,
3.80095899142415));
#90059=CARTESIAN_POINT('Ctrl Pts',(-2.27236340333756,0.679427501577436,
3.80009037572077));
#90060=CARTESIAN_POINT('Ctrl Pts',(-2.27014909308326,0.686789826694812,
3.79957600631263));
#90061=CARTESIAN_POINT('Ctrl Pts',(-2.26238952534064,0.712141889283573,
3.79780896609926));
#90062=CARTESIAN_POINT('Ctrl Pts',(-2.25666573966031,0.730076865422134,
3.79656618069694));
#90063=CARTESIAN_POINT('Ctrl Pts',(-2.20506092858362,0.885367462522205,
3.78585346629572));
#90064=CARTESIAN_POINT('Ctrl Pts',(-2.14689565500221,1.01834203679391,3.77699668770544));
#90065=CARTESIAN_POINT('Ctrl Pts',(-2.03403167844092,1.22303501917587,3.76267448642867));
#90066=CARTESIAN_POINT('Ctrl Pts',(-1.98677025343337,1.29840002093787,3.75723492263853));
#90067=CARTESIAN_POINT('Ctrl Pts',(-1.8823928743076,1.44575318359468,3.74597893702903));
#90068=CARTESIAN_POINT('Ctrl Pts',(-1.82510503389702,1.51743000952789,3.74016516949508));
#90069=CARTESIAN_POINT('Ctrl Pts',(-1.74970440788952,1.60130515005882,3.73280617770581));
#90070=CARTESIAN_POINT('Ctrl Pts',(-1.73538291934173,1.61681470011158,3.73142044335896));
#90071=CARTESIAN_POINT('Ctrl Pts',(-1.71456293996811,1.63876649756727,3.72942174838033));
#90072=CARTESIAN_POINT('Ctrl Pts',(-1.70823094212641,1.64536584170514,3.72881592934065));
#90073=CARTESIAN_POINT('Ctrl Pts',(-1.69539080688644,1.65859409454865,3.72759142424398));
#90074=CARTESIAN_POINT('Ctrl Pts',(-1.6888815803483,1.66522171553472,3.72697269666013));
#90075=CARTESIAN_POINT('Ctrl Pts',(-1.67625406469718,1.67792871210869,3.72577618594853));
#90076=CARTESIAN_POINT('Ctrl Pts',(-1.67014120874367,1.68401329916968,3.72519864863319));
#90077=CARTESIAN_POINT('Ctrl Pts',(-1.65393497670828,1.69996955269224,3.72367180830487));
#90078=CARTESIAN_POINT('Ctrl Pts',(-1.64378653537458,1.70978454734174,3.72272004649197));
#90079=CARTESIAN_POINT('Ctrl Pts',(-1.60747956938144,1.74427655561821,3.71932984637613));
#90080=CARTESIAN_POINT('Ctrl Pts',(-1.58084926410761,1.76844751834255,3.71686998597352));
#90081=CARTESIAN_POINT('Ctrl Pts',(-1.41759214870149,1.90999277741035,3.70193893214385));
#90082=CARTESIAN_POINT('Ctrl Pts',(-1.26852862893191,2.01207654313201,3.68885038268129));
#90083=CARTESIAN_POINT('Ctrl Pts',(-1.00216819019323,2.15303799366413,3.66683807474532));
#90084=CARTESIAN_POINT('Ctrl Pts',(-0.890742161834415,2.20147635933036,
3.65799911947042));
#90085=CARTESIAN_POINT('Ctrl Pts',(-0.756677877038248,2.24790093655933,
3.64811483551695));
#90086=CARTESIAN_POINT('Ctrl Pts',(-0.737179557286774,2.2543705113912,3.64669541061935));
#90087=CARTESIAN_POINT('Ctrl Pts',(-0.710086085275302,2.26297104328652,
3.6447504037421));
#90088=CARTESIAN_POINT('Ctrl Pts',(-0.70256136451534,2.26531845991792,3.6442131087879));
#90089=CARTESIAN_POINT('Ctrl Pts',(-0.689924408600538,2.26919166936752,
3.64331579021148));
#90090=CARTESIAN_POINT('Ctrl Pts',(-0.684818533596174,2.27073778752834,
3.64295460143326));
#90091=CARTESIAN_POINT('Ctrl Pts',(-0.675130587241533,2.27363576113205,
3.64227192246454));
#90092=CARTESIAN_POINT('Ctrl Pts',(-0.670549590521043,2.27499101796484,
3.64195022994878));
#90093=CARTESIAN_POINT('Ctrl Pts',(-0.658539022661996,2.27850483317734,
3.64110965250314));
#90094=CARTESIAN_POINT('Ctrl Pts',(-0.651102851013865,2.28064091886693,
3.64059206567495));
#90095=CARTESIAN_POINT('Ctrl Pts',(-0.625256367238367,2.28792875970234,
3.63880247710767));
#90096=CARTESIAN_POINT('Ctrl Pts',(-0.606793722784177,2.29289445240452,
3.63754070039832));
#90097=CARTESIAN_POINT('Ctrl Pts',(-0.461076736284444,2.33020290816188,
3.62769721174357));
#90098=CARTESIAN_POINT('Ctrl Pts',(-0.33137783749447,2.35215553918783,3.61961639691837));
#90099=CARTESIAN_POINT('Ctrl Pts',(-0.0680890373155831,2.37449453399542,
3.60341336567613));
#90100=CARTESIAN_POINT('Ctrl Pts',(0.0650362530732931,2.37457950498845,
3.59531504719973));
#90101=CARTESIAN_POINT('Ctrl Pts',(0.242549305730111,2.359748881488,3.58406372648677));
#90102=CARTESIAN_POINT('Ctrl Pts',(0.287515412286639,2.35469306867313,3.58117599946213));
#90103=CARTESIAN_POINT('Ctrl Pts',(0.363967415982026,2.34387461484409,3.57618248303863));
#90104=CARTESIAN_POINT('Ctrl Pts',(0.395532273510814,2.33875491460261,3.57409625264696));
#90105=CARTESIAN_POINT('Ctrl Pts',(0.439855407764579,2.33064294503791,3.57112779887556));
#90106=CARTESIAN_POINT('Ctrl Pts',(0.45270807554578,2.32818055651806,3.57026237543125));
#90107=CARTESIAN_POINT('Ctrl Pts',(0.474735912751121,2.32377103837879,3.56877087926951));
#90108=CARTESIAN_POINT('Ctrl Pts',(0.483921216123206,2.32187559483966,3.56814646768479));
#90109=CARTESIAN_POINT('Ctrl Pts',(0.501424639372227,2.31815528216538,3.56695175617748));
#90110=CARTESIAN_POINT('Ctrl Pts',(0.509744663805219,2.31633999137526,3.56638177208391));
#90111=CARTESIAN_POINT('Ctrl Pts',(0.531246865472527,2.31152711092782,3.56490319177167));
#90112=CARTESIAN_POINT('Ctrl Pts',(0.544413360712654,2.30846158644601,3.56399242662124));
#90113=CARTESIAN_POINT('Ctrl Pts',(0.581976703452959,2.29937656894219,3.56137828508119));
#90114=CARTESIAN_POINT('Ctrl Pts',(0.606304433679942,2.29308184285837,3.55966612363967));
#90115=CARTESIAN_POINT('Ctrl Pts',(0.81797356332401,2.2347093202272,3.54459642125485));
#90116=CARTESIAN_POINT('Ctrl Pts',(0.998316528553454,2.16017133425058,3.53047671027753));
#90117=CARTESIAN_POINT('Ctrl Pts',(1.18874885762807,2.0524789858063,3.51449816613163));
#90118=CARTESIAN_POINT('Ctrl Pts',(1.20980862417159,2.04013650115321,3.51271656952236));
#90119=CARTESIAN_POINT('Ctrl Pts',(1.31407415198159,1.97684736065122,3.50383236829042));
#90120=CARTESIAN_POINT('Ctrl Pts',(1.39428058270697,1.92112003507617,3.49678906957557));
#90121=CARTESIAN_POINT('Ctrl Pts',(1.48554773892454,1.84897209317764,3.48870178608658));
#90122=CARTESIAN_POINT('Ctrl Pts',(1.5001243895938,1.83716541372752,3.48740790681232));
#90123=CARTESIAN_POINT('Ctrl Pts',(1.52030046454166,1.82042308376525,3.48561565096546));
#90124=CARTESIAN_POINT('Ctrl Pts',(1.52601852448462,1.81563244439876,3.48510755759805));
#90125=CARTESIAN_POINT('Ctrl Pts',(1.53572306853161,1.80742366146491,3.48424511151257));
#90126=CARTESIAN_POINT('Ctrl Pts',(1.53972094846687,1.80401913466382,3.48388978357505));
#90127=CARTESIAN_POINT('Ctrl Pts',(1.54739980197971,1.7974358313931,3.48320727652981));
#90128=CARTESIAN_POINT('Ctrl Pts',(1.55108232729112,1.79425899195246,3.48287995526891));
#90129=CARTESIAN_POINT('Ctrl Pts',(1.55991262760528,1.78659377048854,3.48209496754698));
#90130=CARTESIAN_POINT('Ctrl Pts',(1.56505087620746,1.78209440386842,3.48163810479394));
#90131=CARTESIAN_POINT('Ctrl Pts',(1.58378223970907,1.76554857306769,3.47997198748051));
#90132=CARTESIAN_POINT('Ctrl Pts',(1.59725672555464,1.75336788755086,3.47877222681043));
#90133=CARTESIAN_POINT('Ctrl Pts',(1.7277773004169,1.63262625133592,3.46712281047167));
#90134=CARTESIAN_POINT('Ctrl Pts',(1.83373822845497,1.51264753172426,3.4574248484245));
#90135=CARTESIAN_POINT('Ctrl Pts',(2.02494378528427,1.24623601691947,3.43732824743916));
#90136=CARTESIAN_POINT('Ctrl Pts',(2.10820379873936,1.09953045784547,3.42695877263075));
#90137=CARTESIAN_POINT('Ctrl Pts',(2.18350817719913,0.926239887498326,3.41462019402099));
#90138=CARTESIAN_POINT('Ctrl Pts',(2.19152475239492,0.907109422104458,3.41325762701685));
#90139=CARTESIAN_POINT('Ctrl Pts',(2.20341226479273,0.877663807018112,3.4111585331563));
#90140=CARTESIAN_POINT('Ctrl Pts',(2.20746409568505,0.867422403498191,3.41042811981367));
#90141=CARTESIAN_POINT('Ctrl Pts',(2.21441559590764,0.849487623037795,3.40914827010957));
#90142=CARTESIAN_POINT('Ctrl Pts',(2.21734689078835,0.841806638172909,3.40859990726908));
#90143=CARTESIAN_POINT('Ctrl Pts',(2.22387542189401,0.824428975056821,3.40735866074647));
#90144=CARTESIAN_POINT('Ctrl Pts',(2.2274492667578,0.81472374775033,3.40666500753011));
#90145=CARTESIAN_POINT('Ctrl Pts',(2.23693798535761,0.788426775510335,3.40478417454047));
#90146=CARTESIAN_POINT('Ctrl Pts',(2.24273158882932,0.771792278964785,3.403592998043));
#90147=CARTESIAN_POINT('Ctrl Pts',(2.26885293220143,0.694014479618448,3.39801562237932));
#90148=CARTESIAN_POINT('Ctrl Pts',(2.28686716492283,0.632128870352567,3.39355446507987));
#90149=CARTESIAN_POINT('Ctrl Pts',(2.35423213896257,0.359833805519979,3.37381027869488));
#90150=CARTESIAN_POINT('Ctrl Pts',(2.37721148295844,0.143977061040169,3.35774185953928));
#90151=CARTESIAN_POINT('Ctrl Pts',(2.36935363813576,-0.114942583988793,
3.33913191624066));
#90152=CARTESIAN_POINT('Ctrl Pts',(2.36687917453508,-0.157898383368767,
3.33607131716526));
#90153=CARTESIAN_POINT('Ctrl Pts',(2.36102481389732,-0.226810794523148,
3.3312273486414));
#90154=CARTESIAN_POINT('Ctrl Pts',(2.35838165075067,-0.252818990104549,
3.32941441903419));
#90155=CARTESIAN_POINT('Ctrl Pts',(2.35431242776139,-0.287198408725764,
3.32704271485801));
#90156=CARTESIAN_POINT('Ctrl Pts',(2.35327079589853,-0.295612077256806,
3.3264642585685));
#90157=CARTESIAN_POINT('Ctrl Pts',(2.35148382452944,-0.309437758480717,
3.32551715608932));
#90158=CARTESIAN_POINT('Ctrl Pts',(2.35076487259093,-0.314853011332579,
3.32514706354511));
#90159=CARTESIAN_POINT('Ctrl Pts',(2.34932004066704,-0.3254548124308,3.32442427578435));
#90160=CARTESIAN_POINT('Ctrl Pts',(2.34859568372984,-0.330641503205517,
3.32407150190324));
#90161=CARTESIAN_POINT('Ctrl Pts',(2.34676963400772,-0.343407938821845,
3.32320515132843));
#90162=CARTESIAN_POINT('Ctrl Pts',(2.34564837960225,-0.350984915519029,
3.32269266936383));
#90163=CARTESIAN_POINT('Ctrl Pts',(2.34167050153528,-0.376995036843662,
3.32093887204118));
#90164=CARTESIAN_POINT('Ctrl Pts',(2.33863305326271,-0.395400419141881,
3.31970724499628));
#90165=CARTESIAN_POINT('Ctrl Pts',(2.30924274821025,-0.561284117958674,
3.30867620028092));
#90166=CARTESIAN_POINT('Ctrl Pts',(2.26918470437125,-0.706014158090181,
3.29953470311035));
#90167=CARTESIAN_POINT('Ctrl Pts',(2.17251748492362,-0.959188039062189,
3.28293068048594));
#90168=CARTESIAN_POINT('Ctrl Pts',(2.12070087630864,-1.06887728099209,3.27550706518723));
#90169=CARTESIAN_POINT('Ctrl Pts',(2.04004690504821,-1.21043511997938,3.26518619782473));
#90170=CARTESIAN_POINT('Ctrl Pts',(2.01840334388994,-1.24619106956255,3.26251221719427));
#90171=CARTESIAN_POINT('Ctrl Pts',(1.97957029422061,-1.30667708803672,3.25785676284712));
#90172=CARTESIAN_POINT('Ctrl Pts',(1.9628333342493,-1.33168642331388,3.25589142400215));
#90173=CARTESIAN_POINT('Ctrl Pts',(1.93831935632939,-1.36685015952646,3.25306623588185));
#90174=CARTESIAN_POINT('Ctrl Pts',(1.93092857231915,-1.37727125996728,3.25222103930754));
#90175=CARTESIAN_POINT('Ctrl Pts',(1.91799974163037,-1.39519244699974,3.25075349610613));
#90176=CARTESIAN_POINT('Ctrl Pts',(1.91250094725718,-1.40272060494509,3.25013267256989));
#90177=CARTESIAN_POINT('Ctrl Pts',(1.90185650287572,-1.41711450440887,3.2489371565414));
#90178=CARTESIAN_POINT('Ctrl Pts',(1.89671769023006,-1.4239851390905,3.2483627373792));
#90179=CARTESIAN_POINT('Ctrl Pts',(1.88451959377135,-1.44011091689343,3.24700554836889));
#90180=CARTESIAN_POINT('Ctrl Pts',(1.87742928520924,-1.44934220350858,3.24622156446382));
#90181=CARTESIAN_POINT('Ctrl Pts',(1.85246456520938,-1.48135463892201,3.24347783010588));
#90182=CARTESIAN_POINT('Ctrl Pts',(1.83424176619718,-1.50385954963592,3.24150427973066));
#90183=CARTESIAN_POINT('Ctrl Pts',(1.7125492387606,-1.64864520560762,3.22850575714423));
#90184=CARTESIAN_POINT('Ctrl Pts',(1.59734837507036,-1.76048753739628,3.21698770460297));
#90185=CARTESIAN_POINT('Ctrl Pts',(1.38002655112039,-1.93246380846643,3.19676496389404));
#90186=CARTESIAN_POINT('Ctrl Pts',(1.28301869734184,-1.9981879664131,3.18817689086393));
#90187=CARTESIAN_POINT('Ctrl Pts',(1.15296112781332,-2.07291244164711,3.17748587302104));
#90188=CARTESIAN_POINT('Ctrl Pts',(1.12402906074737,-2.08874226728799,3.17515704205183));
#90189=CARTESIAN_POINT('Ctrl Pts',(1.07566590984934,-2.11390750204913,3.17135580629137));
#90190=CARTESIAN_POINT('Ctrl Pts',(1.05642159343243,-2.12359025629358,3.16986665403269));
#90191=CARTESIAN_POINT('Ctrl Pts',(1.02996336632331,-2.13645397065153,3.16785367011867));
#90192=CARTESIAN_POINT('Ctrl Pts',(1.02286230506093,-2.13986280262467,3.16731675476663));
#90193=CARTESIAN_POINT('Ctrl Pts',(1.01092455167749,-2.14552046379537,3.16641989280561));
#90194=CARTESIAN_POINT('Ctrl Pts',(1.00609707233937,-2.14778844222199,3.16605878354222));
#90195=CARTESIAN_POINT('Ctrl Pts',(0.996930428107869,-2.15205729817039,
3.16537612223321));
#90196=CARTESIAN_POINT('Ctrl Pts',(0.992592813292142,-2.1540613735774,3.16505436859447));
#90197=CARTESIAN_POINT('Ctrl Pts',(0.98121133816629,-2.15927819162227,3.16421338766116));
#90198=CARTESIAN_POINT('Ctrl Pts',(0.974157677210408,-2.16246961207071,
3.1636954608976));
#90199=CARTESIAN_POINT('Ctrl Pts',(0.949604311915052,-2.1734342334525,3.16190349122837));
#90200=CARTESIAN_POINT('Ctrl Pts',(0.932025628427168,-2.18103026164378,
3.16063970951804));
#90201=CARTESIAN_POINT('Ctrl Pts',(0.800822280802883,-2.23584925648303,
3.15133464740293));
#90202=CARTESIAN_POINT('Ctrl Pts',(0.683752834467941,-2.27438529626563,
3.14373194742638));
#90203=CARTESIAN_POINT('Ctrl Pts',(0.463161426831023,-2.3284119710937,3.12979157711026));
#90204=CARTESIAN_POINT('Ctrl Pts',(0.360597779832508,-2.34648446148754,
3.12345509000767));
#90205=CARTESIAN_POINT('Ctrl Pts',(0.164582677678252,-2.36786555890214,
3.1111921124064));
#90206=CARTESIAN_POINT('Ctrl Pts',(0.071478311598831,-2.37250133709471,
3.10530347247293));
#90207=CARTESIAN_POINT('Ctrl Pts',(-0.0461983933535427,-2.37142708612143,
3.0976457388164));
#90208=CARTESIAN_POINT('Ctrl Pts',(-0.070740632490637,-2.37082188393347,
3.09603715276356));
#90209=CARTESIAN_POINT('Ctrl Pts',(-0.107036589293985,-2.36936277233319,
3.0936392259401));
#90210=CARTESIAN_POINT('Ctrl Pts',(-0.118800982850021,-2.36880203823712,
3.09285905303097));
#90211=CARTESIAN_POINT('Ctrl Pts',(-0.139717212163434,-2.36764888923943,
3.09146650648274));
#90212=CARTESIAN_POINT('Ctrl Pts',(-0.148870772264499,-2.36709096808548,
3.09085522654525));
#90213=CARTESIAN_POINT('Ctrl Pts',(-0.168142499546943,-2.36580410618132,
3.08956422448299));
#90214=CARTESIAN_POINT('Ctrl Pts',(-0.178259662493634,-2.36506330912125,
3.08888414184679));
#90215=CARTESIAN_POINT('Ctrl Pts',(-0.205032001228322,-2.36293022983492,
3.08707813150628));
#90216=CARTESIAN_POINT('Ctrl Pts',(-0.221677495004204,-2.36142678391804,
3.08594873585244));
#90217=CARTESIAN_POINT('Ctrl Pts',(-0.29381504072408,-2.3541417832623,3.081024943442));
#90218=CARTESIAN_POINT('Ctrl Pts',(-0.349105209863459,-2.3465795229204,
3.07717523007461));
#90219=CARTESIAN_POINT('Ctrl Pts',(-0.626428686081089,-2.29863110387524,
3.05746655688346));
#90220=CARTESIAN_POINT('Ctrl Pts',(-0.842145272190765,-2.22864907360465,
3.04068218685984));
#90221=CARTESIAN_POINT('Ctrl Pts',(-1.10283636837371,-2.10074944757143,
3.01981333034785));
#90222=CARTESIAN_POINT('Ctrl Pts',(-1.15981875370415,-2.06983538036067,
3.01522376274076));
#90223=CARTESIAN_POINT('Ctrl Pts',(-1.22513166740634,-2.03085624505323,
3.00998786710767));
#90224=CARTESIAN_POINT('Ctrl Pts',(-1.23475362993853,-2.02502053732562,
3.00921717592305));
#90225=CARTESIAN_POINT('Ctrl Pts',(-1.249503371715,-2.0159306186073,3.00803722566984));
#90226=CARTESIAN_POINT('Ctrl Pts',(-1.25466063264682,-2.0127249275449,3.00762493256777));
#90227=CARTESIAN_POINT('Ctrl Pts',(-1.26413655749831,-2.00678423253315,
3.00686798184273));
#90228=CARTESIAN_POINT('Ctrl Pts',(-1.2684586720845,-2.00405508660435,3.00652296308584));
#90229=CARTESIAN_POINT('Ctrl Pts',(-1.27819918946859,-1.99786042078286,
3.00574592554362));
#90230=CARTESIAN_POINT('Ctrl Pts',(-1.283612331824,-1.99438682630894,3.00531444876674));
#90231=CARTESIAN_POINT('Ctrl Pts',(-1.29956699145617,-1.98405691101932,
3.00404354235361));
#90232=CARTESIAN_POINT('Ctrl Pts',(-1.31006839351826,-1.97713859226048,
3.0032080985197));
#90233=CARTESIAN_POINT('Ctrl Pts',(-1.40208920424571,-1.91546022824193,
2.99589211255175));
#90234=CARTESIAN_POINT('Ctrl Pts',(-1.48020063201021,-1.85576218044727,
2.9897135449707));
#90235=CARTESIAN_POINT('Ctrl Pts',(-1.63708275543549,-1.71963472855321,
2.97685381711691));
#90236=CARTESIAN_POINT('Ctrl Pts',(-1.71470560885042,-1.64224512723675,
2.97020875888437));
#90237=CARTESIAN_POINT('Ctrl Pts',(-1.84376628626021,-1.49440692543913,
2.95811091692015));
#90238=CARTESIAN_POINT('Ctrl Pts',(-1.89719264454364,-1.42596785963892,
2.95270740581405));
#90239=CARTESIAN_POINT('Ctrl Pts',(-1.97599425139401,-1.31273245209263,
2.94390474504922));
#90240=CARTESIAN_POINT('Ctrl Pts',(-2.0038710099289,-1.26977168280228,2.94059479357627));
#90241=CARTESIAN_POINT('Ctrl Pts',(-2.03840440031615,-1.21257961467826,
2.93620795143912));
#90242=CARTESIAN_POINT('Ctrl Pts',(-2.04634222440281,-1.19913523102338,
2.93517812215102));
#90243=CARTESIAN_POINT('Ctrl Pts',(-2.05909681324737,-1.17703714413883,
2.93348721633614));
#90244=CARTESIAN_POINT('Ctrl Pts',(-2.0639932201703,-1.16842976126621,2.93282903407027));
#90245=CARTESIAN_POINT('Ctrl Pts',(-2.07335558941737,-1.15172917984353,
2.93155270441238));
#90246=CARTESIAN_POINT('Ctrl Pts',(-2.07782843087107,-1.14364002708499,
2.9309348187649));
#90247=CARTESIAN_POINT('Ctrl Pts',(-2.08804154648656,-1.12491186313096,
2.92950490658579));
#90248=CARTESIAN_POINT('Ctrl Pts',(-2.0937479524662,-1.11425477417677,2.92869169213439));
#90249=CARTESIAN_POINT('Ctrl Pts',(-2.11189784904858,-1.07972690279284,
2.92605815058622));
#90250=CARTESIAN_POINT('Ctrl Pts',(-2.12401610371344,-1.05568849394934,
2.9242264636216));
#90251=CARTESIAN_POINT('Ctrl Pts',(-2.22441002246677,-0.847812645576312,
2.90839568709296));
#90252=CARTESIAN_POINT('Ctrl Pts',(-2.28902577512322,-0.653538321798643,
2.89354965260473));
#90253=CARTESIAN_POINT('Ctrl Pts',(-2.35073967197113,-0.33670268620984,
2.86998697049575));
#90254=CARTESIAN_POINT('Ctrl Pts',(-2.36466843310237,-0.21839321420602,
2.86135210729747));
#90255=CARTESIAN_POINT('Ctrl Pts',(-2.37030206316532,-0.0842595329870371,
2.85205830356647));
#90256=CARTESIAN_POINT('Ctrl Pts',(-2.37079573292328,-0.0689866878830017,
2.85100743750445));
#90257=CARTESIAN_POINT('Ctrl Pts',(-2.37129733476559,-0.046842264251883,
2.84949543001245));
#90258=CARTESIAN_POINT('Ctrl Pts',(-2.37142305786338,-0.0399741320860062,
2.84902810423781));
#90259=CARTESIAN_POINT('Ctrl Pts',(-2.37159088964592,-0.027951448455367,
2.84821300782077));
#90260=CARTESIAN_POINT('Ctrl Pts',(-2.37164603641732,-0.02279717871641,
2.84786452135961));
#90261=CARTESIAN_POINT('Ctrl Pts',(-2.37172741255881,-0.0118578461686369,
2.84712695927788));
#90262=CARTESIAN_POINT('Ctrl Pts',(-2.37174928065598,-0.00607285206230565,
2.8467381283931));
#90263=CARTESIAN_POINT('Ctrl Pts',(-2.3717511875859,0.00964443574313672,
2.84568485882211));
#90264=CARTESIAN_POINT('Ctrl Pts',(-2.37169000297992,0.0195767578266909,
2.84502267455331));
#90265=CARTESIAN_POINT('Ctrl Pts',(-2.37105122836884,0.070914175783284,
2.84161631971275));
#90266=CARTESIAN_POINT('Ctrl Pts',(-2.36945172122315,0.112302292666018,
2.83892488329156));
#90267=CARTESIAN_POINT('Ctrl Pts',(-2.36634812415,0.160115107416461,2.83585712621301));
#90268=CARTESIAN_POINT('Ctrl Pts',(-2.36590059103696,0.166597310392362,
2.83544210089004));
#90269=CARTESIAN_POINT('Ctrl Pts',(-2.36542649402054,0.173076757208175,
2.83502806412758));
#90270=CARTESIAN_POINT('',(-2.36993516591118,-0.00198226883289276,2.65141112235218));
#90271=CARTESIAN_POINT('Ctrl Pts',(-2.36542650247982,0.173076641595803,
2.63790316127816));
#90272=CARTESIAN_POINT('Ctrl Pts',(-2.36968965435484,0.114812439469591,
2.6420032035342));
#90273=CARTESIAN_POINT('Ctrl Pts',(-2.371799477955,0.0563994550688975,2.64616284491173));
#90274=CARTESIAN_POINT('Ctrl Pts',(-2.37174911952633,-0.00204365507856347,
2.65036731141953));
#90275=CARTESIAN_POINT('Ctrl Pts',(-2.36993516591118,-0.00198226883289275,
2.65141112235218));
#90276=CARTESIAN_POINT('Ctrl Pts',(-2.37186914624274,-0.249525648545458,
2.66799504931007));
#90277=CARTESIAN_POINT('Ctrl Pts',(-2.22218144459194,-1.28536352789007,
2.73754295476256));
#90278=CARTESIAN_POINT('Ctrl Pts',(-0.720433887694406,-2.70989311549094,
2.86005483870968));
#90279=CARTESIAN_POINT('Ctrl Pts',(1.88762043170213,-2.07350795749998,3.01894677419355));
#90280=CARTESIAN_POINT('Ctrl Pts',(2.76545213444046,0.463487386787571,3.17783870967742));
#90281=CARTESIAN_POINT('Ctrl Pts',(1.10842681518721,2.57564282834349,3.33673064516129));
#90282=CARTESIAN_POINT('Ctrl Pts',(-1.48151917809488,2.33465397998857,3.49068403291595));
#90283=CARTESIAN_POINT('Ctrl Pts',(-2.31143607334521,0.884136787947507,
3.59167344217597));
#90284=CARTESIAN_POINT('Ctrl Pts',(-2.36847158556395,0.173320321679478,
3.63969887294137));
#90285=CARTESIAN_POINT('Origin',(0.,0.,-1.84858989190503));
#90286=CARTESIAN_POINT('',(-2.36152614656945,0.172792042906829,4.83696616984731));
#90287=CARTESIAN_POINT('',(-2.36542650810962,0.173076564653691,4.64035944112689));
#90288=CARTESIAN_POINT('',(-2.36542649454111,0.173076750093529,-1.84858989190503));
#90289=CARTESIAN_POINT('',(-2.37061499902234,0.00211578448275317,3.84858989190501));
#90290=CARTESIAN_POINT('Ctrl Pts',(-2.37061499902234,0.00211578448275317,
3.84858989190501));
#90291=CARTESIAN_POINT('Ctrl Pts',(-2.36573802108978,-0.565818237034438,
3.88666572659761));
#90292=CARTESIAN_POINT('Ctrl Pts',(-1.87624458737536,-1.93166428036642,
3.97772985001846));
#90293=CARTESIAN_POINT('Ctrl Pts',(0.40722627036569,-2.77473424763259,4.12178226216756));
#90294=CARTESIAN_POINT('Ctrl Pts',(2.55350060517878,-1.1595766637486,4.2807471283523));
#90295=CARTESIAN_POINT('Ctrl Pts',(2.35722861767805,1.51936059698208,4.43971199453706));
#90296=CARTESIAN_POINT('Ctrl Pts',(-0.00153247116466099,2.80445735060936,
4.5986768607218));
#90297=CARTESIAN_POINT('Ctrl Pts',(-1.96521418831998,1.73182241497003,4.73109491915855));
#90298=CARTESIAN_POINT('Ctrl Pts',(-2.33268167915334,0.567299710385224,
4.81052468886706));
#90299=CARTESIAN_POINT('Ctrl Pts',(-2.36152614656945,0.172792042906829,
4.83696616984731));
#90300=CARTESIAN_POINT('Ctrl Pts',(-2.37174901274681,0.00216403200924694,
3.8492415291672));
#90301=CARTESIAN_POINT('Ctrl Pts',(-2.37169694361488,0.0592310771005431,
3.84510489340989));
#90302=CARTESIAN_POINT('Ctrl Pts',(-2.36958528398647,0.116239040395148,
3.84094193242637));
#90303=CARTESIAN_POINT('Ctrl Pts',(-2.36542646296204,0.1730771816818,3.83677864400945));
#90304=CARTESIAN_POINT('',(-2.37532752442066,-0.000269425568870816,3.65157275994242));
#90305=CARTESIAN_POINT('Ctrl Pts',(-2.36847158556395,0.173320321679478,
3.63969887294137));
#90306=CARTESIAN_POINT('Ctrl Pts',(-2.37310753894245,0.115543826473337,
3.64360247000484));
#90307=CARTESIAN_POINT('Ctrl Pts',(-2.37551285241125,0.0576284297436606,
3.64750606706831));
#90308=CARTESIAN_POINT('Ctrl Pts',(-2.37561175167707,-0.000280201698186815,
3.65140966413178));
#90309=CARTESIAN_POINT('Ctrl Pts',(-2.37174999622658,-0.000133787956428912,
3.65362562379593));
#90310=CARTESIAN_POINT('Ctrl Pts',(-2.37174970721966,-0.00525720993116726,
3.65397696200977));
#90311=CARTESIAN_POINT('Ctrl Pts',(-2.37173281688968,-0.0103806823582881,
3.65432745743365));
#90312=CARTESIAN_POINT('Ctrl Pts',(-2.37165813786147,-0.0218044944275061,
3.65510701147203));
#90313=CARTESIAN_POINT('Ctrl Pts',(-2.37159184582707,-0.0281047681602935,
3.65553561857383));
#90314=CARTESIAN_POINT('Ctrl Pts',(-2.37142817895413,-0.0393862208450815,
3.65630064254654));
#90315=CARTESIAN_POINT('Ctrl Pts',(-2.37134021411968,-0.0443674787193265,
3.65663757609617));
#90316=CARTESIAN_POINT('Ctrl Pts',(-2.37113220301038,-0.0543625767235476,
3.65731188805149));
#90317=CARTESIAN_POINT('Ctrl Pts',(-2.37101195003731,-0.0593763242050389,
3.6576492561793));
#90318=CARTESIAN_POINT('Ctrl Pts',(-2.37063889617656,-0.0731124373295902,
3.65857121978151));
#90319=CARTESIAN_POINT('Ctrl Pts',(-2.37035385828226,-0.0818339603874946,
3.65915404171882));
#90320=CARTESIAN_POINT('Ctrl Pts',(-2.36905857400245,-0.115734776685101,
3.66141021118516));
#90321=CARTESIAN_POINT('Ctrl Pts',(-2.36769516245422,-0.140899999641985,
3.66306510932193));
#90322=CARTESIAN_POINT('Ctrl Pts',(-2.3554783169029,-0.314979866878836,
3.67440461141037));
#90323=CARTESIAN_POINT('Ctrl Pts',(-2.33098360872185,-0.462620410842606,
3.68348708673121));
#90324=CARTESIAN_POINT('Ctrl Pts',(-2.26534192715558,-0.710565442903368,
3.69920747378263));
#90325=CARTESIAN_POINT('Ctrl Pts',(-2.23093644588801,-0.812156119878761,
3.70579008512994));
#90326=CARTESIAN_POINT('Ctrl Pts',(-2.16373862707967,-0.973668583495306,
3.71684337424294));
#90327=CARTESIAN_POINT('Ctrl Pts',(-2.1350228904034,-1.03511895541834,3.72119531228255));
#90328=CARTESIAN_POINT('Ctrl Pts',(-2.09573142586352,-1.11058851939073,
3.72677172255028));
#90329=CARTESIAN_POINT('Ctrl Pts',(-2.08757893011206,-1.12583802252723,
3.72791068993445));
#90330=CARTESIAN_POINT('Ctrl Pts',(-2.07427427723968,-1.15008335178748,
3.72974181874075));
#90331=CARTESIAN_POINT('Ctrl Pts',(-2.06922851821134,-1.15913710443726,
3.73043018412476));
#90332=CARTESIAN_POINT('Ctrl Pts',(-2.05954863937798,-1.17624136389318,
3.73173950145989));
#90333=CARTESIAN_POINT('Ctrl Pts',(-2.05492624086863,-1.1842983088943,3.73236002262995));
#90334=CARTESIAN_POINT('Ctrl Pts',(-2.0443148118103,-1.20254509765448,3.73377403941285));
#90335=CARTESIAN_POINT('Ctrl Pts',(-2.03829673734783,-1.21271767670587,
3.73456857763485));
#90336=CARTESIAN_POINT('Ctrl Pts',(-2.02250023213568,-1.23896933817815,
3.73663542108274));
#90337=CARTESIAN_POINT('Ctrl Pts',(-2.01260617453459,-1.25497751394195,
3.73791192567507));
#90338=CARTESIAN_POINT('Ctrl Pts',(-1.91658393600196,-1.40628123413224,
3.75013453113387));
#90339=CARTESIAN_POINT('Ctrl Pts',(-1.8171485330118,-1.53260343623574,3.76159306645173));
#90340=CARTESIAN_POINT('Ctrl Pts',(-1.65596131908237,-1.69944869451329,
3.77849059041007));
#90341=CARTESIAN_POINT('Ctrl Pts',(-1.60385871365316,-1.74870550438995,
3.78373875413573));
#90342=CARTESIAN_POINT('Ctrl Pts',(-1.47383411763604,-1.86092149620778,
3.79624160657363));
#90343=CARTESIAN_POINT('Ctrl Pts',(-1.39398922261316,-1.92146157633635,
3.80345633987108));
#90344=CARTESIAN_POINT('Ctrl Pts',(-1.30175906154513,-1.98260753120884,
3.81111537666522));
#90345=CARTESIAN_POINT('Ctrl Pts',(-1.29293046844369,-1.98837624479221,
3.81184199963821));
#90346=CARTESIAN_POINT('Ctrl Pts',(-1.27847826439515,-1.99768253729463,
3.81302050070138));
#90347=CARTESIAN_POINT('Ctrl Pts',(-1.27287786345306,-2.00125564077075,
3.81347452637887));
#90348=CARTESIAN_POINT('Ctrl Pts',(-1.26209889716921,-2.00806916010153,
3.8143431808272));
#90349=CARTESIAN_POINT('Ctrl Pts',(-1.25692268889739,-2.01131318651841,
3.81475803685688));
#90350=CARTESIAN_POINT('Ctrl Pts',(-1.24741519546511,-2.01722067335192,
3.81551577334873));
#90351=CARTESIAN_POINT('Ctrl Pts',(-1.24308788368918,-2.01989020232532,
3.81585904124444));
#90352=CARTESIAN_POINT('Ctrl Pts',(-1.23330739220442,-2.0258804754581,3.81663127023021));
#90353=CARTESIAN_POINT('Ctrl Pts',(-1.22784937818766,-2.02919312324305,
3.81705970142194));
#90354=CARTESIAN_POINT('Ctrl Pts',(-1.21221740224743,-2.03859451853526,
3.81827978580032));
#90355=CARTESIAN_POINT('Ctrl Pts',(-1.20201088927664,-2.04462917857802,
3.81906802919313));
#90356=CARTESIAN_POINT('Ctrl Pts',(-1.13319605022371,-2.08462295384708,
3.82432955625535));
#90357=CARTESIAN_POINT('Ctrl Pts',(-1.0731952255722,-2.11613801691913,3.82866089188509));
#90358=CARTESIAN_POINT('Ctrl Pts',(-0.87749173029746,-2.20846085825506,
3.84225084888042));
#90359=CARTESIAN_POINT('Ctrl Pts',(-0.737392594625412,-2.25910336498024,
3.85120452778059));
#90360=CARTESIAN_POINT('Ctrl Pts',(-0.486138510151893,-2.32403884228448,
3.86723646039136));
#90361=CARTESIAN_POINT('Ctrl Pts',(-0.377008688596753,-2.34421567352434,
3.87418864379667));
#90362=CARTESIAN_POINT('Ctrl Pts',(-0.240053621195826,-2.3597247765954,
3.88313845344956));
#90363=CARTESIAN_POINT('Ctrl Pts',(-0.213181660280136,-2.36230401188295,
3.88490461927424));
#90364=CARTESIAN_POINT('Ctrl Pts',(-0.173972016574562,-2.36539299873769,
3.88749897039356));
#90365=CARTESIAN_POINT('Ctrl Pts',(-0.161664457301236,-2.36626602362212,
3.88831578416466));
#90366=CARTESIAN_POINT('Ctrl Pts',(-0.140012976307824,-2.3676321445277,
3.88975730960645));
#90367=CARTESIAN_POINT('Ctrl Pts',(-0.130671824713955,-2.36816605736437,
3.89038072895759));
#90368=CARTESIAN_POINT('Ctrl Pts',(-0.111235292656852,-2.36916164488277,
3.89168113167471));
#90369=CARTESIAN_POINT('Ctrl Pts',(-0.101139650100711,-2.36961409423794,
3.89235839118452));
#90370=CARTESIAN_POINT('Ctrl Pts',(-0.0749404867581275,-2.37062051222863,
3.89412079326294));
#90371=CARTESIAN_POINT('Ctrl Pts',(-0.0588338876249706,-2.37107491253462,
3.89520902722751));
#90372=CARTESIAN_POINT('Ctrl Pts',(0.00656013330813427,-2.37225309905478,
3.89964742863056));
#90373=CARTESIAN_POINT('Ctrl Pts',(0.0558567489632089,-2.37160435045954,
3.90303993479772));
#90374=CARTESIAN_POINT('Ctrl Pts',(0.313039499773506,-2.3601971519408,3.92099558090533));
#90375=CARTESIAN_POINT('Ctrl Pts',(0.518842729267534,-2.32363885097875,
3.9363542566605));
#90376=CARTESIAN_POINT('Ctrl Pts',(0.774593047005348,-2.24250562374867,
3.9558100149284));
#90377=CARTESIAN_POINT('Ctrl Pts',(0.83129421337533,-2.22211089278136,3.96013938341992));
#90378=CARTESIAN_POINT('Ctrl Pts',(0.907677217471089,-2.19130315578729,
3.96594300835406));
#90379=CARTESIAN_POINT('Ctrl Pts',(0.928077527837284,-2.18274131177302,
3.96749011255936));
#90380=CARTESIAN_POINT('Ctrl Pts',(0.962990958682624,-2.16751042073987,
3.9701292799859));
#90381=CARTESIAN_POINT('Ctrl Pts',(0.97756171174331,-2.16097805291686,3.97122809751967));
#90382=CARTESIAN_POINT('Ctrl Pts',(0.998471007213169,-2.15134921296674,
3.97279999535397));
#90383=CARTESIAN_POINT('Ctrl Pts',(1.00486306061145,-2.14837101568828,3.97327986106315));
#90384=CARTESIAN_POINT('Ctrl Pts',(1.01598218928636,-2.14312988805785,3.97411330804923));
#90385=CARTESIAN_POINT('Ctrl Pts',(1.02071517915136,-2.14087973770407,3.97446766159697));
#90386=CARTESIAN_POINT('Ctrl Pts',(1.03069868576416,-2.13609276083518,3.97521420372924));
#90387=CARTESIAN_POINT('Ctrl Pts',(1.03594732396635,-2.13355225095705,3.97560616081146));
#90388=CARTESIAN_POINT('Ctrl Pts',(1.0500889258642,-2.12664277219426,3.97666095431636));
#90389=CARTESIAN_POINT('Ctrl Pts',(1.05896409323906,-2.12223733136424,3.97732157308264));
#90390=CARTESIAN_POINT('Ctrl Pts',(1.09924754701406,-2.10192586663983,3.9803150210401));
#90391=CARTESIAN_POINT('Ctrl Pts',(1.13032876996793,-2.08537639662299,3.98261067152649));
#90392=CARTESIAN_POINT('Ctrl Pts',(1.3763727253247,-1.94724991389,4.00076351122985));
#90393=CARTESIAN_POINT('Ctrl Pts',(1.57153143205635,-1.79346176049961,4.01518883974709));
#90394=CARTESIAN_POINT('Ctrl Pts',(1.78407782115422,-1.56415271190667,4.03496813084));
#90395=CARTESIAN_POINT('Ctrl Pts',(1.82668133820411,-1.51418011505167,4.0391853151012));
#90396=CARTESIAN_POINT('Ctrl Pts',(1.87770989534227,-1.44903299048138,4.04460994046612));
#90397=CARTESIAN_POINT('Ctrl Pts',(1.88811852017685,-1.4354440033568,4.04573756855323));
#90398=CARTESIAN_POINT('Ctrl Pts',(1.9045691203276,-1.41347839193573,4.04755476162712));
#90399=CARTESIAN_POINT('Ctrl Pts',(1.91070518600005,-1.40517272426412,4.04824063335782));
#90400=CARTESIAN_POINT('Ctrl Pts',(1.92226184314132,-1.38931418102175,4.04954799872266));
#90401=CARTESIAN_POINT('Ctrl Pts',(1.92769266202909,-1.38176896900196,4.05016908013848));
#90402=CARTESIAN_POINT('Ctrl Pts',(1.93996643793719,-1.36450342282666,4.05158826890566));
#90403=CARTESIAN_POINT('Ctrl Pts',(1.94678091135795,-1.35476324331788,4.05238744777883));
#90404=CARTESIAN_POINT('Ctrl Pts',(1.96432171480763,-1.32928588676958,4.05447436016386));
#90405=CARTESIAN_POINT('Ctrl Pts',(1.97493204283517,-1.31347027269504,4.05576642902));
#90406=CARTESIAN_POINT('Ctrl Pts',(2.06418426941142,-1.17690534560364,4.06689653573882));
#90407=CARTESIAN_POINT('Ctrl Pts',(2.13184646092771,-1.04937106700619,4.07714202908675));
#90408=CARTESIAN_POINT('Ctrl Pts',(2.22531539093317,-0.826280684265977,
4.09470715444235));
#90409=CARTESIAN_POINT('Ctrl Pts',(2.25749946991448,-0.733801162490264,
4.10188676800893));
#90410=CARTESIAN_POINT('Ctrl Pts',(2.30707275097781,-0.556784957029317,
4.11523832822761));
#90411=CARTESIAN_POINT('Ctrl Pts',(2.3257459865696,-0.472760990867566,4.12141632063393));
#90412=CARTESIAN_POINT('Ctrl Pts',(2.34271409477077,-0.37040932640452,4.12861986573909));
#90413=CARTESIAN_POINT('Ctrl Pts',(2.34541765901632,-0.352885889433598,
4.12984185161993));
#90414=CARTESIAN_POINT('Ctrl Pts',(2.34896453195006,-0.328051510826,4.13155613976685));
#90415=CARTESIAN_POINT('Ctrl Pts',(2.34997064001308,-0.320764962033692,
4.13205699365888));
#90416=CARTESIAN_POINT('Ctrl Pts',(2.35164185178808,-0.30823146073051,4.13291471475521));
#90417=CARTESIAN_POINT('Ctrl Pts',(2.35232332882057,-0.302986784280395,
4.13327248919099));
#90418=CARTESIAN_POINT('Ctrl Pts',(2.35370250739067,-0.292087367266539,
4.13401359199907));
#90419=CARTESIAN_POINT('Ctrl Pts',(2.35439738158168,-0.28643235634986,4.13439676152469));
#90420=CARTESIAN_POINT('Ctrl Pts',(2.35617359165118,-0.271533932111144,
4.13540284167518));
#90421=CARTESIAN_POINT('Ctrl Pts',(2.35722092668861,-0.262286447004037,
4.13602387464888));
#90422=CARTESIAN_POINT('Ctrl Pts',(2.36138660080207,-0.223463225092625,
4.13861759530537));
#90423=CARTESIAN_POINT('Ctrl Pts',(2.36400311925361,-0.19383484212269,4.14056412220954));
#90424=CARTESIAN_POINT('Ctrl Pts',(2.37727587942528,-0.00253661920322199,
4.15296567751372));
#90425=CARTESIAN_POINT('Ctrl Pts',(2.37190077141875,0.159834311433769,4.16274909999971));
#90426=CARTESIAN_POINT('Ctrl Pts',(2.3299939034092,0.467199987332939,4.18179507010532));
#90427=CARTESIAN_POINT('Ctrl Pts',(2.29627290561349,0.611775510969299,4.19099229690927));
#90428=CARTESIAN_POINT('Ctrl Pts',(2.24227577712706,0.773231415345579,4.20209525420844));
#90429=CARTESIAN_POINT('Ctrl Pts',(2.23496604832748,0.794112202902458,4.20354716516677));
#90430=CARTESIAN_POINT('Ctrl Pts',(2.22345016727089,0.825589048674656,4.20576159249658));
#90431=CARTESIAN_POINT('Ctrl Pts',(2.21945781941435,0.836262461060113,4.2065170052569));
#90432=CARTESIAN_POINT('Ctrl Pts',(2.2120854129001,0.855547643021267,4.20789033620728));
#90433=CARTESIAN_POINT('Ctrl Pts',(2.20873157129023,0.864169245725234,4.20850736584027));
#90434=CARTESIAN_POINT('Ctrl Pts',(2.2014104586864,0.882668316094854,4.20983803203578));
#90435=CARTESIAN_POINT('Ctrl Pts',(2.19742697308093,0.892539105816755,4.21055220421699));
#90436=CARTESIAN_POINT('Ctrl Pts',(2.18649446015358,0.919112229826322,4.21248624441324));
#90437=CARTESIAN_POINT('Ctrl Pts',(2.17942068038512,0.935762139399023,4.21371031221542));
#90438=CARTESIAN_POINT('Ctrl Pts',(2.14352697951076,1.01763169874518,4.21979136196593));
#90439=CARTESIAN_POINT('Ctrl Pts',(2.1119693588624,1.08160332434039,4.22474105442175));
#90440=CARTESIAN_POINT('Ctrl Pts',(1.98659147178823,1.30928787170186,4.24310617993216));
#90441=CARTESIAN_POINT('Ctrl Pts',(1.87621844088715,1.46306805842334,4.25704940759086));
#90442=CARTESIAN_POINT('Ctrl Pts',(1.6983172782291,1.65725898757842,4.27610689809782));
#90443=CARTESIAN_POINT('Ctrl Pts',(1.6452239886398,1.70997931759794,4.28145071638405));
#90444=CARTESIAN_POINT('Ctrl Pts',(1.57745429425221,1.77118867700159,4.28778227455734));
#90445=CARTESIAN_POINT('Ctrl Pts',(1.56506947489374,1.7821416771336,4.28892056505657));
#90446=CARTESIAN_POINT('Ctrl Pts',(1.54716442525568,1.79764608512422,4.29053828484874));
#90447=CARTESIAN_POINT('Ctrl Pts',(1.54173690806009,1.80230311431043,4.29102504503779));
#90448=CARTESIAN_POINT('Ctrl Pts',(1.53228447625674,1.81033973752036,4.29186640057855));
#90449=CARTESIAN_POINT('Ctrl Pts',(1.52826927262454,1.81373060680081,4.29222181245014));
#90450=CARTESIAN_POINT('Ctrl Pts',(1.51981173577431,1.82082503246241,4.29296625663399));
#90451=CARTESIAN_POINT('Ctrl Pts',(1.51536710822465,1.82452570279928,4.29335508263167));
#90452=CARTESIAN_POINT('Ctrl Pts',(1.50343691370139,1.83438531200724,4.29439250841883));
#90453=CARTESIAN_POINT('Ctrl Pts',(1.49592695059528,1.84051476304724,4.29503901437206));
#90454=CARTESIAN_POINT('Ctrl Pts',(1.46256386823337,1.86740579342634,4.29788341417074));
#90455=CARTESIAN_POINT('Ctrl Pts',(1.43631315030701,1.88767112475779,4.30004847965507));
#90456=CARTESIAN_POINT('Ctrl Pts',(1.21022240811456,2.05476288348075,4.31816976352286));
#90457=CARTESIAN_POINT('Ctrl Pts',(0.98890396331218,2.16997499662157,4.33264607965647));
#90458=CARTESIAN_POINT('Ctrl Pts',(0.690299094513248,2.27005713786344,4.352555097169));
#90459=CARTESIAN_POINT('Ctrl Pts',(0.626011687492244,2.2886197377138,4.35684998799354));
#90460=CARTESIAN_POINT('Ctrl Pts',(0.544300200113707,2.30851290578193,4.36236216618868));
#90461=CARTESIAN_POINT('Ctrl Pts',(0.527526746175417,2.31240352232557,4.36349638439595));
#90462=CARTESIAN_POINT('Ctrl Pts',(0.500606753032239,2.31833950035922,4.36532167646026));
#90463=CARTESIAN_POINT('Ctrl Pts',(0.490486390575309,2.32050172483876,4.3660089974678));
#90464=CARTESIAN_POINT('Ctrl Pts',(0.471252975983677,2.32447951917007,4.36731749144728));
#90465=CARTESIAN_POINT('Ctrl Pts',(0.462142748437205,2.32630790701498,4.36793824138728));
#90466=CARTESIAN_POINT('Ctrl Pts',(0.44139270999305,2.33034566155726,4.36935439581084));
#90467=CARTESIAN_POINT('Ctrl Pts',(0.429746691947089,2.33252142512537,4.37015085486697));
#90468=CARTESIAN_POINT('Ctrl Pts',(0.399468940107325,2.33794360536491,4.37222599795063));
#90469=CARTESIAN_POINT('Ctrl Pts',(0.380814115402512,2.3410545293295,4.37350893733382));
#90470=CARTESIAN_POINT('Ctrl Pts',(0.20820792657668,2.36772111865761,4.38542259099948));
#90471=CARTESIAN_POINT('Ctrl Pts',(0.0523537403355777,2.3762776780993,4.39653437377631));
#90472=CARTESIAN_POINT('Ctrl Pts',(-0.215849127161198,2.36459812494689,
4.41607365872699));
#90473=CARTESIAN_POINT('Ctrl Pts',(-0.328019740197203,2.35166300702794,
4.42436178304244));
#90474=CARTESIAN_POINT('Ctrl Pts',(-0.506807421998396,2.31800061285028,
4.43746241782096));
#90475=CARTESIAN_POINT('Ctrl Pts',(-0.57418470303871,2.30223686642559,4.44237116962679));
#90476=CARTESIAN_POINT('Ctrl Pts',(-0.651895147882249,2.28043065614961,
4.44792955360047));
#90477=CARTESIAN_POINT('Ctrl Pts',(-0.662984510624347,2.27723139220565,
4.44872022832433));
#90478=CARTESIAN_POINT('Ctrl Pts',(-0.679981547461973,2.2721930876725,4.44992779074919));
#90479=CARTESIAN_POINT('Ctrl Pts',(-0.685905921867381,2.27041172502435,
4.45034787880452));
#90480=CARTESIAN_POINT('Ctrl Pts',(-0.696782684413773,2.26709480073911,
4.45111755228678));
#90481=CARTESIAN_POINT('Ctrl Pts',(-0.70173699109438,2.26556618557821,4.45146752064036));
#90482=CARTESIAN_POINT('Ctrl Pts',(-0.712892019460722,2.26208428064445,
4.45225414322988));
#90483=CARTESIAN_POINT('Ctrl Pts',(-0.719089737897296,2.26012173910042,
4.45269025114568));
#90484=CARTESIAN_POINT('Ctrl Pts',(-0.73732221794135,2.25426573413145,4.45397064475268));
#90485=CARTESIAN_POINT('Ctrl Pts',(-0.749334228816196,2.25030137630539,
4.45481091742305));
#90486=CARTESIAN_POINT('Ctrl Pts',(-0.847354753326082,2.21707946262185,
4.46164523619786));
#90487=CARTESIAN_POINT('Ctrl Pts',(-0.931660081245402,2.18299453085569,
4.46738231061973));
#90488=CARTESIAN_POINT('Ctrl Pts',(-1.04143131933049,2.13109181013205,4.47492116658288));
#90489=CARTESIAN_POINT('Ctrl Pts',(-1.06879719188339,2.11749949828943,4.4768064350546));
#90490=CARTESIAN_POINT('Ctrl Pts',(-1.22661806832913,2.03527247854872,4.48775326911671));
#90491=CARTESIAN_POINT('Ctrl Pts',(-1.35070217210204,1.95512851108792,4.4966831924423));
#90492=CARTESIAN_POINT('Ctrl Pts',(-1.52363056909719,1.8190723751601,4.51055047610442));
#90493=CARTESIAN_POINT('Ctrl Pts',(-1.57861943795132,1.77156242950967,4.51520355521581));
#90494=CARTESIAN_POINT('Ctrl Pts',(-1.64415699757484,1.70946122985096,4.52111848714565));
#90495=CARTESIAN_POINT('Ctrl Pts',(-1.65683950576998,1.69717198690424,4.52228133551876));
#90496=CARTESIAN_POINT('Ctrl Pts',(-1.67680328580924,1.67739020976055,4.52414181436475));
#90497=CARTESIAN_POINT('Ctrl Pts',(-1.68417449882976,1.66998904985739,4.52483542853047));
#90498=CARTESIAN_POINT('Ctrl Pts',(-1.69799786760767,1.65592491537452,4.5261490029716));
#90499=CARTESIAN_POINT('Ctrl Pts',(-1.70446031702403,1.64927229626655,4.52676849402255));
#90500=CARTESIAN_POINT('Ctrl Pts',(-1.71897606798874,1.63415295459913,4.52817234722268));
#90501=CARTESIAN_POINT('Ctrl Pts',(-1.72700610338463,1.62566432934718,4.52895769479941));
#90502=CARTESIAN_POINT('Ctrl Pts',(-1.74750055129954,1.60367623792859,4.53098496474995));
#90503=CARTESIAN_POINT('Ctrl Pts',(-1.75987121619112,1.59009085341708,4.53223082426789));
#90504=CARTESIAN_POINT('Ctrl Pts',(-1.8444552732108,1.49500495954231,4.54090670219134));
#90505=CARTESIAN_POINT('Ctrl Pts',(-1.91112838304458,1.40877147700662,4.54856291767247));
#90506=CARTESIAN_POINT('Ctrl Pts',(-2.05758873578597,1.189722786498,4.56749876885224));
#90507=CARTESIAN_POINT('Ctrl Pts',(-2.13075707555524,1.0530819957587,4.57891935235387));
#90508=CARTESIAN_POINT('Ctrl Pts',(-2.21881323658195,0.841225920122657,
4.59547880856323));
#90509=CARTESIAN_POINT('Ctrl Pts',(-2.24424210985445,0.770826238065321,
4.60080184167317));
#90510=CARTESIAN_POINT('Ctrl Pts',(-2.26976558264185,0.688113489908777,
4.60676488655015));
#90511=CARTESIAN_POINT('Ctrl Pts',(-2.2731450094232,0.676866128282533,4.60756961799544));
#90512=CARTESIAN_POINT('Ctrl Pts',(-2.27818895136523,0.659615013952774,
4.60879406222779));
#90513=CARTESIAN_POINT('Ctrl Pts',(-2.27991352656112,0.653629236209919,
4.60921711278326));
#90514=CARTESIAN_POINT('Ctrl Pts',(-2.2830297419906,0.642650854391736,4.60998962721873));
#90515=CARTESIAN_POINT('Ctrl Pts',(-2.28442859851994,0.637660491857268,
4.61033949400754));
#90516=CARTESIAN_POINT('Ctrl Pts',(-2.28753190277648,0.626448297927628,
4.61112269280696));
#90517=CARTESIAN_POINT('Ctrl Pts',(-2.28922732873539,0.620224085363706,
4.61155550068257));
#90518=CARTESIAN_POINT('Ctrl Pts',(-2.29350161224627,0.60427610910025,4.61265961374422));
#90519=CARTESIAN_POINT('Ctrl Pts',(-2.29604407064238,0.594542593925732,
4.61332888508663));
#90520=CARTESIAN_POINT('Ctrl Pts',(-2.31095562919788,0.535932821222687,
4.61733289063216));
#90521=CARTESIAN_POINT('Ctrl Pts',(-2.3218266685692,0.486684404389039,4.62058910258438));
#90522=CARTESIAN_POINT('Ctrl Pts',(-2.34749859101888,0.349779301689913,
4.62943829620707));
#90523=CARTESIAN_POINT('Ctrl Pts',(-2.35894752791029,0.261624378967379,
4.63491166268408));
#90524=CARTESIAN_POINT('Ctrl Pts',(-2.36542650810962,0.173076564653691,
4.64035944112689));
#90525=CARTESIAN_POINT('Origin',(0.,0.,-1.84858989190503));
#90526=CARTESIAN_POINT('',(-2.36542649454111,0.173076750093528,5.83682189647116));
#90527=CARTESIAN_POINT('',(-2.36542649454144,0.173076750089109,5.63753449772567));
#90528=CARTESIAN_POINT('',(-2.36542649454111,0.173076750093529,-1.84858989190503));
#90529=CARTESIAN_POINT('',(-2.37152864642643,-0.000916510297551713,4.84858989190502));
#90530=CARTESIAN_POINT('Ctrl Pts',(-2.3717498228844,-0.000916595774276441,
4.84858989190502));
#90531=CARTESIAN_POINT('Ctrl Pts',(-2.37171639157236,-0.0874222405099675,
4.85436572821342));
#90532=CARTESIAN_POINT('Ctrl Pts',(-2.36694602552388,-0.17378123686453,
4.86014156452181));
#90533=CARTESIAN_POINT('Ctrl Pts',(-2.3575118136592,-0.2594920248434,4.8659174008302));
#90534=CARTESIAN_POINT('Ctrl Pts',(-2.34805218476827,-0.345433729127539,
4.87170879801269));
#90535=CARTESIAN_POINT('Ctrl Pts',(-2.33390367225374,-0.430723412740602,
4.87750019519518));
#90536=CARTESIAN_POINT('Ctrl Pts',(-2.31519033196285,-0.514870652966122,
4.88329159237767));
#90537=CARTESIAN_POINT('Ctrl Pts',(-2.29639624105013,-0.599381000037756,
4.88910798023079));
#90538=CARTESIAN_POINT('Ctrl Pts',(-2.2729979807044,-0.682738715538656,
4.89492436808392));
#90539=CARTESIAN_POINT('Ctrl Pts',(-2.24516998327953,-0.764467009543649,
4.90074075593704));
#90540=CARTESIAN_POINT('Ctrl Pts',(-2.21986708128255,-0.838779328249715,
4.9060293683218));
#90541=CARTESIAN_POINT('Ctrl Pts',(-2.19090256384451,-0.911744606802647,
4.91131798070655));
#90542=CARTESIAN_POINT('Ctrl Pts',(-2.15844069284499,-0.983021789163822,
4.9166065930913));
#90543=CARTESIAN_POINT('Ctrl Pts',(-2.12571462659243,-1.05487907035018,
4.92193824755109));
#90544=CARTESIAN_POINT('Ctrl Pts',(-2.08933423057337,-1.12523662812698,
4.92726990201087));
#90545=CARTESIAN_POINT('Ctrl Pts',(-2.0494593632955,-1.19369777611438,4.93260155647066));
#90546=CARTESIAN_POINT('Ctrl Pts',(-2.00964221368882,-1.26205982864896,
4.93792549352096));
#90547=CARTESIAN_POINT('Ctrl Pts',(-1.96634087154654,-1.32853052080258,
4.94324943057125));
#90548=CARTESIAN_POINT('Ctrl Pts',(-1.9197625697357,-1.39273462595779,4.94857336762155));
#90549=CARTESIAN_POINT('Ctrl Pts',(-1.87323859286367,-1.45686384894796,
4.95389109528801));
#90550=CARTESIAN_POINT('Ctrl Pts',(-1.82344552529404,-1.51873136068186,
4.95920882295447));
#90551=CARTESIAN_POINT('Ctrl Pts',(-1.77063487472742,-1.57798929112305,
4.96452655062093));
#90552=CARTESIAN_POINT('Ctrl Pts',(-1.71785796100039,-1.63720936603182,
4.96984088118239));
#90553=CARTESIAN_POINT('Ctrl Pts',(-1.66206760155225,-1.69382281937187,
4.97515521174384));
#90554=CARTESIAN_POINT('Ctrl Pts',(-1.60355594992264,-1.74751434270729,
4.9804695423053));
#90555=CARTESIAN_POINT('Ctrl Pts',(-1.54506344174328,-1.80118829960976,
4.98578213415968));
#90556=CARTESIAN_POINT('Ctrl Pts',(-1.48385175452992,-1.85194190800883,
4.99109472601406));
#90557=CARTESIAN_POINT('Ctrl Pts',(-1.42024924886854,-1.89949733708377,
4.99640731786844));
#90558=CARTESIAN_POINT('Ctrl Pts',(-1.35664773074818,-1.94705202777685,
5.00171982723546));
#90559=CARTESIAN_POINT('Ctrl Pts',(-1.29065584428519,-1.99140835813315,
5.00703233660249));
#90560=CARTESIAN_POINT('Ctrl Pts',(-1.22263311438146,-2.03233027092495,
5.01234484596951));
#90561=CARTESIAN_POINT('Ctrl Pts',(-1.15454246275261,-2.0732930448659,5.01766265995753));
#90562=CARTESIAN_POINT('Ctrl Pts',(-1.08441731954588,-2.11081430839001,
5.02298047394555));
#90563=CARTESIAN_POINT('Ctrl Pts',(-1.01264363412979,-2.14470299406617,
5.02829828793356));
#90564=CARTESIAN_POINT('Ctrl Pts',(-0.940835604055967,-2.17860789592664,
5.03361864656591));
#90565=CARTESIAN_POINT('Ctrl Pts',(-0.867377894386582,-2.20887657821286,
5.03893900519825));
#90566=CARTESIAN_POINT('Ctrl Pts',(-0.792675972084069,-2.23536638289578,
5.04425936383059));
#90567=CARTESIAN_POINT('Ctrl Pts',(-0.717837583701502,-2.26190457936965,
5.04958944173741));
#90568=CARTESIAN_POINT('Ctrl Pts',(-0.641750891206771,-2.28464996903973,
5.05491951964424));
#90569=CARTESIAN_POINT('Ctrl Pts',(-0.564835856817695,-2.30351004281575,
5.06024959755106));
#90570=CARTESIAN_POINT('Ctrl Pts',(-0.491135775750442,-2.32158178883092,
5.06535688479273));
#90571=CARTESIAN_POINT('Ctrl Pts',(-0.416675591263177,-2.33608653528661,
5.07046417203439));
#90572=CARTESIAN_POINT('Ctrl Pts',(-0.34182939364102,-2.34698758585192,
5.07557145927605));
#90573=CARTESIAN_POINT('Ctrl Pts',(-0.26369514262485,-2.35836752829748,
5.08090311373587));
#90574=CARTESIAN_POINT('Ctrl Pts',(-0.184843782864509,-2.36586300792345,
5.08623476819567));
#90575=CARTESIAN_POINT('Ctrl Pts',(-0.105695390738131,-2.36939370871046,
5.09156642265548));
#90576=CARTESIAN_POINT('Ctrl Pts',(-0.0266615635290246,-2.37291929891427,
5.09689035970581));
#90577=CARTESIAN_POINT('Ctrl Pts',(0.0526679777719226,-2.3724914861672,
5.10221429675613));
#90578=CARTESIAN_POINT('Ctrl Pts',(0.131865556626997,-2.36808140431773,
5.10753823380646));
#90579=CARTESIAN_POINT('Ctrl Pts',(0.210970766214455,-2.36367646600973,
5.11285596147295));
#90580=CARTESIAN_POINT('Ctrl Pts',(0.289943853474334,-2.35529851430046,
5.11817368913943));
#90581=CARTESIAN_POINT('Ctrl Pts',(0.368356177697091,-2.3429707187356,5.12349141680592));
#90582=CARTESIAN_POINT('Ctrl Pts',(0.446718410054345,-2.33065079849242,
5.1288057473674));
#90583=CARTESIAN_POINT('Ctrl Pts',(0.524520128448813,-2.31438611523804,
5.13412007792888));
#90584=CARTESIAN_POINT('Ctrl Pts',(0.601338068909978,-2.29425164037854,
5.13943440849037));
#90585=CARTESIAN_POINT('Ctrl Pts',(0.678130876591922,-2.27412375298166,
5.14474700034477));
#90586=CARTESIAN_POINT('Ctrl Pts',(0.753940092245238,-2.25012870684461,
5.15005959219918));
#90587=CARTESIAN_POINT('Ctrl Pts',(0.828354364895945,-2.22239220405801,
5.15537218405358));
#90588=CARTESIAN_POINT('Ctrl Pts',(0.902767482133873,-2.19465613192952,
5.16068469342063));
#90589=CARTESIAN_POINT('Ctrl Pts',(0.975785260524075,-2.16317888362801,
5.16599720278768));
#90590=CARTESIAN_POINT('Ctrl Pts',(1.04701460391984,-2.12813497731666,5.17130971215473));
#90591=CARTESIAN_POINT('Ctrl Pts',(1.11831507089285,-2.09305607913456,5.17662752614277));
#90592=CARTESIAN_POINT('Ctrl Pts',(1.18782311378482,-2.05440361608756,5.18194534013082));
#90593=CARTESIAN_POINT('Ctrl Pts',(1.25516916125407,-2.01239867798027,5.18726315411886));
#90594=CARTESIAN_POINT('Ctrl Pts',(1.32254743469775,-1.97037363995454,5.19258351275123));
#90595=CARTESIAN_POINT('Ctrl Pts',(1.38776126633877,-1.92499319923414,5.1979038713836));
#90596=CARTESIAN_POINT('Ctrl Pts',(1.45047122366833,-1.87652106084906,5.20322423001597));
#90597=CARTESIAN_POINT('Ctrl Pts',(1.51329574005863,-1.82796037316684,5.20855430792282));
#90598=CARTESIAN_POINT('Ctrl Pts',(1.57360688486171,-1.77629700762958,5.21388438582967));
#90599=CARTESIAN_POINT('Ctrl Pts',(1.63109954567416,-1.7218340032075,5.21921446373652));
#90600=CARTESIAN_POINT('Ctrl Pts',(1.68618908435905,-1.66964748502227,5.22432175097794));
#90601=CARTESIAN_POINT('Ctrl Pts',(1.73869084946442,-1.61489101139677,5.22942903821936));
#90602=CARTESIAN_POINT('Ctrl Pts',(1.78837148814904,-1.557859262859,5.23453632546079));
#90603=CARTESIAN_POINT('Ctrl Pts',(1.84023463707511,-1.4983220639372,5.23986797992062));
#90604=CARTESIAN_POINT('Ctrl Pts',(1.88921980802755,-1.43607921553118,5.24519963438045));
#90605=CARTESIAN_POINT('Ctrl Pts',(1.93503207904738,-1.37144045279318,5.25053128884028));
#90606=CARTESIAN_POINT('Ctrl Pts',(1.9807780381827,-1.30689525272027,5.25585522589063));
#90607=CARTESIAN_POINT('Ctrl Pts',(2.02335994892682,-1.2399614045999,5.26117916294098));
#90608=CARTESIAN_POINT('Ctrl Pts',(2.06252203564278,-1.17098288415672,5.26650309999132));
#90609=CARTESIAN_POINT('Ctrl Pts',(2.10163844705754,-1.10208481434734,5.27182082765783));
#90610=CARTESIAN_POINT('Ctrl Pts',(2.13734273032496,-1.0311472168224,5.27713855532434));
#90611=CARTESIAN_POINT('Ctrl Pts',(2.16942234081596,-0.958543045287285,
5.28245628299085));
#90612=CARTESIAN_POINT('Ctrl Pts',(2.20148145800376,-0.8859852552162,5.28777061355236));
#90613=CARTESIAN_POINT('Ctrl Pts',(2.22992030934231,-0.811763432003007,
5.29308494411386));
#90614=CARTESIAN_POINT('Ctrl Pts',(2.25457281697321,-0.736274049159331,
5.29839927467537));
#90615=CARTESIAN_POINT('Ctrl Pts',(2.2792172589618,-0.660809364426271,5.30371186652979));
#90616=CARTESIAN_POINT('Ctrl Pts',(2.30007767165316,-0.584078388937312,
5.30902445838422));
#90617=CARTESIAN_POINT('Ctrl Pts',(2.31703708140918,-0.506495040326016,
5.31433705023865));
#90618=CARTESIAN_POINT('Ctrl Pts',(2.33399622784046,-0.428912896332979,
5.31964955960573));
#90619=CARTESIAN_POINT('Ctrl Pts',(2.34705439289442,-0.350478863877989,
5.3249620689728));
#90620=CARTESIAN_POINT('Ctrl Pts',(2.35614553017602,-0.271617935953395,
5.33027457833988));
#90621=CARTESIAN_POINT('Ctrl Pts',(2.36524574509576,-0.192678264198936,
5.33559239232794));
#90622=CARTESIAN_POINT('Ctrl Pts',(2.37037096546595,-0.113311312370886,
5.34091020631601));
#90623=CARTESIAN_POINT('Ctrl Pts',(2.37150703763578,-0.0339475027647511,
5.34622802030408));
#90624=CARTESIAN_POINT('Ctrl Pts',(2.37264365343118,0.0454542834739599,
5.35154837893648));
#90625=CARTESIAN_POINT('Ctrl Pts',(2.36978733515543,0.124852455261711,5.35686873756887));
#90626=CARTESIAN_POINT('Ctrl Pts',(2.36297607546678,0.203818863875749,5.36218909620127));
#90627=CARTESIAN_POINT('Ctrl Pts',(2.35615237291347,0.282929528968124,5.36751917410814));
#90628=CARTESIAN_POINT('Ctrl Pts',(2.34535935558681,0.36160638899144,5.37284925201501));
#90629=CARTESIAN_POINT('Ctrl Pts',(2.33068666681875,0.439428860696832,5.37817932992188));
#90630=CARTESIAN_POINT('Ctrl Pts',(2.31662727829782,0.513998449315545,5.3832866171631));
#90631=CARTESIAN_POINT('Ctrl Pts',(2.29900622707555,0.58778330749414,5.38839390440432));
#90632=CARTESIAN_POINT('Ctrl Pts',(2.27794497244047,0.660427713707715,5.39350119164554));
#90633=CARTESIAN_POINT('Ctrl Pts',(2.2559584800227,0.736263446862324,5.39883284610536));
#90634=CARTESIAN_POINT('Ctrl Pts',(2.23013914030922,0.81114389055524,5.40416450056517));
#90635=CARTESIAN_POINT('Ctrl Pts',(2.20058774310761,0.884653405229739,5.40949615502498));
#90636=CARTESIAN_POINT('Ctrl Pts',(2.17107912066471,0.958056517092479,5.41482009207531));
#90637=CARTESIAN_POINT('Ctrl Pts',(2.1378493418084,1.03009220924528,5.42014402912563));
#90638=CARTESIAN_POINT('Ctrl Pts',(2.10104917685267,1.10035922268446,5.42546796617596));
#90639=CARTESIAN_POINT('Ctrl Pts',(2.06429193245503,1.17054428270206,5.43078569384245));
#90640=CARTESIAN_POINT('Ctrl Pts',(2.02397279350614,1.23896435008457,5.43610342150894));
#90641=CARTESIAN_POINT('Ctrl Pts',(1.98029029697572,1.30523882956485,5.44142114917543));
#90642=CARTESIAN_POINT('Ctrl Pts',(1.93663570597882,1.3714709711557,5.44673547973692));
#90643=CARTESIAN_POINT('Ctrl Pts',(1.88962227932606,1.43555985490998,5.4520498102984));
#90644=CARTESIAN_POINT('Ctrl Pts',(1.83949348281343,1.49715122455512,5.45736414085989));
#90645=CARTESIAN_POINT('Ctrl Pts',(1.78938108710467,1.55872244314851,5.4626767327143));
#90646=CARTESIAN_POINT('Ctrl Pts',(1.73615564124393,1.61779740679662,5.46798932456871));
#90647=CARTESIAN_POINT('Ctrl Pts',(1.68010185893517,1.674053704665,5.47330191642312));
#90648=CARTESIAN_POINT('Ctrl Pts',(1.6240489469602,1.73030912905517,5.47861442579017));
#90649=CARTESIAN_POINT('Ctrl Pts',(1.56516811772133,1.78374564344214,5.48392693515723));
#90650=CARTESIAN_POINT('Ctrl Pts',(1.50378096462929,1.83407766272822,5.48923944452428));
#90651=CARTESIAN_POINT('Ctrl Pts',(1.44233251553598,1.88445993929718,5.49455725851233));
#90652=CARTESIAN_POINT('Ctrl Pts',(1.3783731067335,1.93173123028774,5.49987507250038));
#90653=CARTESIAN_POINT('Ctrl Pts',(1.31225698662644,1.97564664440534,5.50519288648842));
#90654=CARTESIAN_POINT('Ctrl Pts',(1.24610922908144,2.01958307262944,5.5105132451208));
#90655=CARTESIAN_POINT('Ctrl Pts',(1.177803107976,2.06016018510454,5.51583360375317));
#90656=CARTESIAN_POINT('Ctrl Pts',(1.10771918719346,2.09717816716259,5.52115396238555));
#90657=CARTESIAN_POINT('Ctrl Pts',(1.0375072365337,2.13426377397173,5.5264840402924));
#90658=CARTESIAN_POINT('Ctrl Pts',(0.965511422674827,2.16777705958948,5.53181411819925));
#90659=CARTESIAN_POINT('Ctrl Pts',(0.892133907124781,2.19756573377414,5.5371441961061));
#90660=CARTESIAN_POINT('Ctrl Pts',(0.821823480987807,2.22610927821386,5.5422514833475));
#90661=CARTESIAN_POINT('Ctrl Pts',(0.750244923385628,2.25123330724193,5.54735877058889));
#90662=CARTESIAN_POINT('Ctrl Pts',(0.67776308065634,2.27284739236915,5.55246605783029));
#90663=CARTESIAN_POINT('Ctrl Pts',(0.602097052532584,2.29541100156454,5.55779771229011));
#90664=CARTESIAN_POINT('Ctrl Pts',(0.525159509164951,2.31423475176091,5.56312936674993));
#90665=CARTESIAN_POINT('Ctrl Pts',(0.447354488944852,2.32917840100772,5.56846102120975));
#90666=CARTESIAN_POINT('Ctrl Pts',(0.369662089151608,2.34410041977167,5.57378495826008));
#90667=CARTESIAN_POINT('Ctrl Pts',(0.29110516261796,2.3551534030962,5.57910889531041));
#90668=CARTESIAN_POINT('Ctrl Pts',(0.212102710997206,2.36224691818777,5.58443283236075));
#90669=CARTESIAN_POINT('Ctrl Pts',(0.133192401064382,2.36933216001136,5.58975056002724));
#90670=CARTESIAN_POINT('Ctrl Pts',(0.0538380632305106,2.37246706880857,
5.59506828769373));
#90671=CARTESIAN_POINT('Ctrl Pts',(-0.0255328190202548,2.37161256061206,
5.60038601536023));
#90672=CARTESIAN_POINT('Ctrl Pts',(-0.104852997053299,2.37075859829797,
5.60570034592172));
#90673=CARTESIAN_POINT('Ctrl Pts',(-0.184189230931479,2.36592028241939,
5.61101467648321));
#90674=CARTESIAN_POINT('Ctrl Pts',(-0.263111863375871,2.35711056377313,
5.6163290070447));
#90675=CARTESIAN_POINT('Ctrl Pts',(-0.342008674442017,2.3483037274316,5.62164159889911));
#90676=CARTESIAN_POINT('Ctrl Pts',(-0.420491687137116,2.3355281203851,5.62695419075352));
#90677=CARTESIAN_POINT('Ctrl Pts',(-0.49813569284986,2.31884861386184,5.63226678260793));
#90678=CARTESIAN_POINT('Ctrl Pts',(-0.575778493002547,2.30216936631733,
5.63757929197499));
#90679=CARTESIAN_POINT('Ctrl Pts',(-0.652581853916395,2.28158643955674,
5.64289180134205));
#90680=CARTESIAN_POINT('Ctrl Pts',(-0.728131567745196,2.25721564821639,
5.64820431070911));
#90681=CARTESIAN_POINT('Ctrl Pts',(-0.803756719106482,2.2328205222721,5.65352212469716));
#90682=CARTESIAN_POINT('Ctrl Pts',(-0.878125275447008,2.20463012046381,
5.65883993868521));
#90683=CARTESIAN_POINT('Ctrl Pts',(-0.95083956891916,2.17280974240213,5.66415775267327));
#90684=CARTESIAN_POINT('Ctrl Pts',(-1.02358865714246,2.1409741378687,5.66947811130564));
#90685=CARTESIAN_POINT('Ctrl Pts',(-1.09468148538153,2.10550530633641,5.67479846993803));
#90686=CARTESIAN_POINT('Ctrl Pts',(-1.16374404259843,2.0666150744192,5.6801188285704));
#90687=CARTESIAN_POINT('Ctrl Pts',(-1.23293276385728,2.0276537975096,5.68544890647726));
#90688=CARTESIAN_POINT('Ctrl Pts',(-1.30008340518587,1.98525888159663,5.69077898438412));
#90689=CARTESIAN_POINT('Ctrl Pts',(-1.3648502243344,1.93968603841816,5.69610906229097));
#90690=CARTESIAN_POINT('Ctrl Pts',(-1.42690987053112,1.89601808373062,5.70121634953233));
#90691=CARTESIAN_POINT('Ctrl Pts',(-1.4867807505984,1.84943284505042,5.70632363677368));
#90692=CARTESIAN_POINT('Ctrl Pts',(-1.54418933615934,1.80018814477593,5.71143092401504));
#90693=CARTESIAN_POINT('Ctrl Pts',(-1.60323464352845,1.7495394754942,5.71668382028555));
#90694=CARTESIAN_POINT('Ctrl Pts',(-1.65991290861986,1.69587307641002,5.72193671655606));
#90695=CARTESIAN_POINT('Ctrl Pts',(-1.71389270879525,1.63944193103583,5.72718961282656));
#90696=CARTESIAN_POINT('Ctrl Pts',(-1.76780249533153,1.58308397877895,5.73243569591172));
#90697=CARTESIAN_POINT('Ctrl Pts',(-1.81902042514459,1.52396873529004,5.73768177899688));
#90698=CARTESIAN_POINT('Ctrl Pts',(-1.86724818186334,1.46238924019156,5.74292786208204));
#90699=CARTESIAN_POINT('Ctrl Pts',(-1.91542944584182,1.40086910923661,5.74816888781444));
#90700=CARTESIAN_POINT('Ctrl Pts',(-1.96062595724657,1.33688981662153,5.75340991354684));
#90701=CARTESIAN_POINT('Ctrl Pts',(-2.00257751185276,1.27077982810619,5.75865093927924));
#90702=CARTESIAN_POINT('Ctrl Pts',(-2.04450258508999,1.20471157065457,5.76388865668285));
#90703=CARTESIAN_POINT('Ctrl Pts',(-2.0831865077308,1.13651569351908,5.76912637408646));
#90704=CARTESIAN_POINT('Ctrl Pts',(-2.11841152831787,1.06655082353818,5.77436409149006));
#90705=CARTESIAN_POINT('Ctrl Pts',(-2.15364020563546,0.99657869046214,5.77960235262425));
#90706=CARTESIAN_POINT('Ctrl Pts',(-2.18540902907395,0.924837621173666,
5.78484061375845));
#90707=CARTESIAN_POINT('Ctrl Pts',(-2.21354609619333,0.851711067514837,
5.79007887489264));
#90708=CARTESIAN_POINT('Ctrl Pts',(-2.24168272106826,0.778585663222877,
5.79531705369444));
#90709=CARTESIAN_POINT('Ctrl Pts',(-2.26618753750677,0.704075272927715,
5.80055523249625));
#90710=CARTESIAN_POINT('Ctrl Pts',(-2.28693756719801,0.628581439622927,
5.80579341129805));
#90711=CARTESIAN_POINT('Ctrl Pts',(-2.30771013357672,0.553005612173924,
5.8110372793061));
#90712=CARTESIAN_POINT('Ctrl Pts',(-2.32471964709362,0.476444678008371,
5.81628114731416));
#90713=CARTESIAN_POINT('Ctrl Pts',(-2.33789380848674,0.399312662883799,
5.82152501532221));
#90714=CARTESIAN_POINT('Ctrl Pts',(-2.35070391868011,0.324312092927395,
5.82662397570519));
#90715=CARTESIAN_POINT('Ctrl Pts',(-2.35988791953829,0.248772024280277,
5.83172293608818));
#90716=CARTESIAN_POINT('Ctrl Pts',(-2.36542649454111,0.173076750093528,
5.83682189647117));
#90717=CARTESIAN_POINT('Ctrl Pts',(-2.36152614656945,0.172792042906829,
4.83696616984731));
#90718=CARTESIAN_POINT('Ctrl Pts',(-2.36575283962544,0.114983285525077,
4.84084074386655));
#90719=CARTESIAN_POINT('Ctrl Pts',(-2.36797226345534,0.0570274830161041,
4.84471531788578));
#90720=CARTESIAN_POINT('Ctrl Pts',(-2.36817286055345,-0.000915213407331403,
4.84858989190502));
#90721=CARTESIAN_POINT('Ctrl Pts',(-2.36542650810962,0.173076564653691,
4.64035944112689));
#90722=CARTESIAN_POINT('Ctrl Pts',(-2.36958750437766,0.11620849073354,4.64385816856119));
#90723=CARTESIAN_POINT('Ctrl Pts',(-2.37169861402987,0.0591783395543195,
4.6473459065507));
#90724=CARTESIAN_POINT('Ctrl Pts',(-2.37187441627101,-0.139696801513177,
4.65957190085794));
#90725=CARTESIAN_POINT('Ctrl Pts',(-2.35928471804046,-0.281195179106819,
4.66840388462315));
#90726=CARTESIAN_POINT('Ctrl Pts',(-2.33076725754395,-0.439412277896459,
4.67889885482005));
#90727=CARTESIAN_POINT('Ctrl Pts',(-2.32717196098186,-0.458071815686946,
4.68014611575948));
#90728=CARTESIAN_POINT('Ctrl Pts',(-2.32096629810687,-0.488318044859894,
4.68218432644276));
#90729=CARTESIAN_POINT('Ctrl Pts',(-2.31849238503274,-0.499932117136132,
4.68297093061465));
#90730=CARTESIAN_POINT('Ctrl Pts',(-2.31392669677645,-0.520603209596756,
4.68437824924146));
#90731=CARTESIAN_POINT('Ctrl Pts',(-2.31186868097277,-0.529667497215051,
4.6849978708061));
#90732=CARTESIAN_POINT('Ctrl Pts',(-2.3074103029407,-0.548782778761977,
4.6863099840861));
#90733=CARTESIAN_POINT('Ctrl Pts',(-2.30499743380498,-0.55883062610197,
4.68700286654199));
#90734=CARTESIAN_POINT('Ctrl Pts',(-2.29840578554732,-0.585510890930634,
4.68885132204143));
#90735=CARTESIAN_POINT('Ctrl Pts',(-2.29411220662824,-0.602114038084011,
4.69001057245143));
#90736=CARTESIAN_POINT('Ctrl Pts',(-2.27241353217401,-0.682418933247504,
4.69566223477256));
#90737=CARTESIAN_POINT('Ctrl Pts',(-2.25253471582891,-0.745415806194808,
4.70023399072073));
#90738=CARTESIAN_POINT('Ctrl Pts',(-2.1441084002122,-1.04485580356438,4.72265654250698));
#90739=CARTESIAN_POINT('Ctrl Pts',(-2.02084251121103,-1.26691945733865,
4.74163777198388));
#90740=CARTESIAN_POINT('Ctrl Pts',(-1.84615114052892,-1.48924364290899,
4.76152596786354));
#90741=CARTESIAN_POINT('Ctrl Pts',(-1.82692648703119,-1.51276584154836,
4.76363975863069));
#90742=CARTESIAN_POINT('Ctrl Pts',(-1.80117901025009,-1.54306196977669,
4.76636803702352));
#90743=CARTESIAN_POINT('Ctrl Pts',(-1.79506137817033,-1.55017441779998,
4.76700896340856));
#90744=CARTESIAN_POINT('Ctrl Pts',(-1.78514980427773,-1.56156040215943,
4.76803541661321));
#90745=CARTESIAN_POINT('Ctrl Pts',(-1.78138241755102,-1.56585676149367,
4.76842283420383));
#90746=CARTESIAN_POINT('Ctrl Pts',(-1.77410299657614,-1.57409800046261,
4.76916609350036));
#90747=CARTESIAN_POINT('Ctrl Pts',(-1.77059329011003,-1.57804478994432,
4.7695220899373));
#90748=CARTESIAN_POINT('Ctrl Pts',(-1.76219230082097,-1.58742868910293,
4.77036869305112));
#90749=CARTESIAN_POINT('Ctrl Pts',(-1.75728894690622,-1.59285501811389,
4.77085840217392));
#90750=CARTESIAN_POINT('Ctrl Pts',(-1.74058284090955,-1.61117190299985,
4.7725123198229));
#90751=CARTESIAN_POINT('Ctrl Pts',(-1.72866238350954,-1.62395502880084,
4.77366805130195));
#90752=CARTESIAN_POINT('Ctrl Pts',(-1.65894634051325,-1.69707872011143,
4.78029616251592));
#90753=CARTESIAN_POINT('Ctrl Pts',(-1.59812933158786,-1.75446998754613,
4.78556681533012));
#90754=CARTESIAN_POINT('Ctrl Pts',(-1.42435148284244,-1.90190701722134,
4.79971783485057));
#90755=CARTESIAN_POINT('Ctrl Pts',(-1.30600694536709,-1.98503775872641,
4.80842209538814));
#90756=CARTESIAN_POINT('Ctrl Pts',(-1.0922987666495,-2.10772487749247,4.82373939334999));
#90757=CARTESIAN_POINT('Ctrl Pts',(-1.00058111273251,-2.15277825297358,
4.83019812670082));
#90758=CARTESIAN_POINT('Ctrl Pts',(-0.889486987852479,-2.19871329877147,
4.83805331295552));
#90759=CARTESIAN_POINT('Ctrl Pts',(-0.872641041404239,-2.20545343512256,
4.83924507520915));
#90760=CARTESIAN_POINT('Ctrl Pts',(-0.844886856203886,-2.21619023954085,
4.8412103910151));
#90761=CARTESIAN_POINT('Ctrl Pts',(-0.834023441596768,-2.2203013012546,
4.84198010507378));
#90762=CARTESIAN_POINT('Ctrl Pts',(-0.814438309975678,-2.22754892226577,
4.84336881441311));
#90763=CARTESIAN_POINT('Ctrl Pts',(-0.805727518712207,-2.23071448716302,
4.8439868274527));
#90764=CARTESIAN_POINT('Ctrl Pts',(-0.787118261910398,-2.23735400640073,
4.84530799843798));
#90765=CARTESIAN_POINT('Ctrl Pts',(-0.777214883247635,-2.24081349677068,
4.84601162142694));
#90766=CARTESIAN_POINT('Ctrl Pts',(-0.750386593619699,-2.24998602444108,
4.84791934213024));
#90767=CARTESIAN_POINT('Ctrl Pts',(-0.733419840831615,-2.25557364247925,
4.84912754404924));
#90768=CARTESIAN_POINT('Ctrl Pts',(-0.644421085436879,-2.28377305469086,
4.85547545379374));
#90769=CARTESIAN_POINT('Ctrl Pts',(-0.571410207576451,-2.30312528322894,
4.86072019251129));
#90770=CARTESIAN_POINT('Ctrl Pts',(-0.33247284082339,-2.35439694656636,
4.87801375647445));
#90771=CARTESIAN_POINT('Ctrl Pts',(-0.16403828189332,-2.37208816754432,
4.89044295986019));
#90772=CARTESIAN_POINT('Ctrl Pts',(0.101522155663723,-2.3715486348334,4.90974652416848));
#90773=CARTESIAN_POINT('Ctrl Pts',(0.198135674569337,-2.3654379107527,4.91669603020138));
#90774=CARTESIAN_POINT('Ctrl Pts',(0.30669255033607,-2.35187124861168,4.92424452584912));
#90775=CARTESIAN_POINT('Ctrl Pts',(0.319256184966174,-2.35019875685072,
4.92511410572109));
#90776=CARTESIAN_POINT('Ctrl Pts',(0.338248455308202,-2.34751536240829,
4.92642192582697));
#90777=CARTESIAN_POINT('Ctrl Pts',(0.344687082686873,-2.34657861830053,
4.92686412384191));
#90778=CARTESIAN_POINT('Ctrl Pts',(0.356249778339127,-2.34484776533427,
4.92765603529009));
#90779=CARTESIAN_POINT('Ctrl Pts',(0.361375145359988,-2.34406334238391,
4.92800627822399));
#90780=CARTESIAN_POINT('Ctrl Pts',(0.372605607532094,-2.34230684120044,
4.92877198702889));
#90781=CARTESIAN_POINT('Ctrl Pts',(0.378709481809011,-2.34132770190248,
4.929187050444));
#90782=CARTESIAN_POINT('Ctrl Pts',(0.396176992378167,-2.33845559410089,
4.9303718496153));
#90783=CARTESIAN_POINT('Ctrl Pts',(0.407530956926957,-2.33650365020399,
4.93113834465011));
#90784=CARTESIAN_POINT('Ctrl Pts',(0.486400351730555,-2.3223522241704,4.93644031564106));
#90785=CARTESIAN_POINT('Ctrl Pts',(0.553380133549267,-2.30730960664079,
4.94082880884125));
#90786=CARTESIAN_POINT('Ctrl Pts',(0.728854234898164,-2.25981762930148,
4.95224645218833));
#90787=CARTESIAN_POINT('Ctrl Pts',(0.83583822756689,-2.22247192258956,4.95913039472828));
#90788=CARTESIAN_POINT('Ctrl Pts',(1.08290969665503,-2.11584867866025,4.97563993660907));
#90789=CARTESIAN_POINT('Ctrl Pts',(1.21960572734877,-2.04011299665807,4.98529814030505));
#90790=CARTESIAN_POINT('Ctrl Pts',(1.36343384922581,-1.9407740285796,4.9967102984867));
#90791=CARTESIAN_POINT('Ctrl Pts',(1.37886476396616,-1.92984134578562,4.99795164857562));
#90792=CARTESIAN_POINT('Ctrl Pts',(1.4037472110972,-1.91176153998665,4.99998210467897));
#90793=CARTESIAN_POINT('Ctrl Pts',(1.41327902351697,-1.90472591505883,5.00076692035723));
#90794=CARTESIAN_POINT('Ctrl Pts',(1.43019194971998,-1.89204529243752,5.00217224846935));
#90795=CARTESIAN_POINT('Ctrl Pts',(1.4375934062324,-1.88642773405491,5.0027916797455));
#90796=CARTESIAN_POINT('Ctrl Pts',(1.45316819196475,-1.87446188814205,5.00410465540781));
#90797=CARTESIAN_POINT('Ctrl Pts',(1.46133334156503,-1.86810332240308,5.00479859800287));
#90798=CARTESIAN_POINT('Ctrl Pts',(1.48297289354837,-1.85102295299052,5.00665289413923));
#90799=CARTESIAN_POINT('Ctrl Pts',(1.49637237518405,-1.84020766843638,5.00781696625321));
#90800=CARTESIAN_POINT('Ctrl Pts',(1.56125125142481,-1.78666403670446,5.01353262124101));
#90801=CARTESIAN_POINT('Ctrl Pts',(1.6110200834607,-1.74192037457744,5.01816574555396));
#90802=CARTESIAN_POINT('Ctrl Pts',(1.83330790602957,-1.52439390648444,5.04007413403612));
#90803=CARTESIAN_POINT('Ctrl Pts',(1.98034589048124,-1.32777732985035,5.05838552306888));
#90804=CARTESIAN_POINT('Ctrl Pts',(2.11187042801126,-1.08005885891602,5.07821024427486));
#90805=CARTESIAN_POINT('Ctrl Pts',(2.12820364740383,-1.04750820622824,5.08075355205018));
#90806=CARTESIAN_POINT('Ctrl Pts',(2.1480719863172,-1.00552741363043,5.08394425545566));
#90807=CARTESIAN_POINT('Ctrl Pts',(2.15230465795632,-0.996435299638573,
5.08463002952955));
#90808=CARTESIAN_POINT('Ctrl Pts',(2.15891810099998,-0.981990330373744,
5.0857109177359));
#90809=CARTESIAN_POINT('Ctrl Pts',(2.1613368711605,-0.976655162806269,5.08610828545883));
#90810=CARTESIAN_POINT('Ctrl Pts',(2.16587910907739,-0.966536670357887,
5.08685834226424));
#90811=CARTESIAN_POINT('Ctrl Pts',(2.16800648774321,-0.961755332687051,
5.08721125513887));
#90812=CARTESIAN_POINT('Ctrl Pts',(2.17294213324031,-0.950562746984249,
5.08803391100381));
#90813=CARTESIAN_POINT('Ctrl Pts',(2.17573786586754,-0.944146065265629,
5.08850288922842));
#90814=CARTESIAN_POINT('Ctrl Pts',(2.18470254003402,-0.923319324040966,
5.09001679556104));
#90815=CARTESIAN_POINT('Ctrl Pts',(2.19075720603034,-0.908860087931752,
5.09105507417976));
#90816=CARTESIAN_POINT('Ctrl Pts',(2.25119467072546,-0.760414472366681,
5.10159508530331));
#90817=CARTESIAN_POINT('Ctrl Pts',(2.29336764291616,-0.621759861784053,
5.11046051488164));
#90818=CARTESIAN_POINT('Ctrl Pts',(2.35781706658475,-0.309969334690424,
5.12997518060536));
#90819=CARTESIAN_POINT('Ctrl Pts',(2.37418193872334,-0.136503456506024,
5.14059314729835));
#90820=CARTESIAN_POINT('Ctrl Pts',(2.37100799731868,0.0659147618968592,
5.15371280471681));
#90821=CARTESIAN_POINT('Ctrl Pts',(2.37003547022854,0.094633145941178,5.15558987951059));
#90822=CARTESIAN_POINT('Ctrl Pts',(2.36793325115636,0.135007450346536,5.15825396071149));
#90823=CARTESIAN_POINT('Ctrl Pts',(2.36723860454223,0.146684268029842,5.1590274107023));
#90824=CARTESIAN_POINT('Ctrl Pts',(2.36587830994447,0.167012476841364,5.16037928113094));
#90825=CARTESIAN_POINT('Ctrl Pts',(2.3652515062043,0.175666313959956,5.16095647681534));
#90826=CARTESIAN_POINT('Ctrl Pts',(2.36384040087466,0.193769245611332,5.16216755474158));
#90827=CARTESIAN_POINT('Ctrl Pts',(2.3630468945568,0.203217447485967,5.16280171568578));
#90828=CARTESIAN_POINT('Ctrl Pts',(2.3610227015092,0.225701838432521,5.16431594111428));
#90829=CARTESIAN_POINT('Ctrl Pts',(2.3597406786836,0.238732976973948,5.1651976026863));
#90830=CARTESIAN_POINT('Ctrl Pts',(2.35502413595331,0.282916283050316,5.16820117808642));
#90831=CARTESIAN_POINT('Ctrl Pts',(2.35108020337706,0.314009581510047,5.17033897575745));
#90832=CARTESIAN_POINT('Ctrl Pts',(2.34013327349309,0.388462155081126,5.17551834039632));
#90833=CARTESIAN_POINT('Ctrl Pts',(2.33253995733963,0.431721555801046,5.17857740405909));
#90834=CARTESIAN_POINT('Ctrl Pts',(2.27178070594458,0.729123237045156,5.19995480941339));
#90835=CARTESIAN_POINT('Ctrl Pts',(2.17841193075139,0.973187009647618,5.21952396464893));
#90836=CARTESIAN_POINT('Ctrl Pts',(2.04430468537211,1.20251970749297,5.23810674015734));
#90837=CARTESIAN_POINT('Ctrl Pts',(2.04120420212942,1.20777510343126,5.23853256220397));
#90838=CARTESIAN_POINT('Ctrl Pts',(2.02801149174943,1.2299411657943,5.24032830990421));
#90839=CARTESIAN_POINT('Ctrl Pts',(2.01772874993391,1.24673839973457,5.2416884410536));
#90840=CARTESIAN_POINT('Ctrl Pts',(2.00303092899154,1.27008957250782,5.24357625061562));
#90841=CARTESIAN_POINT('Ctrl Pts',(1.99879086489227,1.2767519366088,5.24411451539301));
#90842=CARTESIAN_POINT('Ctrl Pts',(1.9918904446736,1.28747585967918,5.24498019769833));
#90843=CARTESIAN_POINT('Ctrl Pts',(1.98925080188293,1.29155057242852,5.2453089565948));
#90844=CARTESIAN_POINT('Ctrl Pts',(1.98364644225597,1.30014386155943,5.24600187864994));
#90845=CARTESIAN_POINT('Ctrl Pts',(1.98067875841125,1.30466046377341,5.24636583343412));
#90846=CARTESIAN_POINT('Ctrl Pts',(1.9733015255347,1.31580489534596,5.24726337145888));
#90847=CARTESIAN_POINT('Ctrl Pts',(1.96887394654821,1.32242081822958,5.24779576024279));
#90848=CARTESIAN_POINT('Ctrl Pts',(1.95227969403864,1.34694874307405,5.24976841498195));
#90849=CARTESIAN_POINT('Ctrl Pts',(1.93990076086245,1.36471683538012,5.25119516177622));
#90850=CARTESIAN_POINT('Ctrl Pts',(1.85086551681803,1.48885350594662,5.26116631366842));
#90851=CARTESIAN_POINT('Ctrl Pts',(1.76573782140808,1.58888863719543,5.26922580514489));
#90852=CARTESIAN_POINT('Ctrl Pts',(1.54566112505676,1.80783736319113,5.28826012583066));
#90853=CARTESIAN_POINT('Ctrl Pts',(1.40464485835204,1.91945505622121,5.29919384371791));
#90854=CARTESIAN_POINT('Ctrl Pts',(1.22821865607946,2.02915953439354,5.31266040889249));
#90855=CARTESIAN_POINT('Ctrl Pts',(1.20376035668701,2.04376377622626,5.31452154708535));
#90856=CARTESIAN_POINT('Ctrl Pts',(1.16893312841347,2.06371733494372,5.31716665624335));
#90857=CARTESIAN_POINT('Ctrl Pts',(1.15877804640699,2.06943647601103,5.31793732999073));
#90858=CARTESIAN_POINT('Ctrl Pts',(1.14099931623052,2.0792772117406,5.31928573446121));
#90859=CARTESIAN_POINT('Ctrl Pts',(1.13339440009178,2.0834323347137,5.31986225648868));
#90860=CARTESIAN_POINT('Ctrl Pts',(1.11741350487005,2.09205047633714,5.32107329740393));
#90861=CARTESIAN_POINT('Ctrl Pts',(1.10903318393702,2.09650507483446,5.32170810206271));
#90862=CARTESIAN_POINT('Ctrl Pts',(1.08898256795578,2.10700921200683,5.32322642888515));
#90863=CARTESIAN_POINT('Ctrl Pts',(1.07728837755898,2.1130122082572,5.3241115709997));
#90864=CARTESIAN_POINT('Ctrl Pts',(1.03726896156589,2.13313686657551,5.32713972252509));
#90865=CARTESIAN_POINT('Ctrl Pts',(1.00871229935887,2.14678809347021,5.32929897025036));
#90866=CARTESIAN_POINT('Ctrl Pts',(0.939383021990174,2.17824157422433,5.33454000822777));
#90867=CARTESIAN_POINT('Ctrl Pts',(0.898367281129536,2.19547548390258,5.33763985028059));
#90868=CARTESIAN_POINT('Ctrl Pts',(0.737103522343717,2.25795933809084,5.34982556919109));
#90869=CARTESIAN_POINT('Ctrl Pts',(0.613753556759715,2.29455910305775,5.35915740439147));
#90870=CARTESIAN_POINT('Ctrl Pts',(0.354389522121256,2.34909869588778,5.37851506146658));
#90871=CARTESIAN_POINT('Ctrl Pts',(0.21852482661771,2.36561005147958,5.38851101048582));
#90872=CARTESIAN_POINT('Ctrl Pts',(0.0628804492293648,2.37099334845528,
5.39934586989299));
#90873=CARTESIAN_POINT('Ctrl Pts',(0.0437697607818828,2.37142313301968,
5.40066538804387));
#90874=CARTESIAN_POINT('Ctrl Pts',(0.0168552671086221,2.37170293423537,
5.40250657254142));
#90875=CARTESIAN_POINT('Ctrl Pts',(0.0090548244163033,2.37174554343568,
5.40303816146754));
#90876=CARTESIAN_POINT('Ctrl Pts',(-0.00406417473779834,2.37175248072662,
5.40392863216674));
#90877=CARTESIAN_POINT('Ctrl Pts',(-0.00938260691341935,2.37173740451699,
5.40428864125856));
#90878=CARTESIAN_POINT('Ctrl Pts',(-0.0202378703297897,2.37167011803773,
5.40502136885009));
#90879=CARTESIAN_POINT('Ctrl Pts',(-0.0257746381442902,2.37161640866097,
5.40539400227327));
#90880=CARTESIAN_POINT('Ctrl Pts',(-0.0398906909192325,2.37143003588349,
5.40634135441722));
#90881=CARTESIAN_POINT('Ctrl Pts',(-0.0484696303383252,2.37127020454241,
5.40691457644622));
#90882=CARTESIAN_POINT('Ctrl Pts',(-0.0834092862056551,2.37042955813712,
5.40923955621948));
#90883=CARTESIAN_POINT('Ctrl Pts',(-0.109759861686733,2.36935567541848,
5.41097074639765));
#90884=CARTESIAN_POINT('Ctrl Pts',(-0.17939097030521,2.36535372603805,5.41549951029122));
#90885=CARTESIAN_POINT('Ctrl Pts',(-0.222619909798855,2.36167741628952,
5.41826417015449));
#90886=CARTESIAN_POINT('Ctrl Pts',(-0.484951876279791,2.33210002859751,
5.43488563560312));
#90887=CARTESIAN_POINT('Ctrl Pts',(-0.699658592419328,2.2769185362823,5.44793094355953));
#90888=CARTESIAN_POINT('Ctrl Pts',(-0.958812910309933,2.17012321162726,
5.46571199991051));
#90889=CARTESIAN_POINT('Ctrl Pts',(-1.01308820929539,2.14532241894269,5.46955127722558));
#90890=CARTESIAN_POINT('Ctrl Pts',(-1.0817868368128,2.11074235593228,5.47459211989386));
#90891=CARTESIAN_POINT('Ctrl Pts',(-1.09712049242692,2.10281303313422,5.47572917985459));
#90892=CARTESIAN_POINT('Ctrl Pts',(-1.12151439987146,2.08985904077007,5.47755796441454));
#90893=CARTESIAN_POINT('Ctrl Pts',(-1.13063085337342,2.08494106079851,5.4782459103448));
#90894=CARTESIAN_POINT('Ctrl Pts',(-1.14769912161092,2.07558851446122,5.47954253797135));
#90895=CARTESIAN_POINT('Ctrl Pts',(-1.15565821049458,2.07116755759574,5.48015072492854));
#90896=CARTESIAN_POINT('Ctrl Pts',(-1.17347510705874,2.06113630925734,5.48152030808656));
#90897=CARTESIAN_POINT('Ctrl Pts',(-1.18331846438394,2.05550094047568,5.48228259652656));
#90898=CARTESIAN_POINT('Ctrl Pts',(-1.20389611576184,2.04352334164099,5.483888201854));
#90899=CARTESIAN_POINT('Ctrl Pts',(-1.21462155052786,2.03716665592162,5.48473202691521));
#90900=CARTESIAN_POINT('Ctrl Pts',(-1.24259652983613,2.02028715623742,5.48695149894768));
#90901=CARTESIAN_POINT('Ctrl Pts',(-1.25976228369973,2.009628143272,5.48833206544398));
#90902=CARTESIAN_POINT('Ctrl Pts',(-1.31090147666786,1.97696076157795,5.49250226241416));
#90903=CARTESIAN_POINT('Ctrl Pts',(-1.34444832784393,1.95430163707798,5.49531520107348));
#90904=CARTESIAN_POINT('Ctrl Pts',(-1.53173742655295,1.82069277851525,5.51146902654031));
#90905=CARTESIAN_POINT('Ctrl Pts',(-1.67230338136944,1.6924902086597,5.52543729189875));
#90906=CARTESIAN_POINT('Ctrl Pts',(-1.8565585671351,1.47883808364882,5.54592444941382));
#90907=CARTESIAN_POINT('Ctrl Pts',(-1.9128802612953,1.40522775579877,5.55256759423489));
#90908=CARTESIAN_POINT('Ctrl Pts',(-1.97182491919088,1.31805299950105,5.55982784780263));
#90909=CARTESIAN_POINT('Ctrl Pts',(-1.97880820070951,1.30754554179505,5.56069338749701));
#90910=CARTESIAN_POINT('Ctrl Pts',(-1.98925862857628,1.2915457177675,5.56199635025198));
#90911=CARTESIAN_POINT('Ctrl Pts',(-1.99278747019717,1.2860942164689,5.56243768847128));
#90912=CARTESIAN_POINT('Ctrl Pts',(-1.9990932796895,1.27626447108673,5.56322869672522));
#90913=CARTESIAN_POINT('Ctrl Pts',(-2.00187830768283,1.2718915771005,5.5635788906497));
#90914=CARTESIAN_POINT('Ctrl Pts',(-2.0079582900927,1.2622756873784,5.56434524042111));
#90915=CARTESIAN_POINT('Ctrl Pts',(-2.01124705504146,1.25702891434748,5.56476098901073));
#90916=CARTESIAN_POINT('Ctrl Pts',(-2.02062120504914,1.24194277246746,5.56594971624367));
#90917=CARTESIAN_POINT('Ctrl Pts',(-2.02665530401196,1.23207150631075,5.56671942052561));
#90918=CARTESIAN_POINT('Ctrl Pts',(-2.06863063011897,1.16226065679106,5.57210893393199));
#90919=CARTESIAN_POINT('Ctrl Pts',(-2.10198319899789,1.10079575299984,5.57657615674104));
#90920=CARTESIAN_POINT('Ctrl Pts',(-2.23248519754584,0.832663616592894,
5.59529173423322));
#90921=CARTESIAN_POINT('Ctrl Pts',(-2.30223425814597,0.614040601513204,
5.60878614194203));
#90922=CARTESIAN_POINT('Ctrl Pts',(-2.34765271186541,0.340734190738411,
5.62648121305212));
#90923=CARTESIAN_POINT('Ctrl Pts',(-2.3541576934841,0.292427874392742,5.6296328163226));
#90924=CARTESIAN_POINT('Ctrl Pts',(-2.36081779389675,0.228022097629499,
5.63388261605264));
#90925=CARTESIAN_POINT('Ctrl Pts',(-2.36230416096772,0.212070184214435,
5.63493904269972));
#90926=CARTESIAN_POINT('Ctrl Pts',(-2.36426539688882,0.188431626328554,
5.6365106903392));
#90927=CARTESIAN_POINT('Ctrl Pts',(-2.36486464284438,0.180755533574063,
5.63702200834809));
#90928=CARTESIAN_POINT('Ctrl Pts',(-2.36542649454145,0.17307675008899,5.63753449772568));
#90929=CARTESIAN_POINT('Origin',(0.,0.,-1.84858989190503));
#90930=CARTESIAN_POINT('',(-2.36542649097266,0.173076798863304,6.83516330511797));
#90931=CARTESIAN_POINT('',(-2.36542649458272,0.173076749524953,6.63992069752827));
#90932=CARTESIAN_POINT('',(-2.36542649454111,0.173076750093529,-1.84858989190503));
#90933=CARTESIAN_POINT('',(-2.37174936880892,-0.00173018488177715,5.84847577200946));
#90934=CARTESIAN_POINT('Ctrl Pts',(-2.36542649097266,0.173076798863304,
6.83516330511797));
#90935=CARTESIAN_POINT('Ctrl Pts',(-2.36239649348597,0.214487527335679,
6.83221060003601));
#90936=CARTESIAN_POINT('Ctrl Pts',(-2.35827870088117,0.255823468632288,
6.82929290278159));
#90937=CARTESIAN_POINT('Ctrl Pts',(-2.35149985856541,0.309523430433347,
6.82555870176947));
#90938=CARTESIAN_POINT('Ctrl Pts',(-2.3498248886175,0.321992778120867,6.82469558143828));
#90939=CARTESIAN_POINT('Ctrl Pts',(-2.34714360213076,0.340817188454468,
6.82339917369846));
#90940=CARTESIAN_POINT('Ctrl Pts',(-2.34621055351314,0.34718220871066,6.82296196878176));
#90941=CARTESIAN_POINT('Ctrl Pts',(-2.34448962924959,0.358598062692276,
6.82217997809001));
#90942=CARTESIAN_POINT('Ctrl Pts',(-2.34371131539799,0.363650194419785,
6.82183466813806));
#90943=CARTESIAN_POINT('Ctrl Pts',(-2.34197284299442,0.374697378334203,
6.82108127597791));
#90944=CARTESIAN_POINT('Ctrl Pts',(-2.34100599849535,0.380691265673151,
6.82067357548603));
#90945=CARTESIAN_POINT('Ctrl Pts',(-2.33818227512663,0.397779124639109,
6.81951414891658));
#90946=CARTESIAN_POINT('Ctrl Pts',(-2.33626944621218,0.408863878237154,
6.81876550452044));
#90947=CARTESIAN_POINT('Ctrl Pts',(-2.32282569984133,0.48359317605611,6.81373926659921));
#90948=CARTESIAN_POINT('Ctrl Pts',(-2.30877312776872,0.546763186882581,
6.80959251326109));
#90949=CARTESIAN_POINT('Ctrl Pts',(-2.23457759216252,0.825889316317598,
6.7914090291213));
#90950=CARTESIAN_POINT('Ctrl Pts',(-2.14659191612895,1.03324007164408,6.77816957430384));
#90951=CARTESIAN_POINT('Ctrl Pts',(-2.00129232220707,1.27408424848588,6.76029845111335));
#90952=CARTESIAN_POINT('Ctrl Pts',(-1.97002650167567,1.32191390451803,6.75661758667882));
#90953=CARTESIAN_POINT('Ctrl Pts',(-1.92734144344122,1.38233030482115,6.75176727899503));
#90954=CARTESIAN_POINT('Ctrl Pts',(-1.91747013737626,1.39599081625172,6.75065680995948));
#90955=CARTESIAN_POINT('Ctrl Pts',(-1.90140709650536,1.41772798908525,6.7488668939515));
#90956=CARTESIAN_POINT('Ctrl Pts',(-1.8953073853557,1.42587219174202,6.74819102848461));
#90957=CARTESIAN_POINT('Ctrl Pts',(-1.88361503506092,1.44127597549491,6.74690255842353));
#90958=CARTESIAN_POINT('Ctrl Pts',(-1.87803234479443,1.44854290432811,6.74629035306979));
#90959=CARTESIAN_POINT('Ctrl Pts',(-1.86521349796526,1.46503039152873,6.74489128417443));
#90960=CARTESIAN_POINT('Ctrl Pts',(-1.8579508696085,1.47422996802471,6.74410337659854));
#90961=CARTESIAN_POINT('Ctrl Pts',(-1.83545124181449,1.50229992079303,6.74167660432467));
#90962=CARTESIAN_POINT('Ctrl Pts',(-1.81999313703158,1.52099020965799,6.74002888214876));
#90963=CARTESIAN_POINT('Ctrl Pts',(-1.78369035365146,1.56353774256823,6.73620223779732));
#90964=CARTESIAN_POINT('Ctrl Pts',(-1.76264926320664,1.58722051355428,6.73401550344207));
#90965=CARTESIAN_POINT('Ctrl Pts',(-1.68822861194474,1.66767934887966,6.72638477565455));
#90966=CARTESIAN_POINT('Ctrl Pts',(-1.63253423415591,1.72223694943101,6.72084932730787));
#90967=CARTESIAN_POINT('Ctrl Pts',(-1.47559444271971,1.86151038281402,6.70573375783291));
#90968=CARTESIAN_POINT('Ctrl Pts',(-1.36979656621939,1.94068402486398,6.69602356115621));
#90969=CARTESIAN_POINT('Ctrl Pts',(-1.23861700942068,2.02275735788989,6.68479647408051));
#90970=CARTESIAN_POINT('Ctrl Pts',(-1.219085787577,2.0345882408334,6.68314503689447));
#90971=CARTESIAN_POINT('Ctrl Pts',(-1.1809542949778,2.05693983679522,6.67996320328007));
#90972=CARTESIAN_POINT('Ctrl Pts',(-1.16237655377124,2.06749494178062,6.67843198943586));
#90973=CARTESIAN_POINT('Ctrl Pts',(-1.10166096604134,2.10091392103701,6.67349418857176));
#90974=CARTESIAN_POINT('Ctrl Pts',(-1.05896880896651,2.12275340681874,6.67012446048209));
#90975=CARTESIAN_POINT('Ctrl Pts',(-1.00591391596295,2.14789457557882,6.66608520275205));
#90976=CARTESIAN_POINT('Ctrl Pts',(-0.996155792751487,2.15243758604564,
6.66534830854618));
#90977=CARTESIAN_POINT('Ctrl Pts',(-0.980880856537691,2.15942288535779,
6.66420456417137));
#90978=CARTESIAN_POINT('Ctrl Pts',(-0.975385235201043,2.16191075152279,
6.66379502528418));
#90979=CARTESIAN_POINT('Ctrl Pts',(-0.96521255310511,2.16646923600531,6.66304063980613));
#90980=CARTESIAN_POINT('Ctrl Pts',(-0.960538314210664,2.16854568111346,
6.66269545061306));
#90981=CARTESIAN_POINT('Ctrl Pts',(-0.949924806382464,2.1732194880845,6.66191488758089));
#90982=CARTESIAN_POINT('Ctrl Pts',(-0.943981590558935,2.17580762945389,
6.66148007771738));
#90983=CARTESIAN_POINT('Ctrl Pts',(-0.925863766115912,2.18360933948141,
6.66016126776235));
#90984=CARTESIAN_POINT('Ctrl Pts',(-0.913655775259458,2.18874544095387,
6.6592818166453));
#90985=CARTESIAN_POINT('Ctrl Pts',(-0.784084368184924,2.2419852216568,6.65003775837734));
#90986=CARTESIAN_POINT('Ctrl Pts',(-0.663066909302293,2.28070998719904,
6.6421772597597));
#90987=CARTESIAN_POINT('Ctrl Pts',(-0.346534459684943,2.35465203887098,
6.62220805594224));
#90988=CARTESIAN_POINT('Ctrl Pts',(-0.148687939204253,2.37536420871635,
6.61021155508095));
#90989=CARTESIAN_POINT('Ctrl Pts',(0.0769607245850977,2.37066103469526,
6.59556293067362));
#90990=CARTESIAN_POINT('Ctrl Pts',(0.104484942857661,2.36960745435298,6.59376141024054));
#90991=CARTESIAN_POINT('Ctrl Pts',(0.144164511526693,2.36739593015381,6.59114035539814));
#90992=CARTESIAN_POINT('Ctrl Pts',(0.15633974470815,2.36662307334932,6.59033286143499));
#90993=CARTESIAN_POINT('Ctrl Pts',(0.177746557087909,2.36509830718153,6.58890714294588));
#90994=CARTESIAN_POINT('Ctrl Pts',(0.186980782203273,2.36438618336646,6.58829017892366));
#90995=CARTESIAN_POINT('Ctrl Pts',(0.206034672480333,2.36280446840757,6.58701299270216));
#90996=CARTESIAN_POINT('Ctrl Pts',(0.2158535457556,2.36192770505005,6.58635255650918));
#90997=CARTESIAN_POINT('Ctrl Pts',(0.241004539067627,2.35952373967243,6.58465487561567));
#90998=CARTESIAN_POINT('Ctrl Pts',(0.2563275621908,2.35790831611662,6.58361487549254));
#90999=CARTESIAN_POINT('Ctrl Pts',(0.320629590791626,2.3504951089313,6.57922586537475));
#91000=CARTESIAN_POINT('Ctrl Pts',(0.369434156124747,2.34331994471636,6.57583393054837));
#91001=CARTESIAN_POINT('Ctrl Pts',(0.498794164553883,2.32016018356242,6.56667387718558));
#91002=CARTESIAN_POINT('Ctrl Pts',(0.578797865108882,2.30150591841724,6.56082960592347));
#91003=CARTESIAN_POINT('Ctrl Pts',(0.80300077726726,2.23679887355092,6.543985425435));
#91004=CARTESIAN_POINT('Ctrl Pts',(0.94398233663671,2.18104900126282,6.53280808610936));
#91005=CARTESIAN_POINT('Ctrl Pts',(1.13644471084273,2.0827617950108,6.517269451714));
#91006=CARTESIAN_POINT('Ctrl Pts',(1.1929696263991,2.05090918332885,6.51267288432958));
#91007=CARTESIAN_POINT('Ctrl Pts',(1.25721813593359,2.0111476883741,6.5074667578661));
#91008=CARTESIAN_POINT('Ctrl Pts',(1.26627528432626,2.00545739941599,6.50673330671539));
#91009=CARTESIAN_POINT('Ctrl Pts',(1.28085467965955,1.99615952564365,6.50555379588315));
#91010=CARTESIAN_POINT('Ctrl Pts',(1.28640078951203,1.99258991607556,6.50510536912282));
#91011=CARTESIAN_POINT('Ctrl Pts',(1.2962287643113,1.98620625923233,6.50431131368709));
#91012=CARTESIAN_POINT('Ctrl Pts',(1.30051646938115,1.98340142894344,6.50396508907988));
#91013=CARTESIAN_POINT('Ctrl Pts',(1.30976403916918,1.97730918907636,6.50321881906587));
#91014=CARTESIAN_POINT('Ctrl Pts',(1.31472062827064,1.97401700577413,6.50281909904628));
#91015=CARTESIAN_POINT('Ctrl Pts',(1.32854401471498,1.96476030504954,6.50170492758854));
#91016=CARTESIAN_POINT('Ctrl Pts',(1.33738310919335,1.95875437086076,6.50099319098197));
#91017=CARTESIAN_POINT('Ctrl Pts',(1.3898583082066,1.92257802546464,6.49677004216902));
#91018=CARTESIAN_POINT('Ctrl Pts',(1.43251658981317,1.89100756805329,6.49334612324831));
#91019=CARTESIAN_POINT('Ctrl Pts',(1.57351228088135,1.77914745700038,6.48192647386613));
#91020=CARTESIAN_POINT('Ctrl Pts',(1.66645642123609,1.69240497841442,6.47421228289519));
#91021=CARTESIAN_POINT('Ctrl Pts',(1.85970314041212,1.48061699369025,6.45663122934411));
#91022=CARTESIAN_POINT('Ctrl Pts',(1.95517308434902,1.35203933031459,6.44674944940347));
#91023=CARTESIAN_POINT('Ctrl Pts',(2.04657249037062,1.19878649602293,6.43509740902278));
#91024=CARTESIAN_POINT('Ctrl Pts',(2.05596399159708,1.18260731168867,6.43386926048223));
#91025=CARTESIAN_POINT('Ctrl Pts',(2.07091594983215,1.1561323705261,6.43186185702301));
#91026=CARTESIAN_POINT('Ctrl Pts',(2.07659345541119,1.1459033737946,6.43108681478807));
#91027=CARTESIAN_POINT('Ctrl Pts',(2.08658153605222,1.12759012273576,6.42970000073125));
#91028=CARTESIAN_POINT('Ctrl Pts',(2.090921415242,1.11952205101748,6.42908928938134));
#91029=CARTESIAN_POINT('Ctrl Pts',(2.09998831305486,1.10242955795379,6.42779592282349));
#91030=CARTESIAN_POINT('Ctrl Pts',(2.1047041365032,1.09339944090773,6.4271128863998));
#91031=CARTESIAN_POINT('Ctrl Pts',(2.11709219046754,1.06930100238087,6.42529061481575));
#91032=CARTESIAN_POINT('Ctrl Pts',(2.12466158536467,1.0541807712242,6.42414779940345));
#91033=CARTESIAN_POINT('Ctrl Pts',(2.16054448767759,0.980546327184998,6.41858390131191));
#91034=CARTESIAN_POINT('Ctrl Pts',(2.18660346630006,0.920970921135726,6.4140858473953));
#91035=CARTESIAN_POINT('Ctrl Pts',(2.29725064503045,0.636744068258404,6.39262505281426));
#91036=CARTESIAN_POINT('Ctrl Pts',(2.34985058937652,0.40121469531636,6.37465229600322));
#91037=CARTESIAN_POINT('Ctrl Pts',(2.36910922974393,0.11962189203901,6.35461662334392));
#91038=CARTESIAN_POINT('Ctrl Pts',(2.37086628401135,0.0773405126507377,
6.35165172948856));
#91039=CARTESIAN_POINT('Ctrl Pts',(2.37164411208569,0.0246849394310393,
6.34803110781958));
#91040=CARTESIAN_POINT('Ctrl Pts',(2.37172924227082,0.0143370814770219,
6.34732303521107));
#91041=CARTESIAN_POINT('Ctrl Pts',(2.37175663163015,-0.00194883477221039,
6.34621441346017));
#91042=CARTESIAN_POINT('Ctrl Pts',(2.37174432059112,-0.00788653020719567,
6.34581142806732));
#91043=CARTESIAN_POINT('Ctrl Pts',(2.37168012137295,-0.0189006875714829,
6.3450662263417));
#91044=CARTESIAN_POINT('Ctrl Pts',(2.37163423381124,-0.0239769861441997,
6.34472369387298));
#91045=CARTESIAN_POINT('Ctrl Pts',(2.37149135694326,-0.0356398036958509,
6.34393880520891));
#91046=CARTESIAN_POINT('Ctrl Pts',(2.37138322748416,-0.0422260905602065,
6.34349707517851));
#91047=CARTESIAN_POINT('Ctrl Pts',(2.37096407876875,-0.0625880218969371,
6.34213588968068));
#91048=CARTESIAN_POINT('Ctrl Pts',(2.37056044527093,-0.0763617779763865,
6.34122142065141));
#91049=CARTESIAN_POINT('Ctrl Pts',(2.36549601564208,-0.209532377360633,
6.33243409190259));
#91050=CARTESIAN_POINT('Ctrl Pts',(2.35193797877032,-0.328437652506021,
6.32500495603257));
#91051=CARTESIAN_POINT('Ctrl Pts',(2.29074641445491,-0.648165588870033,
6.30498109131401));
#91052=CARTESIAN_POINT('Ctrl Pts',(2.22583241613452,-0.844570418934279,
6.29254817703081));
#91053=CARTESIAN_POINT('Ctrl Pts',(2.12593444838301,-1.05174980904635,6.27760889007402));
#91054=CARTESIAN_POINT('Ctrl Pts',(2.11517495783682,-1.07322400679646,6.27603828328488));
#91055=CARTESIAN_POINT('Ctrl Pts',(2.0986001394902,-1.10508692452149,6.27367262235648));
#91056=CARTESIAN_POINT('Ctrl Pts',(2.09302948632704,-1.11560172861481,6.27288612652966));
#91057=CARTESIAN_POINT('Ctrl Pts',(2.08327516106729,-1.13368311898736,6.27152334071085));
#91058=CARTESIAN_POINT('Ctrl Pts',(2.07912876433113,-1.14126963901535,6.2709483809903));
#91059=CARTESIAN_POINT('Ctrl Pts',(2.07044794557262,-1.15694831757623,6.26975346474412));
#91060=CARTESIAN_POINT('Ctrl Pts',(2.06590735222598,-1.16503687180161,6.26913329460183));
#91061=CARTESIAN_POINT('Ctrl Pts',(2.05513560747416,-1.18396453015402,6.26767318929662));
#91062=CARTESIAN_POINT('Ctrl Pts',(2.04886601573737,-1.19478132429664,6.26683187729822));
#91063=CARTESIAN_POINT('Ctrl Pts',(2.02802526295338,-1.23009097417759,6.26406252045436));
#91064=CARTESIAN_POINT('Ctrl Pts',(2.01309861498401,-1.2543700070325,6.26212160173201));
#91065=CARTESIAN_POINT('Ctrl Pts',(1.97674626518233,-1.31117852711607,6.25749045480803));
#91066=CARTESIAN_POINT('Ctrl Pts',(1.95495012253785,-1.34345995146858,6.25478708793931));
#91067=CARTESIAN_POINT('Ctrl Pts',(1.82171218888216,-1.5306815527133,6.23867546737853));
#91068=CARTESIAN_POINT('Ctrl Pts',(1.69270118782702,-1.67223290701709,6.22462038490807));
#91069=CARTESIAN_POINT('Ctrl Pts',(1.47644817419918,-1.85856387333622,6.20387963443048));
#91070=CARTESIAN_POINT('Ctrl Pts',(1.40109084863731,-1.91601349107674,6.19708261345989));
#91071=CARTESIAN_POINT('Ctrl Pts',(1.31208938842366,-1.97579769915946,6.18968618277438));
#91072=CARTESIAN_POINT('Ctrl Pts',(1.30163103559756,-1.98270314865796,6.18882646169767));
#91073=CARTESIAN_POINT('Ctrl Pts',(1.28573070573171,-1.99302179191498,6.18753413871277));
#91074=CARTESIAN_POINT('Ctrl Pts',(1.28032899656168,-1.99649617423959,6.18709765501801));
#91075=CARTESIAN_POINT('Ctrl Pts',(1.27060323232783,-2.00269608591159,6.18631642615164));
#91076=CARTESIAN_POINT('Ctrl Pts',(1.26628444068462,-2.00542960569357,6.18597116143956));
#91077=CARTESIAN_POINT('Ctrl Pts',(1.25680901165208,-2.01138413390584,6.18521725031906));
#91078=CARTESIAN_POINT('Ctrl Pts',(1.25164882135281,-2.01459927926368,6.1848089895165));
#91079=CARTESIAN_POINT('Ctrl Pts',(1.23687285453848,-2.02372701297762,6.18364636149306));
#91080=CARTESIAN_POINT('Ctrl Pts',(1.22722698979042,-2.02959094635472,6.1828951027205));
#91081=CARTESIAN_POINT('Ctrl Pts',(1.16120693031008,-2.06908322225391,6.17780290500921));
#91082=CARTESIAN_POINT('Ctrl Pts',(1.10349371200586,-2.10043099382029,6.17359677600057));
#91083=CARTESIAN_POINT('Ctrl Pts',(0.831022780086311,-2.23409127172142,
6.15450100693689));
#91084=CARTESIAN_POINT('Ctrl Pts',(0.602960272125606,-2.30612538574392,
6.14049064105049));
#91085=CARTESIAN_POINT('Ctrl Pts',(0.323316549712038,-2.35004437495338,
6.12236868443929));
#91086=CARTESIAN_POINT('Ctrl Pts',(0.278463526682619,-2.35578008010954,
6.11943997061636));
#91087=CARTESIAN_POINT('Ctrl Pts',(0.218085951187239,-2.36175268805271,
6.11545539589988));
#91088=CARTESIAN_POINT('Ctrl Pts',(0.202681441791024,-2.36312451128064,
6.11443514744303));
#91089=CARTESIAN_POINT('Ctrl Pts',(0.177425231078782,-2.36512489663515,
6.11275598315232));
#91090=CARTESIAN_POINT('Ctrl Pts',(0.167580904629891,-2.36584279373594,
6.11209988370629));
#91091=CARTESIAN_POINT('Ctrl Pts',(0.148496615315916,-2.36711480465946,
6.11082474215954));
#91092=CARTESIAN_POINT('Ctrl Pts',(0.139257311593275,-2.36767631659477,
6.11020594446512));
#91093=CARTESIAN_POINT('Ctrl Pts',(0.117651506328053,-2.36886249157385,
6.10875537773273));
#91094=CARTESIAN_POINT('Ctrl Pts',(0.105283026177298,-2.36944441909614,
6.10792228376503));
#91095=CARTESIAN_POINT('Ctrl Pts',(0.0651145845503644,-2.37101918341653,
6.10520760035641));
#91096=CARTESIAN_POINT('Ctrl Pts',(0.0373024771205957,-2.37161976028034,
6.10331383010153));
#91097=CARTESIAN_POINT('Ctrl Pts',(-0.109459459548115,-2.37220682773543,
6.09324179139596));
#91098=CARTESIAN_POINT('Ctrl Pts',(-0.228254854195834,-2.36373401639321,
6.08480339288133));
#91099=CARTESIAN_POINT('Ctrl Pts',(-0.471229339202864,-2.32791542711345,
6.06703192592368));
#91100=CARTESIAN_POINT('Ctrl Pts',(-0.594874432469824,-2.2994283066647,
6.05770387292772));
#91101=CARTESIAN_POINT('Ctrl Pts',(-0.745299102759525,-2.25182023655606,
6.04628897149488));
#91102=CARTESIAN_POINT('Ctrl Pts',(-0.77476098578532,-2.24185429428373,
6.04405081447384));
#91103=CARTESIAN_POINT('Ctrl Pts',(-0.852195690335419,-2.21395187149007,
6.03817494336151));
#91104=CARTESIAN_POINT('Ctrl Pts',(-0.899801647534457,-2.19503492170247,
6.03456928572836));
#91105=CARTESIAN_POINT('Ctrl Pts',(-0.95594151689227,-2.17059303460668,
6.03035523432686));
#91106=CARTESIAN_POINT('Ctrl Pts',(-0.965096174326821,-2.16653818078733,
6.02966929276538));
#91107=CARTESIAN_POINT('Ctrl Pts',(-0.980050032561339,-2.15980110498478,
6.02855118524911));
#91108=CARTESIAN_POINT('Ctrl Pts',(-0.985864444278068,-2.15715325820128,
6.02811702641031));
#91109=CARTESIAN_POINT('Ctrl Pts',(-0.996309660260205,-2.15234551848709,
6.02733824087445));
#91110=CARTESIAN_POINT('Ctrl Pts',(-1.00094422111427,-2.15019413956728,
6.02699310960761));
#91111=CARTESIAN_POINT('Ctrl Pts',(-1.00558943402976,-2.14801954205282,
6.02664760545554));
#91112=CARTESIAN_POINT('Ctrl Pts',(-1.00560692740749,-2.14801135248936,
6.02664630432953));
#91113=CARTESIAN_POINT('Ctrl Pts',(-1.00564165457892,-2.14799509437007,
6.02664372139654));
#91114=CARTESIAN_POINT('Ctrl Pts',(-1.00565888841172,-2.1479870258036,6.02664243958649));
#91115=CARTESIAN_POINT('Ctrl Pts',(-1.00569310075358,-2.1479710077066,6.02663989496804));
#91116=CARTESIAN_POINT('Ctrl Pts',(-1.00571007929939,-2.14796305816629,
6.02663863215674));
#91117=CARTESIAN_POINT('Ctrl Pts',(-1.00574378533899,-2.1479472761437,6.02663612521757));
#91118=CARTESIAN_POINT('Ctrl Pts',(-1.00576051281802,-2.14793944367554,
6.02663488109065));
#91119=CARTESIAN_POINT('Ctrl Pts',(-1.00579372078305,-2.14792389391816,
6.02663241121784));
#91120=CARTESIAN_POINT('Ctrl Pts',(-1.00581020127874,-2.14791617663139,
6.02663118547109));
#91121=CARTESIAN_POINT('Ctrl Pts',(-1.00584291946799,-2.14790085529514,
6.02662875204647));
#91122=CARTESIAN_POINT('Ctrl Pts',(-1.00585915709539,-2.14789325128341,
6.02662754437337));
#91123=CARTESIAN_POINT('Ctrl Pts',(-1.00589139327967,-2.14787815476995,
6.02662514681806));
#91124=CARTESIAN_POINT('Ctrl Pts',(-1.00590739191761,-2.14787066223682,
6.02662395692967));
#91125=CARTESIAN_POINT('Ctrl Pts',(-1.00593915416863,-2.14785578680541,
6.02662159464244));
#91126=CARTESIAN_POINT('Ctrl Pts',(-1.00595491774891,-2.14784840392887,
6.0266204222459));
#91127=CARTESIAN_POINT('Ctrl Pts',(-1.00598621372859,-2.14783374602929,
6.02661809465605));
#91128=CARTESIAN_POINT('Ctrl Pts',(-1.00600174609874,-2.14782647102611,
6.02661693946477));
#91129=CARTESIAN_POINT('Ctrl Pts',(-1.00603258327955,-2.14781202719547,
6.02661464601571));
#91130=CARTESIAN_POINT('Ctrl Pts',(-1.00604788814422,-2.14780485834868,
6.02661350775376));
#91131=CARTESIAN_POINT('Ctrl Pts',(-1.00607861960909,-2.14779046323324,
6.02661122218509));
#91132=CARTESIAN_POINT('Ctrl Pts',(-1.0060940462051,-2.14778323696337,6.02661007487874));
#91133=CARTESIAN_POINT('Ctrl Pts',(-1.00612485059905,-2.14776880687737,
6.02660778390434));
#91134=CARTESIAN_POINT('Ctrl Pts',(-1.00614022835534,-2.14776160308202,
6.02660664023936));
#91135=CARTESIAN_POINT('Ctrl Pts',(-1.00617093524703,-2.14774721786589,
6.02660435653443));
#91136=CARTESIAN_POINT('Ctrl Pts',(-1.00618626441533,-2.14774003643097,
6.026603216492));
#91137=CARTESIAN_POINT('Ctrl Pts',(-1.00621687448557,-2.14772569577338,
6.02660094000573));
#91138=CARTESIAN_POINT('Ctrl Pts',(-1.00623215537904,-2.14771853655595,
6.02659980356248));
#91139=CARTESIAN_POINT('Ctrl Pts',(-1.00626266914499,-2.14770424022214,
6.02659753425622));
#91140=CARTESIAN_POINT('Ctrl Pts',(-1.00627790204101,-2.14769710309599,
6.02659640139144));
#91141=CARTESIAN_POINT('Ctrl Pts',(-1.00630832007796,-2.14768285082391,
6.02659413922225));
#91142=CARTESIAN_POINT('Ctrl Pts',(-1.00632350524556,-2.1476757356667,6.02659300991583));
#91143=CARTESIAN_POINT('Ctrl Pts',(-1.00635382818239,-2.14766152716906,
6.02659075483677));
#91144=CARTESIAN_POINT('Ctrl Pts',(-1.00636896593287,-2.14765443383862,
6.02658962906549));
#91145=CARTESIAN_POINT('Ctrl Pts',(-1.0063991942562,-2.14764026889472,6.02658738104019));
#91146=CARTESIAN_POINT('Ctrl Pts',(-1.00641428484788,-2.14763319727366,
6.02658625878474));
#91147=CARTESIAN_POINT('Ctrl Pts',(-1.00644441918803,-2.14761907559541,
6.02658401776616));
#91148=CARTESIAN_POINT('Ctrl Pts',(-1.00645946292222,-2.14761202554612,
6.02658289900406));
#91149=CARTESIAN_POINT('Ctrl Pts',(-1.00648950375712,-2.14759794691675,
6.0265806649565));
#91150=CARTESIAN_POINT('Ctrl Pts',(-1.00650450087375,-2.1475909183304,6.02657954966982));
#91151=CARTESIAN_POINT('Ctrl Pts',(-1.00653444889226,-2.1475768824342,6.02657732254188));
#91152=CARTESIAN_POINT('Ctrl Pts',(-1.00654939972445,-2.14756987515819,
6.02657621070577));
#91153=CARTESIAN_POINT('Ctrl Pts',(-1.00657925534405,-2.14755588180656,
6.02657399046623));
#91154=CARTESIAN_POINT('Ctrl Pts',(-1.00659416014469,-2.14754889572591,
6.0265728820618));
#91155=CARTESIAN_POINT('Ctrl Pts',(-1.00662392395113,-2.14753494465132,
6.02657066866696));
#91156=CARTESIAN_POINT('Ctrl Pts',(-1.00663878298614,-2.14752797964485,
6.02656956367435));
#91157=CARTESIAN_POINT('Ctrl Pts',(-1.00666845552237,-2.14751407059974,
6.02656735708365));
#91158=CARTESIAN_POINT('Ctrl Pts',(-1.00668326904571,-2.14750712655188,
6.0265662554839));
#91159=CARTESIAN_POINT('Ctrl Pts',(-1.00671285092441,-2.14749325925594,
6.02656405565164));
#91160=CARTESIAN_POINT('Ctrl Pts',(-1.00672761924087,-2.14748633602723,
6.026562957422));
#91161=CARTESIAN_POINT('Ctrl Pts',(-1.00675711092601,-2.14747251026977,
6.02656076431351));
#91162=CARTESIAN_POINT('Ctrl Pts',(-1.00677183429801,-2.14746560774059,
6.02655966943439));
#91163=CARTESIAN_POINT('Ctrl Pts',(-1.01238901536777,-2.14483212176056,
6.0261419586633));
#91164=CARTESIAN_POINT('Ctrl Pts',(-1.01798125389777,-2.14218358641286,
6.02572670067114));
#91165=CARTESIAN_POINT('Ctrl Pts',(-1.03429204886649,-2.13438034925337,
6.02451708883166));
#91166=CARTESIAN_POINT('Ctrl Pts',(-1.04498247192894,-2.12916677732829,
6.0237262667899));
#91167=CARTESIAN_POINT('Ctrl Pts',(-1.0694490556912,-2.11700609399699,6.02191988688929));
#91168=CARTESIAN_POINT('Ctrl Pts',(-1.08319770121043,-2.11000446768699,
6.02090741321021));
#91169=CARTESIAN_POINT('Ctrl Pts',(-1.12846896679929,-2.08639052339599,
6.01757893478856));
#91170=CARTESIAN_POINT('Ctrl Pts',(-1.15968692821761,-2.06920132863935,
6.01529238185314));
#91171=CARTESIAN_POINT('Ctrl Pts',(-1.30804532298124,-1.98309957077005,
6.00441059785337));
#91172=CARTESIAN_POINT('Ctrl Pts',(-1.4195119398381,-1.90490371468249,5.99617609143742));
#91173=CARTESIAN_POINT('Ctrl Pts',(-1.54207211375442,-1.80216204176423,
5.98635844464451));
#91174=CARTESIAN_POINT('Ctrl Pts',(-1.56023490247544,-1.78646059504067,
5.9848822653925));
#91175=CARTESIAN_POINT('Ctrl Pts',(-1.6725712424867,-1.68632749833562,5.97560057057227));
#91176=CARTESIAN_POINT('Ctrl Pts',(-1.76009059158471,-1.59476314563626,
5.96767438752151));
#91177=CARTESIAN_POINT('Ctrl Pts',(-1.85167919458033,-1.48217118031905,
5.95819656984604));
#91178=CARTESIAN_POINT('Ctrl Pts',(-1.86329908656174,-1.46753661915126,
5.9569697594968));
#91179=CARTESIAN_POINT('Ctrl Pts',(-1.88190675446481,-1.44352407375356,
5.95496411162887));
#91180=CARTESIAN_POINT('Ctrl Pts',(-1.88900037851996,-1.43422883308548,
5.9541894744489));
#91181=CARTESIAN_POINT('Ctrl Pts',(-1.90152828644079,-1.41755851882537,
5.95280311144105));
#91182=CARTESIAN_POINT('Ctrl Pts',(-1.90698915853618,-1.41020364614544,
5.9521924434639));
#91183=CARTESIAN_POINT('Ctrl Pts',(-1.9184348070306,-1.39460023214132,5.95089888285282));
#91184=CARTESIAN_POINT('Ctrl Pts',(-1.92440928686034,-1.38634440429817,
5.95021560733883));
#91185=CARTESIAN_POINT('Ctrl Pts',(-1.94016408816266,-1.36427556750855,
5.94839201912898));
#91186=CARTESIAN_POINT('Ctrl Pts',(-1.94984992336837,-1.35039615057062,
5.94724811702544));
#91187=CARTESIAN_POINT('Ctrl Pts',(-1.99612268973972,-1.28255326662644,
5.94166995331878));
#91188=CARTESIAN_POINT('Ctrl Pts',(-2.03061928624485,-1.22720517826059,
5.93715824062264));
#91189=CARTESIAN_POINT('Ctrl Pts',(-2.14172365008245,-1.03140612123326,
5.92131619744516));
#91190=CARTESIAN_POINT('Ctrl Pts',(-2.20637533085743,-0.88468866950939,
5.9096124632956));
#91191=CARTESIAN_POINT('Ctrl Pts',(-2.27200001914009,-0.682624243660154,
5.89411155682401));
#91192=CARTESIAN_POINT('Ctrl Pts',(-2.28656803566439,-0.632113078932413,
5.89028918052477));
#91193=CARTESIAN_POINT('Ctrl Pts',(-2.31579602479463,-0.516467790260524,
5.88170517114246));
#91194=CARTESIAN_POINT('Ctrl Pts',(-2.32941033004485,-0.451109283366782,
5.87697144602369));
#91195=CARTESIAN_POINT('Ctrl Pts',(-2.34200045216955,-0.374630398346349,
5.87163021230572));
#91196=CARTESIAN_POINT('Ctrl Pts',(-2.34367750884852,-0.363991481848435,
5.87089161974628));
#91197=CARTESIAN_POINT('Ctrl Pts',(-2.34626794910025,-0.346797585288626,
5.86970548411986));
#91198=CARTESIAN_POINT('Ctrl Pts',(-2.34722644651092,-0.340249710716274,
5.86925553185338));
#91199=CARTESIAN_POINT('Ctrl Pts',(-2.34887869886702,-0.328623177020545,
5.86845980859675));
#91200=CARTESIAN_POINT('Ctrl Pts',(-2.34958340881228,-0.323546196627361,
5.86811343196532));
#91201=CARTESIAN_POINT('Ctrl Pts',(-2.35092002050089,-0.313682058718947,
5.86744259054819));
#91202=CARTESIAN_POINT('Ctrl Pts',(-2.35155375974119,-0.308895278150122,
5.86711801917119));
#91203=CARTESIAN_POINT('Ctrl Pts',(-2.35292637112213,-0.298278540813172,
5.86640022251461));
#91204=CARTESIAN_POINT('Ctrl Pts',(-2.35365820599988,-0.292447682505695,
5.86600738738861));
#91205=CARTESIAN_POINT('Ctrl Pts',(-2.35542698095829,-0.27791822282563,
5.86503183372));
#91206=CARTESIAN_POINT('Ctrl Pts',(-2.35643742515107,-0.269216396844644,
5.8644505275705));
#91207=CARTESIAN_POINT('Ctrl Pts',(-2.36689225779544,-0.174608463986798,
5.85816065486418));
#91208=CARTESIAN_POINT('Ctrl Pts',(-2.37168361370965,-0.0882439611840601,
5.85268828811318));
#91209=CARTESIAN_POINT('Ctrl Pts',(-2.37174931491709,-0.00180268974679477,
5.84731037310509));
#91210=CARTESIAN_POINT('Ctrl Pts',(-2.36542649454111,0.173076750093528,
5.83682189647117));
#91211=CARTESIAN_POINT('Ctrl Pts',(-2.36968735820944,0.114843857430324,
5.84074456160273));
#91212=CARTESIAN_POINT('Ctrl Pts',(-2.37179168735252,0.0565192335834641,
5.84466722673429));
#91213=CARTESIAN_POINT('Ctrl Pts',(-2.37174937408619,-0.0017230849568048,
5.84858989186585));
#91214=CARTESIAN_POINT('',(-2.37174917807861,-0.0010014824649929,5.64933374379984));
#91215=CARTESIAN_POINT('Ctrl Pts',(-2.36542649454145,0.17307675008899,5.63753449772568));
#91216=CARTESIAN_POINT('Ctrl Pts',(-2.36560061936644,0.170696999636211,
5.63769332455426));
#91217=CARTESIAN_POINT('Ctrl Pts',(-2.36577115263263,0.168316990748921,
5.63785226386776));
#91218=CARTESIAN_POINT('Ctrl Pts',(-2.36656180708301,0.157043781578322,
5.63860555501616));
#91219=CARTESIAN_POINT('Ctrl Pts',(-2.36713536850584,0.14814749237512,5.63920135913883));
#91220=CARTESIAN_POINT('Ctrl Pts',(-2.36819217453898,0.130178466331304,
5.6404075810499));
#91221=CARTESIAN_POINT('Ctrl Pts',(-2.36867346784838,0.121105769301657,
5.64101804978109));
#91222=CARTESIAN_POINT('Ctrl Pts',(-2.36989028236562,0.0953738939302946,
5.64275364584945));
#91223=CARTESIAN_POINT('Ctrl Pts',(-2.37050224432586,0.0787096876410045,
5.64388261705857));
#91224=CARTESIAN_POINT('Ctrl Pts',(-2.37148822085233,0.0410297989315304,
5.6464470834772));
#91225=CARTESIAN_POINT('Ctrl Pts',(-2.37175868112921,0.0200131535808708,
5.6478857009166));
#91226=CARTESIAN_POINT('Ctrl Pts',(-2.37174978765133,-0.00100363135235019,
5.6493328323041));
#91227=CARTESIAN_POINT('Ctrl Pts',(-2.37174978852891,-0.00100155531720748,
5.64933268935669));
#91228=CARTESIAN_POINT('Ctrl Pts',(-2.37164352059503,-0.25265111013939,
5.66666026014709));
#91229=CARTESIAN_POINT('Ctrl Pts',(-2.3314818712988,-0.502669839439992,
5.68534782967035));
#91230=CARTESIAN_POINT('Ctrl Pts',(-2.23099083816382,-0.807930067335497,
5.7084964503446));
#91231=CARTESIAN_POINT('Ctrl Pts',(-2.20624354312408,-0.8732483324028,5.71345291330625));
#91232=CARTESIAN_POINT('Ctrl Pts',(-2.17407648886176,-0.948010154838691,
5.71905808347072));
#91233=CARTESIAN_POINT('Ctrl Pts',(-2.16942752156901,-0.958601103420047,
5.71985047611426));
#91234=CARTESIAN_POINT('Ctrl Pts',(-2.16217112603119,-0.974808914280169,
5.72106010300624));
#91235=CARTESIAN_POINT('Ctrl Pts',(-2.15961895055886,-0.980450094712068,
5.7214805542687));
#91236=CARTESIAN_POINT('Ctrl Pts',(-2.15488915357983,-0.990796486453308,
5.72225057329077));
#91237=CARTESIAN_POINT('Ctrl Pts',(-2.1527182023096,-0.995504537562328,
5.72260052643411));
#91238=CARTESIAN_POINT('Ctrl Pts',(-2.14779287459998,-1.00609443412296,
5.72338671686396));
#91239=CARTESIAN_POINT('Ctrl Pts',(-2.1450297705687,-1.01197209866505,5.72382241060949));
#91240=CARTESIAN_POINT('Ctrl Pts',(-2.1368268685492,-1.02923673024633,5.72510045028314));
#91241=CARTESIAN_POINT('Ctrl Pts',(-2.13132018810372,-1.04059194030834,
5.72593880518431));
#91242=CARTESIAN_POINT('Ctrl Pts',(-2.08454888549568,-1.13510905485041,
5.73290279492563));
#91243=CARTESIAN_POINT('Ctrl Pts',(-2.03851936991568,-1.21583709985596,
5.73875970763128));
#91244=CARTESIAN_POINT('Ctrl Pts',(-1.88429052296251,-1.45282749523415,
5.75630196704557));
#91245=CARTESIAN_POINT('Ctrl Pts',(-1.76197769473203,-1.59896644506038,
5.767671633576));
#91246=CARTESIAN_POINT('Ctrl Pts',(-1.59427083611109,-1.75644850489534,
5.78226591336158));
#91247=CARTESIAN_POINT('Ctrl Pts',(-1.56430323833072,-1.78318982355163,
5.78483842293011));
#91248=CARTESIAN_POINT('Ctrl Pts',(-1.51834538867038,-1.82214957837045,
5.78874323828754));
#91249=CARTESIAN_POINT('Ctrl Pts',(-1.50285419560241,-1.8349471470548,5.79005283202768));
#91250=CARTESIAN_POINT('Ctrl Pts',(-1.47752655319581,-1.85533491325641,
5.79218463040832));
#91251=CARTESIAN_POINT('Ctrl Pts',(-1.46778958188249,-1.86304752739457,
5.79300199218648));
#91252=CARTESIAN_POINT('Ctrl Pts',(-1.4490539650235,-1.87764988846594,5.79457088144892));
#91253=CARTESIAN_POINT('Ctrl Pts',(-1.44006561842391,-1.88455233524633,
5.79532188206845));
#91254=CARTESIAN_POINT('Ctrl Pts',(-1.43090270378343,-1.89148500908713,
5.79608589365064));
#91255=CARTESIAN_POINT('Ctrl Pts',(-1.43077711925714,-1.89158000684779,
5.79609636469634));
#91256=CARTESIAN_POINT('Ctrl Pts',(-1.43052238465917,-1.89177265962518,
5.79611760347274));
#91257=CARTESIAN_POINT('Ctrl Pts',(-1.43039323404485,-1.89187031392613,
5.79612837123159));
#91258=CARTESIAN_POINT('Ctrl Pts',(-1.4301311075033,-1.89206847276602,5.79615022504056));
#91259=CARTESIAN_POINT('Ctrl Pts',(-1.42999813097738,-1.89216897651477,
5.79616131112176));
#91260=CARTESIAN_POINT('Ctrl Pts',(-1.42972806970698,-1.89237304427792,
5.79618382510407));
#91261=CARTESIAN_POINT('Ctrl Pts',(-1.4295909843142,-1.89247660740768,5.79619525303842));
#91262=CARTESIAN_POINT('Ctrl Pts',(-1.42931239657002,-1.89268702297861,
5.79621847640193));
#91263=CARTESIAN_POINT('Ctrl Pts',(-1.42917089348143,-1.89279387445275,
5.79623027186949));
#91264=CARTESIAN_POINT('Ctrl Pts',(-1.42888313250292,-1.89301111716922,
5.79625425839183));
#91265=CARTESIAN_POINT('Ctrl Pts',(-1.42873687380275,-1.8931215073296,5.79626644948855));
#91266=CARTESIAN_POINT('Ctrl Pts',(-1.42843923104685,-1.89334610192275,
5.79629125807869));
#91267=CARTESIAN_POINT('Ctrl Pts',(-1.42828784608697,-1.89346030515034,
5.79630387561898));
#91268=CARTESIAN_POINT('Ctrl Pts',(-1.42797954331297,-1.89369282752043,
5.79632957097407));
#91269=CARTESIAN_POINT('Ctrl Pts',(-1.42782262448709,-1.89381114531661,
5.79634264884139));
#91270=CARTESIAN_POINT('Ctrl Pts',(-1.42750280463764,-1.89405222917953,
5.79636930220332));
#91271=CARTESIAN_POINT('Ctrl Pts',(-1.4273399024832,-1.89417499373408,5.79638287775658));
#91272=CARTESIAN_POINT('Ctrl Pts',(-1.42700761912436,-1.89442533830914,
5.79641056778808));
#91273=CARTESIAN_POINT('Ctrl Pts',(-1.42683823664427,-1.89455291663139,
5.79642468233264));
#91274=CARTESIAN_POINT('Ctrl Pts',(-1.42656320003674,-1.89476001548673,
5.79644760010651));
#91275=CARTESIAN_POINT('Ctrl Pts',(-1.42645755634096,-1.89483954992081,
5.7964564027934));
#91276=CARTESIAN_POINT('Ctrl Pts',(-1.42622378958899,-1.89501551186902,
5.79647588078437));
#91277=CARTESIAN_POINT('Ctrl Pts',(-1.42609566340418,-1.89511193522535,
5.79648655625138));
#91278=CARTESIAN_POINT('Ctrl Pts',(-1.42581128666588,-1.89532590219913,
5.79651024982894));
#91279=CARTESIAN_POINT('Ctrl Pts',(-1.42565503137244,-1.89544343947615,
5.79652326818584));
#91280=CARTESIAN_POINT('Ctrl Pts',(-1.42530691291307,-1.89570523133822,
5.79655227054785));
#91281=CARTESIAN_POINT('Ctrl Pts',(-1.42511504240005,-1.89584947610455,
5.7965682549352));
#91282=CARTESIAN_POINT('Ctrl Pts',(-1.42468554926835,-1.89617225919652,
5.79660403370901));
#91283=CARTESIAN_POINT('Ctrl Pts',(-1.42444791501096,-1.89635078196553,
5.79662382870145));
#91284=CARTESIAN_POINT('Ctrl Pts',(-1.42297314047316,-1.89745827292467,
5.79674667130934));
#91285=CARTESIAN_POINT('Ctrl Pts',(-1.42173512747768,-1.89838607329354,
5.79684976438959));
#91286=CARTESIAN_POINT('Ctrl Pts',(-1.41318210851119,-1.90478287740268,
5.79756180674377));
#91287=CARTESIAN_POINT('Ctrl Pts',(-1.40583655979324,-1.9102107331337,5.7981723516872));
#91288=CARTESIAN_POINT('Ctrl Pts',(-1.38861814817107,-1.92278084667566,
5.7996013490787));
#91289=CARTESIAN_POINT('Ctrl Pts',(-1.37872130443466,-1.92988966027054,
5.80042107460918));
#91290=CARTESIAN_POINT('Ctrl Pts',(-1.34681535886223,-1.95243672978268,
5.80305883338443));
#91291=CARTESIAN_POINT('Ctrl Pts',(-1.32459906132585,-1.96757668658768,
5.80488812864631));
#91292=CARTESIAN_POINT('Ctrl Pts',(-1.13099670897635,-2.09474772250308,
5.82077267787698));
#91293=CARTESIAN_POINT('Ctrl Pts',(-0.94605809966199,-2.18450462048365,
5.83568150925143));
#91294=CARTESIAN_POINT('Ctrl Pts',(-0.638191641956783,-2.28742140951938,
5.85937213535218));
#91295=CARTESIAN_POINT('Ctrl Pts',(-0.52169745343123,-2.31677017497521,
5.86807495598809));
#91296=CARTESIAN_POINT('Ctrl Pts',(-0.389754124245291,-2.3395477181449,
5.87732743521931));
#91297=CARTESIAN_POINT('Ctrl Pts',(-0.376016943639302,-2.34179484251328,
5.87828345213837));
#91298=CARTESIAN_POINT('Ctrl Pts',(-0.355668554911659,-2.34493975006678,
5.87968800516814));
#91299=CARTESIAN_POINT('Ctrl Pts',(-0.349072372565663,-2.34593073936025,
5.88014151632692));
#91300=CARTESIAN_POINT('Ctrl Pts',(-0.337330317666764,-2.34764420623886,
5.8809455336139));
#91301=CARTESIAN_POINT('Ctrl Pts',(-0.332186171227807,-2.34837761269774,
5.88129664264268));
#91302=CARTESIAN_POINT('Ctrl Pts',(-0.321040608432324,-2.34992929135538,
5.88205491613039));
#91303=CARTESIAN_POINT('Ctrl Pts',(-0.315038459784062,-2.35074148250563,
5.8824617368412));
#91304=CARTESIAN_POINT('Ctrl Pts',(-0.298478904158658,-2.352917704224,5.88358008444642));
#91305=CARTESIAN_POINT('Ctrl Pts',(-0.287915161494948,-2.35423368625574,
5.88428897637085));
#91306=CARTESIAN_POINT('Ctrl Pts',(-0.23266796084399,-2.36073869401767,
5.88797444637277));
#91307=CARTESIAN_POINT('Ctrl Pts',(-0.187849042852606,-2.36472724463345,
5.89088933607169));
#91308=CARTESIAN_POINT('Ctrl Pts',(-0.0985806804751241,-2.37011705757224,
5.89659477654039));
#91309=CARTESIAN_POINT('Ctrl Pts',(-0.0541522024456966,-2.37154821828459,
5.89938525696319));
#91310=CARTESIAN_POINT('Ctrl Pts',(0.179518625458638,-2.3725046498886,5.91392236832583));
#91311=CARTESIAN_POINT('Ctrl Pts',(0.368152876807087,-2.35063204475772,
5.92523604500701));
#91312=CARTESIAN_POINT('Ctrl Pts',(0.617453587024003,-2.29095024475468,
5.94143947561378));
#91313=CARTESIAN_POINT('Ctrl Pts',(0.682022398383635,-2.27256376804027,
5.94574820714996));
#91314=CARTESIAN_POINT('Ctrl Pts',(0.762082865922435,-2.24604649654846,
5.95127597254893));
#91315=CARTESIAN_POINT('Ctrl Pts',(0.778385269496632,-2.24044895173486,
5.95241134983343));
#91316=CARTESIAN_POINT('Ctrl Pts',(0.804379249423792,-2.23120578711897,
5.95423806639015));
#91317=CARTESIAN_POINT('Ctrl Pts',(0.814110685978092,-2.2276734559981,5.95492564229107));
#91318=CARTESIAN_POINT('Ctrl Pts',(0.832531208999378,-2.22085032679191,
5.95623433645183));
#91319=CARTESIAN_POINT('Ctrl Pts',(0.841224715795494,-2.21757195176718,
5.95685502978516));
#91320=CARTESIAN_POINT('Ctrl Pts',(0.86095293595342,-2.20999961659303,5.95827065875023));
#91321=CARTESIAN_POINT('Ctrl Pts',(0.871975135035369,-2.20567396010796,
5.95906664601563));
#91322=CARTESIAN_POINT('Ctrl Pts',(0.90049581829444,-2.19423384100996,5.96113974963232));
#91323=CARTESIAN_POINT('Ctrl Pts',(0.917942232758514,-2.18699265866527,
5.96242110754909));
#91324=CARTESIAN_POINT('Ctrl Pts',(1.07868426769145,-2.11801400971624,5.97435242843188));
#91325=CARTESIAN_POINT('Ctrl Pts',(1.215618887166,-2.04249759000248,5.98548539149245));
#91326=CARTESIAN_POINT('Ctrl Pts',(1.4376130628623,-1.88979934865933,6.00509708836814));
#91327=CARTESIAN_POINT('Ctrl Pts',(1.52636532580569,-1.81886848107397,6.01343689573029));
#91328=CARTESIAN_POINT('Ctrl Pts',(1.65984233522129,-1.69551847548,6.02651924676869));
#91329=CARTESIAN_POINT('Ctrl Pts',(1.70796577252639,-1.64703199426663,6.03136347374993));
#91330=CARTESIAN_POINT('Ctrl Pts',(1.76168020460538,-1.58802182992971,6.03685850539932));
#91331=CARTESIAN_POINT('Ctrl Pts',(1.76936431108184,-1.57945573658155,6.03764681343532));
#91332=CARTESIAN_POINT('Ctrl Pts',(1.78107839695748,-1.56620432473983,6.03885153117371));
#91333=CARTESIAN_POINT('Ctrl Pts',(1.78515278456655,-1.56155876639799,6.03927111834033));
#91334=CARTESIAN_POINT('Ctrl Pts',(1.79261279932702,-1.55298560873611,6.04004031660864));
#91335=CARTESIAN_POINT('Ctrl Pts',(1.79600369016847,-1.54906284417673,6.0403903072451));
#91336=CARTESIAN_POINT('Ctrl Pts',(1.80362263570205,-1.54019019139871,6.04117753168807));
#91337=CARTESIAN_POINT('Ctrl Pts',(1.8078431872828,-1.53523400511345,6.04161421531363));
#91338=CARTESIAN_POINT('Ctrl Pts',(1.82023065230123,-1.52056550615132,6.04289788431874));
#91339=CARTESIAN_POINT('Ctrl Pts',(1.82834024858055,-1.5108047654104,6.04374082597503));
#91340=CARTESIAN_POINT('Ctrl Pts',(1.89831531260124,-1.42519384763072,6.05104171470197));
#91341=CARTESIAN_POINT('Ctrl Pts',(1.9555171070979,-1.34563608436072,6.05720056355624));
#91342=CARTESIAN_POINT('Ctrl Pts',(2.08672304532995,-1.1370337391475,6.07246031657022));
#91343=CARTESIAN_POINT('Ctrl Pts',(2.15381640537072,-1.00415853192139,6.08141817039771));
#91344=CARTESIAN_POINT('Ctrl Pts',(2.23042248411881,-0.808808755687088,
6.09451730864341));
#91345=CARTESIAN_POINT('Ctrl Pts',(2.25058033181989,-0.750895048197857,
6.09838923272766));
#91346=CARTESIAN_POINT('Ctrl Pts',(2.27635558317712,-0.666433015072911,
6.10406517614306));
#91347=CARTESIAN_POINT('Ctrl Pts',(2.28379763817206,-0.640465424549628,
6.1058139657998));
#91348=CARTESIAN_POINT('Ctrl Pts',(2.29634789639335,-0.593669969203855,
6.10897574655151));
#91349=CARTESIAN_POINT('Ctrl Pts',(2.30162026921757,-0.572888977318162,
6.11038344067438));
#91350=CARTESIAN_POINT('Ctrl Pts',(2.30922973128833,-0.541094062931542,
6.11254396789617));
#91351=CARTESIAN_POINT('Ctrl Pts',(2.31177141035443,-0.530129866787261,
6.11329022092351));
#91352=CARTESIAN_POINT('Ctrl Pts',(2.31606234559062,-0.511001931758536,
6.11459441058515));
#91353=CARTESIAN_POINT('Ctrl Pts',(2.31784672710881,-0.502846208584473,
6.1151512100008));
#91354=CARTESIAN_POINT('Ctrl Pts',(2.32176450549418,-0.484475529782045,
6.11640710177646));
#91355=CARTESIAN_POINT('Ctrl Pts',(2.32387360923528,-0.474255627470957,
6.11710695882104));
#91356=CARTESIAN_POINT('Ctrl Pts',(2.32936095095243,-0.446750285774738,
6.11899387208129));
#91357=CARTESIAN_POINT('Ctrl Pts',(2.33261414962988,-0.429440865989278,
6.1201848804274));
#91358=CARTESIAN_POINT('Ctrl Pts',(2.34666763333714,-0.349788886658925,
6.12568291458601));
#91359=CARTESIAN_POINT('Ctrl Pts',(2.35516241993981,-0.287071261502332,
6.130061908112));
#91360=CARTESIAN_POINT('Ctrl Pts',(2.37943180232297,-0.0313597398278462,
6.148130441687));
#91361=CARTESIAN_POINT('Ctrl Pts',(2.37405377868918,0.162873211078528,6.16242613955079));
#91362=CARTESIAN_POINT('Ctrl Pts',(2.3334132936838,0.431914028405834,6.18214234284624));
#91363=CARTESIAN_POINT('Ctrl Pts',(2.317829636573,0.508955494113488,6.18776571030832));
#91364=CARTESIAN_POINT('Ctrl Pts',(2.29426877791969,0.601511447794637,6.19439093476283));
#91365=CARTESIAN_POINT('Ctrl Pts',(2.28991218038564,0.617889549008795,6.19555816849853));
#91366=CARTESIAN_POINT('Ctrl Pts',(2.2834487278293,0.641180274425502,6.19720937229039));
#91367=CARTESIAN_POINT('Ctrl Pts',(2.2814853861732,0.648131678830813,6.19770108555274));
#91368=CARTESIAN_POINT('Ctrl Pts',(2.27803564598726,0.66013589177824,6.198548164334));
#91369=CARTESIAN_POINT('Ctrl Pts',(2.27656412921852,0.665192880184589,6.19890437820197));
#91370=CARTESIAN_POINT('Ctrl Pts',(2.27345035952992,0.675762241054621,6.19964751241828));
#91371=CARTESIAN_POINT('Ctrl Pts',(2.27180489248476,0.681273569104934,6.20003424370884));
#91372=CARTESIAN_POINT('Ctrl Pts',(2.26737398105875,0.6959198927091,6.2010600611649));
#91373=CARTESIAN_POINT('Ctrl Pts',(2.26455334720966,0.705044262775467,6.20169713463655));
#91374=CARTESIAN_POINT('Ctrl Pts',(2.25208683913038,0.744524990166895,6.20444609074892));
#91375=CARTESIAN_POINT('Ctrl Pts',(2.24188459421818,0.774704010454745,6.20652777912287));
#91376=CARTESIAN_POINT('Ctrl Pts',(2.14602509536759,1.04048983149595,6.22476273027979));
#91377=CARTESIAN_POINT('Ctrl Pts',(2.02411829607826,1.26135781528861,6.23938161213371));
#91378=CARTESIAN_POINT('Ctrl Pts',(1.82930402985824,1.5110228754464,6.25941183839382));
#91379=CARTESIAN_POINT('Ctrl Pts',(1.78660642885283,1.56127498276236,6.26364611463614));
#91380=CARTESIAN_POINT('Ctrl Pts',(1.73024200384967,1.62226830023338,6.26909000378854));
#91381=CARTESIAN_POINT('Ctrl Pts',(1.71847367238726,1.63472934808138,6.27021909355155));
#91382=CARTESIAN_POINT('Ctrl Pts',(1.69939691261262,1.65449537148487,6.27203808293578));
#91383=CARTESIAN_POINT('Ctrl Pts',(1.69217385703761,1.66188219578317,6.272724276117));
#91384=CARTESIAN_POINT('Ctrl Pts',(1.67836078779289,1.67582503084034,6.27403189038995));
#91385=CARTESIAN_POINT('Ctrl Pts',(1.6717800266233,1.68238996856526,6.27465289685876));
#91386=CARTESIAN_POINT('Ctrl Pts',(1.65670233121933,1.69725559220843,6.27607140568344));
#91387=CARTESIAN_POINT('Ctrl Pts',(1.64818134407532,1.70553141503085,6.2768699757662));
#91388=CARTESIAN_POINT('Ctrl Pts',(1.62585902272575,1.72688797432641,6.27895425197548));
#91389=CARTESIAN_POINT('Ctrl Pts',(1.61196213608799,1.73986714225083,6.2802442754692));
#91390=CARTESIAN_POINT('Ctrl Pts',(1.49024882828482,1.85083281569976,6.29148047793259));
#91391=CARTESIAN_POINT('Ctrl Pts',(1.37379218172203,1.93884098467862,6.30184377902377));
#91392=CARTESIAN_POINT('Ctrl Pts',(1.17560720141769,2.06174998487815,6.31878451813567));
#91393=CARTESIAN_POINT('Ctrl Pts',(1.09869490774124,2.10374296301721,6.32520396882803));
#91394=CARTESIAN_POINT('Ctrl Pts',(0.935067877722646,2.18165532529008,6.33839261979896));
#91395=CARTESIAN_POINT('Ctrl Pts',(0.848176009214477,2.21688366206929,6.34514384478063));
#91396=CARTESIAN_POINT('Ctrl Pts',(0.741903400349646,2.25280253618081,6.35293952008697));
#91397=CARTESIAN_POINT('Ctrl Pts',(0.724318054424877,2.25851795030297,6.35421469066821));
#91398=CARTESIAN_POINT('Ctrl Pts',(0.699526691615532,2.26625603611395,6.35598994503083));
#91399=CARTESIAN_POINT('Ctrl Pts',(0.69237576046333,2.26845097449551,6.35649940121703));
#91400=CARTESIAN_POINT('Ctrl Pts',(0.680130243775401,2.27214636788819,6.35736722092279));
#91401=CARTESIAN_POINT('Ctrl Pts',(0.675040818855446,2.2736635988542,6.35772654732124));
#91402=CARTESIAN_POINT('Ctrl Pts',(0.665189569395497,2.27656440428095,6.35841940723507));
#91403=CARTESIAN_POINT('Ctrl Pts',(0.660428478575191,2.2779501478118,6.35875307213003));
#91404=CARTESIAN_POINT('Ctrl Pts',(0.64755262969523,2.28165397807519,6.35965230007065));
#91405=CARTESIAN_POINT('Ctrl Pts',(0.639429689354419,2.28394372997664,6.36021623801014));
#91406=CARTESIAN_POINT('Ctrl Pts',(0.608978391316408,2.29235236502331,6.36231839492872));
#91407=CARTESIAN_POINT('Ctrl Pts',(0.586572166600323,2.29818781637954,6.3638412169786));
#91408=CARTESIAN_POINT('Ctrl Pts',(0.310643436690889,2.36575177604356,6.38234250638371));
#91409=CARTESIAN_POINT('Ctrl Pts',(0.0486684398523651,2.38557305746104,
6.39748784648216));
#91410=CARTESIAN_POINT('Ctrl Pts',(-0.277615625657801,2.35638691575043,
6.41820057974612));
#91411=CARTESIAN_POINT('Ctrl Pts',(-0.343637046383645,2.34766735666593,
6.42247557752387));
#91412=CARTESIAN_POINT('Ctrl Pts',(-0.426134999956826,2.33321722491782,
6.42796534867093));
#91413=CARTESIAN_POINT('Ctrl Pts',(-0.443036897512371,2.33006693860655,
6.4290978932103));
#91414=CARTESIAN_POINT('Ctrl Pts',(-0.470049500471686,2.32472762058551,
6.43092112837355));
#91415=CARTESIAN_POINT('Ctrl Pts',(-0.480182944354966,2.32265567335727,
6.43160808131974));
#91416=CARTESIAN_POINT('Ctrl Pts',(-0.499394698549412,2.31859641994398,
6.43291628712508));
#91417=CARTESIAN_POINT('Ctrl Pts',(-0.508475537562165,2.31662190419033,
6.43353711969187));
#91418=CARTESIAN_POINT('Ctrl Pts',(-0.529116236963151,2.31200663321201,
6.43495403717135));
#91419=CARTESIAN_POINT('Ctrl Pts',(-0.5406682927007,2.30933246905127,6.43575118092231));
#91420=CARTESIAN_POINT('Ctrl Pts',(-0.570624589086373,2.30216084944802,
6.43782928490675));
#91421=CARTESIAN_POINT('Ctrl Pts',(-0.58899555068453,2.29752936940754,6.43911452055364));
#91422=CARTESIAN_POINT('Ctrl Pts',(-0.756000064596244,2.25329146984254,
6.45089969773735));
#91423=CARTESIAN_POINT('Ctrl Pts',(-0.900478250844775,2.19954102965899,
6.46186805089603));
#91424=CARTESIAN_POINT('Ctrl Pts',(-1.1370107387608,2.08431288285918,6.48101152832534));
#91425=CARTESIAN_POINT('Ctrl Pts',(-1.23187959060156,2.02968635978568,6.48904571610723));
#91426=CARTESIAN_POINT('Ctrl Pts',(-1.38417757517021,1.92736770765579,6.50228511976788));
#91427=CARTESIAN_POINT('Ctrl Pts',(-1.44374834514962,1.88315878506548,6.50755908708761));
#91428=CARTESIAN_POINT('Ctrl Pts',(-1.51023041583423,1.82880822853708,6.5134743888991));
#91429=CARTESIAN_POINT('Ctrl Pts',(-1.51925006603606,1.82132223859127,6.51427755338328));
#91430=CARTESIAN_POINT('Ctrl Pts',(-1.53297410686293,1.80975887706714,6.51550011692175));
#91431=CARTESIAN_POINT('Ctrl Pts',(-1.53771839746722,1.80572947525135,6.51592283830246));
#91432=CARTESIAN_POINT('Ctrl Pts',(-1.54638402517318,1.79831069955638,6.51669503458054));
#91433=CARTESIAN_POINT('Ctrl Pts',(-1.55031010818538,1.79492715591652,6.51704491017287));
#91434=CARTESIAN_POINT('Ctrl Pts',(-1.55910203802877,1.78729980173313,6.51782847825032));
#91435=CARTESIAN_POINT('Ctrl Pts',(-1.56396165835234,1.78304898417524,6.5182616441885));
#91436=CARTESIAN_POINT('Ctrl Pts',(-1.57813476381062,1.77054893094451,6.51952536040642));
#91437=CARTESIAN_POINT('Ctrl Pts',(-1.5874009497539,1.76224603590044,6.5203520522118));
#91438=CARTESIAN_POINT('Ctrl Pts',(-1.65713257706351,1.69876721218072,6.52658089696703));
#91439=CARTESIAN_POINT('Ctrl Pts',(-1.71477782204225,1.64056046896255,6.53177491707383));
#91440=CARTESIAN_POINT('Ctrl Pts',(-1.86247474059268,1.47511344678568,6.54559967541651));
#91441=CARTESIAN_POINT('Ctrl Pts',(-1.94623076905406,1.36270326896003,6.5540422323445));
#91442=CARTESIAN_POINT('Ctrl Pts',(-2.0749762767777,1.15361578549244,6.5692385193745));
#91443=CARTESIAN_POINT('Ctrl Pts',(-2.12428396047665,1.06007996438854,6.57587846070062));
#91444=CARTESIAN_POINT('Ctrl Pts',(-2.17789213199494,0.939509286126425,
6.58445131741887));
#91445=CARTESIAN_POINT('Ctrl Pts',(-2.18819115352131,0.915265656650994,
6.58617531668177));
#91446=CARTESIAN_POINT('Ctrl Pts',(-2.2026731205161,0.879533093272834,6.58871901368476));
#91447=CARTESIAN_POINT('Ctrl Pts',(-2.20717464032213,0.868174772541766,
6.58952796881525));
#91448=CARTESIAN_POINT('Ctrl Pts',(-2.21496181824128,0.848073949802716,
6.59096049982565));
#91449=CARTESIAN_POINT('Ctrl Pts',(-2.21828399901025,0.839345802425944,
6.59158283554681));
#91450=CARTESIAN_POINT('Ctrl Pts',(-2.22511241544924,0.821082222959828,
6.5928858134757));
#91451=CARTESIAN_POINT('Ctrl Pts',(-2.22860909699271,0.81154344645067,6.59356675975158));
#91452=CARTESIAN_POINT('Ctrl Pts',(-2.23757555413144,0.786588379783388,
6.59534948724987));
#91453=CARTESIAN_POINT('Ctrl Pts',(-2.24294723750275,0.771137669957799,
6.59645449475848));
#91454=CARTESIAN_POINT('Ctrl Pts',(-2.26451733705607,0.70696232798761,6.60105019947246));
#91455=CARTESIAN_POINT('Ctrl Pts',(-2.27929010313608,0.657776875753961,
6.60458710088747));
#91456=CARTESIAN_POINT('Ctrl Pts',(-2.33027845221822,0.465574788540541,
6.61847480376621));
#91457=CARTESIAN_POINT('Ctrl Pts',(-2.35468277218743,0.319910369141827,
6.62916731607634));
#91458=CARTESIAN_POINT('Ctrl Pts',(-2.36542649458273,0.173076749524785,
6.63992069752829));
#91459=CARTESIAN_POINT('Origin',(0.,0.,-1.84858989190503));
#91460=CARTESIAN_POINT('',(-2.36542646504704,0.173077153186224,7.83873326832757));
#91461=CARTESIAN_POINT('',(-2.36542649614281,0.173076728203254,7.64172477676247));
#91462=CARTESIAN_POINT('',(-2.36542649454111,0.173076750093529,-1.84858989190503));
#91463=CARTESIAN_POINT('Ctrl Pts',(-2.36542646504704,0.173077153186224,
7.83873326832757));
#91464=CARTESIAN_POINT('Ctrl Pts',(-2.35859713820071,0.266412813979041,
7.83212657790829));
#91465=CARTESIAN_POINT('Ctrl Pts',(-2.34624650250625,0.359304652133148,
7.82537226129759));
#91466=CARTESIAN_POINT('Ctrl Pts',(-2.30671452143895,0.563280434734312,
7.81024149271578));
#91467=CARTESIAN_POINT('Ctrl Pts',(-2.27695014932979,0.673584236738167,
7.80185481430998));
#91468=CARTESIAN_POINT('Ctrl Pts',(-2.21768175819681,0.843455168062414,
7.78891858434391));
#91469=CARTESIAN_POINT('Ctrl Pts',(-2.19342301360757,0.904669167529441,
7.78425482366189));
#91470=CARTESIAN_POINT('Ctrl Pts',(-2.16205208087438,0.97511867786204,7.77894572581195));
#91471=CARTESIAN_POINT('Ctrl Pts',(-2.15738369884976,0.985404092282611,
7.77817212378772));
#91472=CARTESIAN_POINT('Ctrl Pts',(-2.15008901833257,1.00117543764157,7.77698867212681));
#91473=CARTESIAN_POINT('Ctrl Pts',(-2.14751488053171,1.00668509659365,7.77657576085194));
#91474=CARTESIAN_POINT('Ctrl Pts',(-2.14273828863819,1.01680716577538,7.77581822761812));
#91475=CARTESIAN_POINT('Ctrl Pts',(-2.14054212614924,1.02142233828548,7.7754732403832));
#91476=CARTESIAN_POINT('Ctrl Pts',(-2.13555337036302,1.03181931077721,7.77469696372537));
#91477=CARTESIAN_POINT('Ctrl Pts',(-2.13275221201588,1.03759688336428,7.77426621152597));
#91478=CARTESIAN_POINT('Ctrl Pts',(-2.12441831205146,1.0546097559616,7.77299943289799));
#91479=CARTESIAN_POINT('Ctrl Pts',(-2.11881989795727,1.06581290995251,7.77216735384925));
#91480=CARTESIAN_POINT('Ctrl Pts',(-2.07029449566352,1.16102492091658,7.76510933549118));
#91481=CARTESIAN_POINT('Ctrl Pts',(-2.02247335302033,1.24245899632823,7.75916181418998));
#91482=CARTESIAN_POINT('Ctrl Pts',(-1.86392018407025,1.47892827437336,7.74150957209283));
#91483=CARTESIAN_POINT('Ctrl Pts',(-1.7392797873306,1.62367896159526,7.73011247101089));
#91484=CARTESIAN_POINT('Ctrl Pts',(-1.56957625910148,1.77853325132801,7.71552800930969));
#91485=CARTESIAN_POINT('Ctrl Pts',(-1.53981872293582,1.80435811096509,7.71300279883867));
#91486=CARTESIAN_POINT('Ctrl Pts',(-1.49419925009088,1.84199802308108,7.70916804848646));
#91487=CARTESIAN_POINT('Ctrl Pts',(-1.47880941299403,1.85437612107044,7.70788039866558));
#91488=CARTESIAN_POINT('Ctrl Pts',(-1.45364809009576,1.87410103297913,7.70578363635452));
#91489=CARTESIAN_POINT('Ctrl Pts',(-1.44397103632676,1.88156718950209,7.70497920431179));
#91490=CARTESIAN_POINT('Ctrl Pts',(-1.42535110372405,1.89570482101435,7.70343485548718));
#91491=CARTESIAN_POINT('Ctrl Pts',(-1.4164179895194,1.90238865877847,7.70269544682371));
#91492=CARTESIAN_POINT('Ctrl Pts',(-1.40731247095666,1.9091018034619,7.70194318785404));
#91493=CARTESIAN_POINT('Ctrl Pts',(-1.40718675482854,1.90919446990786,7.70193280199882));
#91494=CARTESIAN_POINT('Ctrl Pts',(-1.40693194857391,1.90938225096314,7.70191175210349));
#91495=CARTESIAN_POINT('Ctrl Pts',(-1.40680285795568,1.90947736489825,7.70190108803752));
#91496=CARTESIAN_POINT('Ctrl Pts',(-1.40654104462256,1.90967022793526,7.70187946044391));
#91497=CARTESIAN_POINT('Ctrl Pts',(-1.40640832136201,1.9097679762929,7.70186849688749));
#91498=CARTESIAN_POINT('Ctrl Pts',(-1.40613896135281,1.90996631191575,7.7018462471179));
#91499=CARTESIAN_POINT('Ctrl Pts',(-1.4060023239998,1.9100668983558,7.70183496087285));
#91500=CARTESIAN_POINT('Ctrl Pts',(-1.40572482820554,1.91027113270616,7.70181204037269));
#91501=CARTESIAN_POINT('Ctrl Pts',(-1.40558396909825,1.91037477969586,7.70180040608258));
#91502=CARTESIAN_POINT('Ctrl Pts',(-1.40529769265285,1.91058537891128,7.7017767617064));
#91503=CARTESIAN_POINT('Ctrl Pts',(-1.4051522745702,1.91069233011366,7.70176475158111));
#91504=CARTESIAN_POINT('Ctrl Pts',(-1.40485650961055,1.91090980549179,7.70174032499689));
#91505=CARTESIAN_POINT('Ctrl Pts',(-1.40470616189514,1.91102032852965,7.70172790849357));
#91506=CARTESIAN_POINT('Ctrl Pts',(-1.40440012916865,1.91124524250924,7.70170263549223));
#91507=CARTESIAN_POINT('Ctrl Pts',(-1.40424444321824,1.91135963217648,7.70168977894445));
#91508=CARTESIAN_POINT('Ctrl Pts',(-1.4039272823144,1.91159260529264,7.70166358863627));
#91509=CARTESIAN_POINT('Ctrl Pts',(-1.40376580631556,1.91171118730194,7.70165025482076));
#91510=CARTESIAN_POINT('Ctrl Pts',(-1.40343656428871,1.91195290627821,7.70162306869952));
#91511=CARTESIAN_POINT('Ctrl Pts',(-1.4032687970762,1.91207604162608,7.70160921633113));
#91512=CARTESIAN_POINT('Ctrl Pts',(-1.40299949606084,1.91227364475057,7.7015869811886));
#91513=CARTESIAN_POINT('Ctrl Pts',(-1.40289797250772,1.91234812654189,7.70157859895711));
#91514=CARTESIAN_POINT('Ctrl Pts',(-1.40267370307335,1.9125126322138,7.70156008267231));
#91515=CARTESIAN_POINT('Ctrl Pts',(-1.40255095446362,1.91260265235726,7.70154994847458));
#91516=CARTESIAN_POINT('Ctrl Pts',(-1.40227892711332,1.91280210877508,7.70152749030266));
#91517=CARTESIAN_POINT('Ctrl Pts',(-1.40212964423217,1.91291153938853,7.70151516610906));
#91518=CARTESIAN_POINT('Ctrl Pts',(-1.40179749090975,1.9131549619345,7.70148774570849));
#91519=CARTESIAN_POINT('Ctrl Pts',(-1.40161461408571,1.91328894510912,7.70147264916351));
#91520=CARTESIAN_POINT('Ctrl Pts',(-1.40120566409264,1.91358846880083,7.7014388914654));
#91521=CARTESIAN_POINT('Ctrl Pts',(-1.40097958081774,1.91375399546139,7.70142022977654));
#91522=CARTESIAN_POINT('Ctrl Pts',(-1.39356384010784,1.91918140482585,7.70080813739702));
#91523=CARTESIAN_POINT('Ctrl Pts',(-1.38634470553244,1.92440271117738,7.70021314441324));
#91524=CARTESIAN_POINT('Ctrl Pts',(-1.36987210244326,1.93617587972856,7.69885736292171));
#91525=CARTESIAN_POINT('Ctrl Pts',(-1.36060078385588,1.94270227093378,7.69809561312119));
#91526=CARTESIAN_POINT('Ctrl Pts',(-1.33688729801939,1.95914197007981,7.69615042720372));
#91527=CARTESIAN_POINT('Ctrl Pts',(-1.32238165640151,1.96896206986078,7.69496349482084));
#91528=CARTESIAN_POINT('Ctrl Pts',(-1.2320120022656,2.02869188236615,7.68758559819184));
#91529=CARTESIAN_POINT('Ctrl Pts',(-1.15345179809127,2.07436484652869,7.68123928101915));
#91530=CARTESIAN_POINT('Ctrl Pts',(-0.887736527611923,2.20907729893899,
7.65998886571653));
#91531=CARTESIAN_POINT('Ctrl Pts',(-0.691549029664566,2.27812341566044,
7.6445434862203));
#91532=CARTESIAN_POINT('Ctrl Pts',(-0.459486059393531,2.32700973565514,
7.62768620384646));
#91533=CARTESIAN_POINT('Ctrl Pts',(-0.429953608869919,2.33264695726725,
7.62556821430839));
#91534=CARTESIAN_POINT('Ctrl Pts',(-0.380501906823794,2.34111525916777,
7.62207538756554));
#91535=CARTESIAN_POINT('Ctrl Pts',(-0.360640094876113,2.34425705667519,
7.62068688401175));
#91536=CARTESIAN_POINT('Ctrl Pts',(-0.333152031406262,2.34824755420108,
7.61878721344964));
#91537=CARTESIAN_POINT('Ctrl Pts',(-0.325558719069628,2.34931231989943,
7.61826475636649));
#91538=CARTESIAN_POINT('Ctrl Pts',(-0.312716905947515,2.35104959432534,
7.6173852267336));
#91539=CARTESIAN_POINT('Ctrl Pts',(-0.307471120690429,2.35174139100683,
7.61702708613879));
#91540=CARTESIAN_POINT('Ctrl Pts',(-0.297444982145176,2.35302948367331,
7.61634481355863));
#91541=CARTESIAN_POINT('Ctrl Pts',(-0.292665083883659,2.35362877662986,
7.6160205087947));
#91542=CARTESIAN_POINT('Ctrl Pts',(-0.279989928832113,2.35517874902322,
7.61516300546171));
#91543=CARTESIAN_POINT('Ctrl Pts',(-0.272091572147632,2.35610430181736,
7.61463120770876));
#91544=CARTESIAN_POINT('Ctrl Pts',(-0.243898549587004,2.35926438048947,
7.61274155579772));
#91545=CARTESIAN_POINT('Ctrl Pts',(-0.223579161974676,2.36127663509652,
7.61139549880651));
#91546=CARTESIAN_POINT('Ctrl Pts',(0.0607325000245537,2.38572926933319,
7.59275074674434));
#91547=CARTESIAN_POINT('Ctrl Pts',(0.32667571273809,2.36404879684728,7.57740314276114));
#91548=CARTESIAN_POINT('Ctrl Pts',(0.626261723691821,2.28799795602327,7.55786075552404));
#91549=CARTESIAN_POINT('Ctrl Pts',(0.668644327702617,2.27597293350804,7.55504683885569));
#91550=CARTESIAN_POINT('Ctrl Pts',(0.740556047261216,2.25338775305678,7.55016975966));
#91551=CARTESIAN_POINT('Ctrl Pts',(0.770256267070677,2.24340918180106,7.54812493260406));
#91552=CARTESIAN_POINT('Ctrl Pts',(0.811970298228573,2.22846826724015,7.545205464371));
#91553=CARTESIAN_POINT('Ctrl Pts',(0.824155219490051,2.22399072529079,7.54434687113046));
#91554=CARTESIAN_POINT('Ctrl Pts',(0.845060926720512,2.21611319502959,7.54286348748364));
#91555=CARTESIAN_POINT('Ctrl Pts',(0.853799563654025,2.21276116285665,7.54224031131249));
#91556=CARTESIAN_POINT('Ctrl Pts',(0.870469810806107,2.20625321273352,7.54104543075245));
#91557=CARTESIAN_POINT('Ctrl Pts',(0.878404688089678,2.20310601897893,7.54047402810891));
#91558=CARTESIAN_POINT('Ctrl Pts',(0.898968075931657,2.19482125323606,7.53898623178626));
#91559=CARTESIAN_POINT('Ctrl Pts',(0.911569436884585,2.1896175655554,7.53806761455233));
#91560=CARTESIAN_POINT('Ctrl Pts',(0.947665605990753,2.17434618032149,7.53541603037497));
#91561=CARTESIAN_POINT('Ctrl Pts',(0.971042823124448,2.164007199402,7.53367391140437));
#91562=CARTESIAN_POINT('Ctrl Pts',(1.16578528582348,2.07408806260248,7.51894640250906));
#91563=CARTESIAN_POINT('Ctrl Pts',(1.32721143025869,1.97468438494245,7.50524676484006));
#91564=CARTESIAN_POINT('Ctrl Pts',(1.58103012016887,1.77308772647009,7.48156875768949));
#91565=CARTESIAN_POINT('Ctrl Pts',(1.67957668927501,1.68003787485905,7.47170427028828));
#91566=CARTESIAN_POINT('Ctrl Pts',(1.77830126663248,1.56939832935967,7.4614706491221));
#91567=CARTESIAN_POINT('Ctrl Pts',(1.78686299040038,1.55964328736992,7.46058005893303));
#91568=CARTESIAN_POINT('Ctrl Pts',(1.79954573528522,1.54495130874593,7.45925676670227));
#91569=CARTESIAN_POINT('Ctrl Pts',(1.80372728270528,1.54006730109177,7.45881980440846));
#91570=CARTESIAN_POINT('Ctrl Pts',(1.81087956535331,1.53164441349969,7.45807134411544));
#91571=CARTESIAN_POINT('Ctrl Pts',(1.81385986391892,1.52811380630679,7.45775914979262));
#91572=CARTESIAN_POINT('Ctrl Pts',(1.82060701070292,1.52007325547495,7.45705165837129));
#91573=CARTESIAN_POINT('Ctrl Pts',(1.82436742448894,1.51555801334149,7.45665683149812));
#91574=CARTESIAN_POINT('Ctrl Pts',(1.83453291579958,1.50325934143804,7.45558793903481));
#91575=CARTESIAN_POINT('Ctrl Pts',(1.84090530920182,1.49544886854054,7.45491618863659));
#91576=CARTESIAN_POINT('Ctrl Pts',(1.87179016287247,1.45709753406977,7.45165073090195));
#91577=CARTESIAN_POINT('Ctrl Pts',(1.89559507612819,1.4259913688188,7.44910358447032));
#91578=CARTESIAN_POINT('Ctrl Pts',(2.06163939350298,1.19750809226236,7.43099581613569));
#91579=CARTESIAN_POINT('Ctrl Pts',(2.17354088267521,0.979862812330626,7.41676360529145));
#91580=CARTESIAN_POINT('Ctrl Pts',(2.27099985204871,0.687036662951345,7.39723536746917));
#91581=CARTESIAN_POINT('Ctrl Pts',(2.28904730857409,0.624276295934643,7.39304057083386));
#91582=CARTESIAN_POINT('Ctrl Pts',(2.3084862870845,0.544404088868842,7.38765113615887));
#91583=CARTESIAN_POINT('Ctrl Pts',(2.31231384060281,0.52791043502709,7.38653559542166));
#91584=CARTESIAN_POINT('Ctrl Pts',(2.3181619934658,0.501424889421902,7.38473944653926));
#91585=CARTESIAN_POINT('Ctrl Pts',(2.32029538919853,0.491458288167029,7.38406246505419));
#91586=CARTESIAN_POINT('Ctrl Pts',(2.32422403100956,0.472508863813081,7.3827731286825));
#91587=CARTESIAN_POINT('Ctrl Pts',(2.32603161068842,0.463528763632339,7.38216118126298));
#91588=CARTESIAN_POINT('Ctrl Pts',(2.33002746611611,0.443065150077618,7.38076446180649));
#91589=CARTESIAN_POINT('Ctrl Pts',(2.33218293781247,0.431575550882417,7.37997865868202));
#91590=CARTESIAN_POINT('Ctrl Pts',(2.33756138311075,0.401688546028813,7.37793025116457));
#91591=CARTESIAN_POINT('Ctrl Pts',(2.34065207857208,0.383268469866972,7.37666348599672));
#91592=CARTESIAN_POINT('Ctrl Pts',(2.36820305419092,0.206284174461328,7.36444853252089));
#91593=CARTESIAN_POINT('Ctrl Pts',(2.37672722837762,0.0456910543134037,
7.35298667603099));
#91594=CARTESIAN_POINT('Ctrl Pts',(2.36552636649971,-0.186047691462226,
7.3360863689165));
#91595=CARTESIAN_POINT('Ctrl Pts',(2.35882902810994,-0.257399111476526,
7.33084011283655));
#91596=CARTESIAN_POINT('Ctrl Pts',(2.33567110919041,-0.423069765918993,
7.31866030556069));
#91597=CARTESIAN_POINT('Ctrl Pts',(2.31670893203323,-0.516924836609715,
7.31176031181739));
#91598=CARTESIAN_POINT('Ctrl Pts',(2.28735364391774,-0.627340815716504,
7.30381981682918));
#91599=CARTESIAN_POINT('Ctrl Pts',(2.28236941463297,-0.645238793559342,
7.30253849389459));
#91600=CARTESIAN_POINT('Ctrl Pts',(2.27509768731547,-0.670211754459335,
7.30076055946019));
#91601=CARTESIAN_POINT('Ctrl Pts',(2.27298661842687,-0.677336783946034,
7.30025443165674));
#91602=CARTESIAN_POINT('Ctrl Pts',(2.26932823599783,-0.689474391795433,
7.29939431075049));
#91603=CARTESIAN_POINT('Ctrl Pts',(2.26779772659917,-0.69449193877369,7.29903935505281));
#91604=CARTESIAN_POINT('Ctrl Pts',(2.26481413523986,-0.704158160772356,
7.29835676261713));
#91605=CARTESIAN_POINT('Ctrl Pts',(2.26336337404955,-0.708807463754769,
7.29802898808188));
#91606=CARTESIAN_POINT('Ctrl Pts',(2.25983605606962,-0.719990319679812,
7.29724183107911));
#91607=CARTESIAN_POINT('Ctrl Pts',(2.25774545759106,-0.726519450813188,
7.29678326213378));
#91608=CARTESIAN_POINT('Ctrl Pts',(2.24995390860999,-0.750494726447138,
7.2951027915529));
#91609=CARTESIAN_POINT('Ctrl Pts',(2.24407863020956,-0.767884156626534,
7.29389060203576));
#91610=CARTESIAN_POINT('Ctrl Pts',(2.18660979501815,-0.931682752912291,
7.2825200662413));
#91611=CARTESIAN_POINT('Ctrl Pts',(2.12095311379356,-1.07278495583558,7.27307084842636));
#91612=CARTESIAN_POINT('Ctrl Pts',(1.95499435336365,-1.35367146213064,7.25308015244388));
#91613=CARTESIAN_POINT('Ctrl Pts',(1.8523766151989,-1.49101280217569,7.24256159582333));
#91614=CARTESIAN_POINT('Ctrl Pts',(1.72118565409415,-1.63192651773559,7.2299992364612));
#91615=CARTESIAN_POINT('Ctrl Pts',(1.7062590404462,-1.64752670732413,7.22858175789613));
#91616=CARTESIAN_POINT('Ctrl Pts',(1.68327644747264,-1.67089906110656,7.22641567090201));
#91617=CARTESIAN_POINT('Ctrl Pts',(1.67537471936943,-1.67882185279682,7.22567380703523));
#91618=CARTESIAN_POINT('Ctrl Pts',(1.66093456843582,-1.69309702014057,7.22432305533289));
#91619=CARTESIAN_POINT('Ctrl Pts',(1.65441498537867,-1.69946821458672,7.22371501354805));
#91620=CARTESIAN_POINT('Ctrl Pts',(1.64029056312016,-1.71311285839444,7.22240148512265));
#91621=CARTESIAN_POINT('Ctrl Pts',(1.63267374706394,-1.72037357178596,7.2216954633815));
#91622=CARTESIAN_POINT('Ctrl Pts',(1.61192434453083,-1.73989099019388,7.21977820898521));
#91623=CARTESIAN_POINT('Ctrl Pts',(1.59870063887065,-1.75204936758964,7.21856281032493));
#91624=CARTESIAN_POINT('Ctrl Pts',(1.53211559611749,-1.81188871202563,7.21247358060979));
#91625=CARTESIAN_POINT('Ctrl Pts',(1.47675875450595,-1.85728312342909,7.20750610062777));
#91626=CARTESIAN_POINT('Ctrl Pts',(1.25232140698049,-2.02494529556847,7.18771044423677));
#91627=CARTESIAN_POINT('Ctrl Pts',(1.06946727708176,-2.12718861147645,7.17220295262649));
#91628=CARTESIAN_POINT('Ctrl Pts',(0.816766957560711,-2.22757811294163,
7.15267450055625));
#91629=CARTESIAN_POINT('Ctrl Pts',(0.756963595577901,-2.2486040724997,7.14818954950338));
#91630=CARTESIAN_POINT('Ctrl Pts',(0.685685497273274,-2.27049746123778,
7.14305709042383));
#91631=CARTESIAN_POINT('Ctrl Pts',(0.674963437966963,-2.2737079171588,7.142290628263));
#91632=CARTESIAN_POINT('Ctrl Pts',(0.658402006244923,-2.27853935124699,
7.14111576685995));
#91633=CARTESIAN_POINT('Ctrl Pts',(0.65257865762519,-2.28021399757045,7.14070437349789));
#91634=CARTESIAN_POINT('Ctrl Pts',(0.641830016151763,-2.28326048265854,
7.13994826637109));
#91635=CARTESIAN_POINT('Ctrl Pts',(0.636906729965374,-2.28463870657681,
7.13960319751137));
#91636=CARTESIAN_POINT('Ctrl Pts',(0.625764110380621,-2.2877191514243,7.13882503332171));
#91637=CARTESIAN_POINT('Ctrl Pts',(0.619542276983423,-2.28941193478995,
7.13839248705704));
#91638=CARTESIAN_POINT('Ctrl Pts',(0.601092864758016,-2.29435077466064,
7.13711547545022));
#91639=CARTESIAN_POINT('Ctrl Pts',(0.588845890504762,-2.29752445994452,
7.13627505308196));
#91640=CARTESIAN_POINT('Ctrl Pts',(0.466933722638177,-2.32807794866601,
7.1279758186843));
#91641=CARTESIAN_POINT('Ctrl Pts',(0.355452973144535,-2.34768707150716,
7.12091856356863));
#91642=CARTESIAN_POINT('Ctrl Pts',(0.0813470902774454,-2.37591760865688,
7.10393650010297));
#91643=CARTESIAN_POINT('Ctrl Pts',(-0.081564445033582,-2.37590973708495,
7.09412794386011));
#91644=CARTESIAN_POINT('Ctrl Pts',(-0.310045515017346,-2.35235763083039,
7.07960934753421));
#91645=CARTESIAN_POINT('Ctrl Pts',(-0.376568074205888,-2.34262882198343,
7.07529433028151));
#91646=CARTESIAN_POINT('Ctrl Pts',(-0.459370191439679,-2.32690116971652,
7.06976955639437));
#91647=CARTESIAN_POINT('Ctrl Pts',(-0.476121682074541,-2.32353139527184,
7.06864394284447));
#91648=CARTESIAN_POINT('Ctrl Pts',(-0.502838253932188,-2.3178559780098,
7.06683541444242));
#91649=CARTESIAN_POINT('Ctrl Pts',(-0.512827580939557,-2.3156663211804,
7.06615621662041));
#91650=CARTESIAN_POINT('Ctrl Pts',(-0.531730766488592,-2.31139443694434,
7.06486513098005));
#91651=CARTESIAN_POINT('Ctrl Pts',(-0.540647364713944,-2.30932506896214,
7.06425366684398));
#91652=CARTESIAN_POINT('Ctrl Pts',(-0.560865676789947,-2.30450928065009,
7.06286147274528));
#91653=CARTESIAN_POINT('Ctrl Pts',(-0.572159544942579,-2.3017312568454,
7.06207973669673));
#91654=CARTESIAN_POINT('Ctrl Pts',(-0.601344154292878,-2.29432446878618,
7.06004889020675));
#91655=CARTESIAN_POINT('Ctrl Pts',(-0.61920175852899,-2.28956954653065,
7.05879573579285));
#91656=CARTESIAN_POINT('Ctrl Pts',(-0.750574781512671,-2.25293968640675,
7.0494969012744));
#91657=CARTESIAN_POINT('Ctrl Pts',(-0.861610127714849,-2.21285331412349,
7.04118363665795));
#91658=CARTESIAN_POINT('Ctrl Pts',(-1.15243018813763,-2.08264496413429,
7.01821288779835));
#91659=CARTESIAN_POINT('Ctrl Pts',(-1.32450408721529,-1.97767385047271,
7.00324126810711));
#91660=CARTESIAN_POINT('Ctrl Pts',(-1.50151292169903,-1.83611737657584,
6.98737059076585));
#91661=CARTESIAN_POINT('Ctrl Pts',(-1.52146327737978,-1.81962021043655,
6.98557561406372));
#91662=CARTESIAN_POINT('Ctrl Pts',(-1.54756118413861,-1.79731015534653,
6.98322358994138));
#91663=CARTESIAN_POINT('Ctrl Pts',(-1.55395256693055,-1.79178705163262,
6.98264725936922));
#91664=CARTESIAN_POINT('Ctrl Pts',(-1.56442345379187,-1.78264048173592,
6.98170273526608));
#91665=CARTESIAN_POINT('Ctrl Pts',(-1.56852013563661,-1.77903693484713,
6.98133311041173));
#91666=CARTESIAN_POINT('Ctrl Pts',(-1.57652818939613,-1.77194368030196,
6.98061047755162));
#91667=CARTESIAN_POINT('Ctrl Pts',(-1.58044047639011,-1.76845509968554,
6.98025739491826));
#91668=CARTESIAN_POINT('Ctrl Pts',(-1.59005897668736,-1.75982088586775,
6.97938912464548));
#91669=CARTESIAN_POINT('Ctrl Pts',(-1.59575187792092,-1.75466037965643,
6.97887504292403));
#91670=CARTESIAN_POINT('Ctrl Pts',(-1.61528609949086,-1.73677927980854,
6.97711002036254));
#91671=CARTESIAN_POINT('Ctrl Pts',(-1.62900164213386,-1.72392144682518,
6.9758689347841));
#91672=CARTESIAN_POINT('Ctrl Pts',(-1.74819459020511,-1.60948938671038,
6.96505167587362));
#91673=CARTESIAN_POINT('Ctrl Pts',(-1.84422319386273,-1.4984971709672,6.956102752247));
#91674=CARTESIAN_POINT('Ctrl Pts',(-2.00122720528134,-1.27888140576905,
6.93956184548723));
#91675=CARTESIAN_POINT('Ctrl Pts',(-2.06508501177404,-1.17297433140261,
6.93200211613002));
#91676=CARTESIAN_POINT('Ctrl Pts',(-2.14906488677702,-1.00539066205684,
6.9201323554964));
#91677=CARTESIAN_POINT('Ctrl Pts',(-2.17539680059664,-0.947068037957572,
6.91601955630612));
#91678=CARTESIAN_POINT('Ctrl Pts',(-2.20563472884328,-0.872156247685243,
6.91072252891918));
#91679=CARTESIAN_POINT('Ctrl Pts',(-2.21176537190557,-0.856489925674334,
6.90961405358843));
#91680=CARTESIAN_POINT('Ctrl Pts',(-2.22133331998129,-0.83125191234857,
6.90782658767819));
#91681=CARTESIAN_POINT('Ctrl Pts',(-2.22487670051025,-0.821720829886908,
6.90715116091621));
#91682=CARTESIAN_POINT('Ctrl Pts',(-2.23149712460786,-0.803556250096017,
6.90586302864958));
#91683=CARTESIAN_POINT('Ctrl Pts',(-2.23458563452362,-0.794927104901584,
6.90525071913964));
#91684=CARTESIAN_POINT('Ctrl Pts',(-2.24151376908877,-0.775210778895963,
6.90385071326976));
#91685=CARTESIAN_POINT('Ctrl Pts',(-2.24532126577143,-0.764112644565494,
6.90306196771814));
#91686=CARTESIAN_POINT('Ctrl Pts',(-2.25502148282346,-0.735139714666286,
6.90100082640634));
#91687=CARTESIAN_POINT('Ctrl Pts',(-2.26078396054019,-0.717222515071759,
6.89972418420463));
#91688=CARTESIAN_POINT('Ctrl Pts',(-2.30786272297779,-0.56463360682363,
6.88883255054628));
#91689=CARTESIAN_POINT('Ctrl Pts',(-2.337311039493,-0.426620982245834,6.87882847603298));
#91690=CARTESIAN_POINT('Ctrl Pts',(-2.36600858523276,-0.191071139730028,
6.86160922248717));
#91691=CARTESIAN_POINT('Ctrl Pts',(-2.37182185185997,-0.0946856752146957,
6.85453038374071));
#91692=CARTESIAN_POINT('Ctrl Pts',(-2.37170635525136,0.05894780034332,6.84335697066085));
#91693=CARTESIAN_POINT('Ctrl Pts',(-2.36959668181367,0.116083140830984,
6.83922711828715));
#91694=CARTESIAN_POINT('Ctrl Pts',(-2.36542649097266,0.173076798863304,
6.83516330511797));
#91695=CARTESIAN_POINT('Ctrl Pts',(-2.36542649458273,0.173076749524786,
6.63992069752828));
#91696=CARTESIAN_POINT('Ctrl Pts',(-2.36967747850252,0.114978882425194,
6.64417550326076));
#91697=CARTESIAN_POINT('Ctrl Pts',(-2.37178999848562,0.0566976894277928,
6.6484358273091));
#91698=CARTESIAN_POINT('Ctrl Pts',(-2.37174753504741,-0.004369630699211,
6.6528635848913));
#91699=CARTESIAN_POINT('Ctrl Pts',(-2.37174096292677,-0.0070899602370591,
6.65306074906281));
#91700=CARTESIAN_POINT('Ctrl Pts',(-2.37138061207792,-0.0942082585031944,
6.65937236008294));
#91701=CARTESIAN_POINT('Ctrl Pts',(-2.36652673115363,-0.178537856873665,
6.66540734168897));
#91702=CARTESIAN_POINT('Ctrl Pts',(-2.35579946062723,-0.274888910244556,
6.67209505017504));
#91703=CARTESIAN_POINT('Ctrl Pts',(-2.35431455585673,-0.287329081406165,
6.67295447783768));
#91704=CARTESIAN_POINT('Ctrl Pts',(-2.35191275908435,-0.306180275712124,
6.67425008836422));
#91705=CARTESIAN_POINT('Ctrl Pts',(-2.35106810000044,-0.312600030835821,
6.67469012229654));
#91706=CARTESIAN_POINT('Ctrl Pts',(-2.34949991417654,-0.324152874232651,
6.67547976544824));
#91707=CARTESIAN_POINT('Ctrl Pts',(-2.34878584499419,-0.329287091343433,
6.67582989003546));
#91708=CARTESIAN_POINT('Ctrl Pts',(-2.34717956071975,-0.340565286268546,
6.67659723469193));
#91709=CARTESIAN_POINT('Ctrl Pts',(-2.34628005439331,-0.346708109314429,
6.67701404011835));
#91710=CARTESIAN_POINT('Ctrl Pts',(-2.34362404520581,-0.364362449084394,
6.67820883628627));
#91711=CARTESIAN_POINT('Ctrl Pts',(-2.34180684115401,-0.375864858847475,
6.67898350036948));
#91712=CARTESIAN_POINT('Ctrl Pts',(-2.32815459406481,-0.458334600875785,
6.68451350013596));
#91713=CARTESIAN_POINT('Ctrl Pts',(-2.31317915540793,-0.528752235816668,
6.6891070262067));
#91714=CARTESIAN_POINT('Ctrl Pts',(-2.26725313977886,-0.704894486627939,
6.7005181392203));
#91715=CARTESIAN_POINT('Ctrl Pts',(-2.23210141579862,-0.80934462105835,
6.70721530085243));
#91716=CARTESIAN_POINT('Ctrl Pts',(-2.13011598400987,-1.05449801690206,
6.72350630122272));
#91717=CARTESIAN_POINT('Ctrl Pts',(-2.0564570265753,-1.19177801976795,6.73313665764792));
#91718=CARTESIAN_POINT('Ctrl Pts',(-1.95936915926106,-1.33657345989726,
6.744518199362));
#91719=CARTESIAN_POINT('Ctrl Pts',(-1.94864364943561,-1.35216271558097,
6.7457602750314));
#91720=CARTESIAN_POINT('Ctrl Pts',(-1.93089961923421,-1.37730358266181,
6.74779168315955));
#91721=CARTESIAN_POINT('Ctrl Pts',(-1.9239938700328,-1.38693405676526,6.74857671851891));
#91722=CARTESIAN_POINT('Ctrl Pts',(-1.91154495403558,-1.40402289777107,
6.7499822908886));
#91723=CARTESIAN_POINT('Ctrl Pts',(-1.90602954113646,-1.41150125499576,
6.75060174530038));
#91724=CARTESIAN_POINT('Ctrl Pts',(-1.89428004116471,-1.42723797955601,
6.75191461388151));
#91725=CARTESIAN_POINT('Ctrl Pts',(-1.88803558789786,-1.43548832721985,
6.7526084253377));
#91726=CARTESIAN_POINT('Ctrl Pts',(-1.87126109194202,-1.45735246310538,
6.75446199891347));
#91727=CARTESIAN_POINT('Ctrl Pts',(-1.86063667590849,-1.4708927251605,6.75562547449794));
#91728=CARTESIAN_POINT('Ctrl Pts',(-1.80806454624123,-1.53641206800181,
6.76133316276216));
#91729=CARTESIAN_POINT('Ctrl Pts',(-1.76408500348182,-1.58671421636419,
6.76595864153161));
#91730=CARTESIAN_POINT('Ctrl Pts',(-1.53526695850398,-1.82714125070671,
6.78933744787219));
#91731=CARTESIAN_POINT('Ctrl Pts',(-1.32162701547217,-1.98714714692027,
6.80935726368658));
#91732=CARTESIAN_POINT('Ctrl Pts',(-1.06828962441027,-2.1176288157243,6.82920024445143));
#91733=CARTESIAN_POINT('Ctrl Pts',(-1.05047339873072,-2.12652303705205,
6.83057568674166));
#91734=CARTESIAN_POINT('Ctrl Pts',(-1.02540401877355,-2.13864620889186,
6.83248110157235));
#91735=CARTESIAN_POINT('Ctrl Pts',(-1.01824406944295,-2.14206443137263,
6.8330219151395));
#91736=CARTESIAN_POINT('Ctrl Pts',(-1.00666913296062,-2.14751925617365,
6.83389060392221));
#91737=CARTESIAN_POINT('Ctrl Pts',(-1.00226487962963,-2.14957828679285,
6.83421983795524));
#91738=CARTESIAN_POINT('Ctrl Pts',(-0.992958637941359,-2.15389422395794,
6.83491272332799));
#91739=CARTESIAN_POINT('Ctrl Pts',(-0.988055222932292,-2.15614796852391,
6.83527617110475));
#91740=CARTESIAN_POINT('Ctrl Pts',(-0.975934158987395,-2.16166911176563,
6.83617068610346));
#91741=CARTESIAN_POINT('Ctrl Pts',(-0.96870766621894,-2.16491715623831,
6.83670057680693));
#91742=CARTESIAN_POINT('Ctrl Pts',(-0.941911915999356,-2.17679983183458,
6.83865330086264));
#91743=CARTESIAN_POINT('Ctrl Pts',(-0.922241673575557,-2.18520615517008,
6.84006296698035));
#91744=CARTESIAN_POINT('Ctrl Pts',(-0.784470417845294,-2.24189261026015,
6.84978987182887));
#91745=CARTESIAN_POINT('Ctrl Pts',(-0.662739767213739,-2.28084655128256,
6.85764699279954));
#91746=CARTESIAN_POINT('Ctrl Pts',(-0.359723184962003,-2.35148403114571,
6.87673112956145));
#91747=CARTESIAN_POINT('Ctrl Pts',(-0.176786174264235,-2.37225951021968,
6.88790408119525));
#91748=CARTESIAN_POINT('Ctrl Pts',(0.0355572932765855,-2.37165891632982,
6.90167095604359));
#91749=CARTESIAN_POINT('Ctrl Pts',(0.0644013643421935,-2.37105096579454,
6.90355642784415));
#91750=CARTESIAN_POINT('Ctrl Pts',(0.104622092786952,-2.36946879026094,
6.90621013316511));
#91751=CARTESIAN_POINT('Ctrl Pts',(0.116014453899781,-2.368938321093,6.90696453246844));
#91752=CARTESIAN_POINT('Ctrl Pts',(0.136855224416032,-2.36781720681523,
6.9083498372584));
#91753=CARTESIAN_POINT('Ctrl Pts',(0.146304819695609,-2.36725211429231,
6.9089799315763));
#91754=CARTESIAN_POINT('Ctrl Pts',(0.165433127955941,-2.36599325841199,
6.91025950565679));
#91755=CARTESIAN_POINT('Ctrl Pts',(0.17511146476788,-2.36529663863489,6.91090906323409));
#91756=CARTESIAN_POINT('Ctrl Pts',(0.198975662538783,-2.36343168913475,
6.91251609512297));
#91757=CARTESIAN_POINT('Ctrl Pts',(0.213155646421861,-2.36219502126307,
6.9134756959265));
#91758=CARTESIAN_POINT('Ctrl Pts',(0.265991845461163,-2.35710744658709,
6.91706939030862));
#91759=CARTESIAN_POINT('Ctrl Pts',(0.304560868446427,-2.35243481159841,
6.91972903956202));
#91760=CARTESIAN_POINT('Ctrl Pts',(0.400841287716569,-2.33836308024794,
6.92646380887083));
#91761=CARTESIAN_POINT('Ctrl Pts',(0.458349912665385,-2.32777361970157,
6.93057355323144));
#91762=CARTESIAN_POINT('Ctrl Pts',(0.627024723069871,-2.29022151486651,
6.94288001599588));
#91763=CARTESIAN_POINT('Ctrl Pts',(0.736692836291548,-2.25733343057093,
6.95121871308962));
#91764=CARTESIAN_POINT('Ctrl Pts',(0.961979604805321,-2.17160068591368,
6.96882529350945));
#91765=CARTESIAN_POINT('Ctrl Pts',(1.07661792128258,-2.11711001523005,6.9780689773271));
#91766=CARTESIAN_POINT('Ctrl Pts',(1.20305591776346,-2.04407098286272,6.98822950905937));
#91767=CARTESIAN_POINT('Ctrl Pts',(1.21963181197995,-2.0342241831658,6.98956055951263));
#91768=CARTESIAN_POINT('Ctrl Pts',(1.24276707430886,-2.02009636785497,6.99141498271036));
#91769=CARTESIAN_POINT('Ctrl Pts',(1.24942758321333,-2.01598364455661,6.99194846467697));
#91770=CARTESIAN_POINT('Ctrl Pts',(1.26058359589859,-2.00901851721435,6.9928411933727));
#91771=CARTESIAN_POINT('Ctrl Pts',(1.2650900330684,-2.00618384374638,6.99320157993477));
#91772=CARTESIAN_POINT('Ctrl Pts',(1.27425751000463,-2.000374073935,6.99393419029286));
#91773=CARTESIAN_POINT('Ctrl Pts',(1.27891775038243,-1.99739781386632,6.99430633388162));
#91774=CARTESIAN_POINT('Ctrl Pts',(1.29075395308675,-1.98978022142828,6.9952509275931));
#91775=CARTESIAN_POINT('Ctrl Pts',(1.29791539407534,-1.9851163019975,6.9958218981866));
#91776=CARTESIAN_POINT('Ctrl Pts',(1.32683481353048,-1.96605900346237,6.99812603503372));
#91777=CARTESIAN_POINT('Ctrl Pts',(1.34838082908326,-1.95134515339099,6.99983909475312));
#91778=CARTESIAN_POINT('Ctrl Pts',(1.40456235934286,-1.91160356667001,7.00430885554283));
#91779=CARTESIAN_POINT('Ctrl Pts',(1.43877304190542,-1.88598945031633,7.00703369645474));
#91780=CARTESIAN_POINT('Ctrl Pts',(1.63674022688492,-1.72924415987663,7.0229411833198));
#91781=CARTESIAN_POINT('Ctrl Pts',(1.78320648917726,-1.57777981865735,7.03537571786528));
#91782=CARTESIAN_POINT('Ctrl Pts',(1.94926867088966,-1.35292699177745,7.05300810713387));
#91783=CARTESIAN_POINT('Ctrl Pts',(1.98819469251165,-1.29504447755104,7.05747648546227));
#91784=CARTESIAN_POINT('Ctrl Pts',(2.03387400029331,-1.22019570889695,7.06321779521482));
#91785=CARTESIAN_POINT('Ctrl Pts',(2.04306088069061,-1.2047502751166,7.06440055973187));
#91786=CARTESIAN_POINT('Ctrl Pts',(2.05739453179471,-1.18001632329284,7.06629223144208));
#91787=CARTESIAN_POINT('Ctrl Pts',(2.06265609893493,-1.1707948556351,7.06699697621043));
#91788=CARTESIAN_POINT('Ctrl Pts',(2.07238728835208,-1.1534706828955,7.06832015347643));
#91789=CARTESIAN_POINT('Ctrl Pts',(2.07687176356292,-1.14537651571552,7.06893803753259));
#91790=CARTESIAN_POINT('Ctrl Pts',(2.08679056294257,-1.12722398364047,7.07032312615786));
#91791=CARTESIAN_POINT('Ctrl Pts',(2.09219972749352,-1.11715220771192,7.07109120879116));
#91792=CARTESIAN_POINT('Ctrl Pts',(2.10794604700161,-1.0873173211394,7.07336544443912));
#91793=CARTESIAN_POINT('Ctrl Pts',(2.11807724541879,-1.0674475242442,7.07487879529841));
#91794=CARTESIAN_POINT('Ctrl Pts',(2.19569824967337,-0.909756352348034,
7.08688272446702));
#91795=CARTESIAN_POINT('Ctrl Pts',(2.24993485982392,-0.765848593577822,
7.09783554292199));
#91796=CARTESIAN_POINT('Ctrl Pts',(2.33495520448039,-0.450687575349145,
7.12159359029764));
#91797=CARTESIAN_POINT('Ctrl Pts',(2.36160806942126,-0.279196776185002,
7.13438916012477));
#91798=CARTESIAN_POINT('Ctrl Pts',(2.37013316012776,-0.0892189002088124,
7.14758966101635));
#91799=CARTESIAN_POINT('Ctrl Pts',(2.37071549403491,-0.0721061564834831,
7.14876970703295));
#91800=CARTESIAN_POINT('Ctrl Pts',(2.37126861349832,-0.0482553432358436,
7.15040046377114));
#91801=CARTESIAN_POINT('Ctrl Pts',(2.37139607531557,-0.0415219496452577,
7.15085930146506));
#91802=CARTESIAN_POINT('Ctrl Pts',(2.3715664709993,-0.0299060913625083,
7.15164807682085));
#91803=CARTESIAN_POINT('Ctrl Pts',(2.3716230108178,-0.0250239153481056,
7.15197875693282));
#91804=CARTESIAN_POINT('Ctrl Pts',(2.37171011657951,-0.014767221435175,
7.15267164218714));
#91805=CARTESIAN_POINT('Ctrl Pts',(2.37173749087287,-0.00939272184908155,
7.15303365792538));
#91806=CARTESIAN_POINT('Ctrl Pts',(2.37175983439651,0.00379579987885965,
7.15391952011867));
#91807=CARTESIAN_POINT('Ctrl Pts',(2.37173445711543,0.0116098851496699,
7.15444224112882));
#91808=CARTESIAN_POINT('Ctrl Pts',(2.3715013737321,0.0400695999226933,7.15633870050681));
#91809=CARTESIAN_POINT('Ctrl Pts',(2.37106269939108,0.0607131454763198,
7.1577002384941));
#91810=CARTESIAN_POINT('Ctrl Pts',(2.36929020506543,0.112360122897574,7.16107726098657));
#91811=CARTESIAN_POINT('Ctrl Pts',(2.36761740900082,0.143348785695668,7.16307703502416));
#91812=CARTESIAN_POINT('Ctrl Pts',(2.35767504763082,0.278273669383143,7.17170311819737));
#91813=CARTESIAN_POINT('Ctrl Pts',(2.34316492297942,0.381640660970419,7.17810526922334));
#91814=CARTESIAN_POINT('Ctrl Pts',(2.28596083380586,0.656222713460131,7.19529894857697));
#91815=CARTESIAN_POINT('Ctrl Pts',(2.23091940197626,0.824156845293147,7.20605719407641));
#91816=CARTESIAN_POINT('Ctrl Pts',(2.14591089768657,1.01048709659728,7.21933111514027));
#91817=CARTESIAN_POINT('Ctrl Pts',(2.13355715005715,1.03631632483864,7.22120155455864));
#91818=CARTESIAN_POINT('Ctrl Pts',(2.11550987449121,1.07235835889184,7.22385773805628));
#91819=CARTESIAN_POINT('Ctrl Pts',(2.11020345435234,1.08276306363527,7.22463003394501));
#91820=CARTESIAN_POINT('Ctrl Pts',(2.10082351689131,1.10082415487385,7.22598046302871));
#91821=CARTESIAN_POINT('Ctrl Pts',(2.09678442025638,1.10849824565853,7.22655737815117));
#91822=CARTESIAN_POINT('Ctrl Pts',(2.08823957142258,1.12451924208615,7.22776843793311));
#91823=CARTESIAN_POINT('Ctrl Pts',(2.08372566054862,1.13286159813459,7.22840286422378));
#91824=CARTESIAN_POINT('Ctrl Pts',(2.0728515061733,1.15267371864003,7.2299187837567));
#91825=CARTESIAN_POINT('Ctrl Pts',(2.0664459846036,1.16411814218372,7.2308018835259));
#91826=CARTESIAN_POINT('Ctrl Pts',(2.04434938040251,1.20283994228793,7.23381559564766));
#91827=CARTESIAN_POINT('Ctrl Pts',(2.02821106694831,1.22985690943136,7.2359622375485));
#91828=CARTESIAN_POINT('Ctrl Pts',(1.98815075427778,1.29398754633503,7.24116700866976));
#91829=CARTESIAN_POINT('Ctrl Pts',(1.96372129336663,1.33076873943882,7.24424286206683));
#91830=CARTESIAN_POINT('Ctrl Pts',(1.78483514075512,1.58444173963456,7.26610763197226));
#91831=CARTESIAN_POINT('Ctrl Pts',(1.5958842059277,1.77460063579503,7.28622068216769));
#91832=CARTESIAN_POINT('Ctrl Pts',(1.36384643705875,1.94048545157253,7.30606342928434));
#91833=CARTESIAN_POINT('Ctrl Pts',(1.34821739987404,1.95137664027384,7.30737832266372));
#91834=CARTESIAN_POINT('Ctrl Pts',(1.32601429871494,1.96645488550723,7.30921419815238));
#91835=CARTESIAN_POINT('Ctrl Pts',(1.31954872931874,1.97079930293002,7.30974502840509));
#91836=CARTESIAN_POINT('Ctrl Pts',(1.30863461214616,1.97805504886825,7.31063459479104));
#91837=CARTESIAN_POINT('Ctrl Pts',(1.30419750845687,1.98098338846003,7.31099445323348));
#91838=CARTESIAN_POINT('Ctrl Pts',(1.29511649541476,1.98693281646046,7.31172723116024));
#91839=CARTESIAN_POINT('Ctrl Pts',(1.29047179064321,1.98995259063937,7.31210006360233));
#91840=CARTESIAN_POINT('Ctrl Pts',(1.27859498283242,1.99761527587033,7.31304853541022));
#91841=CARTESIAN_POINT('Ctrl Pts',(1.27134806854374,2.00223525462293,7.31362267109997));
#91842=CARTESIAN_POINT('Ctrl Pts',(1.24166682895499,2.02093121261976,7.31595616055643));
#91843=CARTESIAN_POINT('Ctrl Pts',(1.21902156079035,2.03467099580191,7.31769475691884));
#91844=CARTESIAN_POINT('Ctrl Pts',(1.01342440518146,2.15474983690623,7.33315290616915));
#91845=CARTESIAN_POINT('Ctrl Pts',(0.817214979028365,2.23655133959443,7.34567959061039));
#91846=CARTESIAN_POINT('Ctrl Pts',(0.50997285230316,2.318715177038,7.36541781445755));
#91847=CARTESIAN_POINT('Ctrl Pts',(0.405495383277972,2.33924805596278,7.37213596680569));
#91848=CARTESIAN_POINT('Ctrl Pts',(0.281857636864072,2.35501356429138,7.38027881608126));
#91849=CARTESIAN_POINT('Ctrl Pts',(0.263688036992343,2.35711713832055,7.38148006405105));
#91850=CARTESIAN_POINT('Ctrl Pts',(0.233899104598512,2.36021719841683,7.38345785203343));
#91851=CARTESIAN_POINT('Ctrl Pts',(0.222293311896435,2.36133853779836,7.38423046803939));
#91852=CARTESIAN_POINT('Ctrl Pts',(0.201444213349857,2.3631978900725,7.38562234298475));
#91853=CARTESIAN_POINT('Ctrl Pts',(0.192203894770174,2.36396736385486,7.38624060068705));
#91854=CARTESIAN_POINT('Ctrl Pts',(0.172529042038899,2.36548963981481,7.38756006212258));
#91855=CARTESIAN_POINT('Ctrl Pts',(0.162093593333101,2.36622762373575,7.38826171749581));
#91856=CARTESIAN_POINT('Ctrl Pts',(0.133958040174383,2.36803034810612,7.39015856236435));
#91857=CARTESIAN_POINT('Ctrl Pts',(0.116250607923798,2.36896565032319,7.39135777627514));
#91858=CARTESIAN_POINT('Ctrl Pts',(0.0249594232379776,2.3727616357525,7.39756953796162));
#91859=CARTESIAN_POINT('Ctrl Pts',(-0.0487106889193495,2.37239245720335,
7.40268178308466));
#91860=CARTESIAN_POINT('Ctrl Pts',(-0.208153470922428,2.36416398570984,
7.41396903815144));
#91861=CARTESIAN_POINT('Ctrl Pts',(-0.293757029317236,2.35505917650116,
7.42017060640061));
#91862=CARTESIAN_POINT('Ctrl Pts',(-0.444638027794583,2.33065670333367,
7.43129146736727));
#91863=CARTESIAN_POINT('Ctrl Pts',(-0.51012502524503,2.31720433865143,7.43618245951646));
#91864=CARTESIAN_POINT('Ctrl Pts',(-0.686168998494371,2.27321596242966,
7.44941510043279));
#91865=CARTESIAN_POINT('Ctrl Pts',(-0.795236002910107,2.23739692145749,
7.45771024258265));
#91866=CARTESIAN_POINT('Ctrl Pts',(-0.913069957599856,2.18898683195156,
7.46650067311795));
#91867=CARTESIAN_POINT('Ctrl Pts',(-0.924805530854167,2.18405468020414,
7.46737410677108));
#91868=CARTESIAN_POINT('Ctrl Pts',(-0.942489636805805,2.17645441787358,
7.4686865581843));
#91869=CARTESIAN_POINT('Ctrl Pts',(-0.948467581317756,2.17385597460957,
7.4691295745721));
#91870=CARTESIAN_POINT('Ctrl Pts',(-0.959182051804963,2.16914608655972,
7.46992234808808));
#91871=CARTESIAN_POINT('Ctrl Pts',(-0.963922412205101,2.16704373242484,
7.47027264005255));
#91872=CARTESIAN_POINT('Ctrl Pts',(-0.96867547128321,2.16491706406728,7.47062341409115));
#91873=CARTESIAN_POINT('Ctrl Pts',(-0.968694951178242,2.16490834783305,
7.47062485169279));
#91874=CARTESIAN_POINT('Ctrl Pts',(-0.968733628915929,2.16489104094172,
7.47062770606584));
#91875=CARTESIAN_POINT('Ctrl Pts',(-0.968752826773134,2.16488245028718,
7.47062912283853));
#91876=CARTESIAN_POINT('Ctrl Pts',(-0.968790945158034,2.16486539246889,
7.47063193590286));
#91877=CARTESIAN_POINT('Ctrl Pts',(-0.968809865627772,2.16485692533987,
7.47063333219043));
#91878=CARTESIAN_POINT('Ctrl Pts',(-0.968847433653024,2.16484011262295,
7.47063610461099));
#91879=CARTESIAN_POINT('Ctrl Pts',(-0.968866081234489,2.16483176703196,
7.4706374807461));
#91880=CARTESIAN_POINT('Ctrl Pts',(-0.96890310781857,2.16481519547627,7.47064021318229));
#91881=CARTESIAN_POINT('Ctrl Pts',(-0.968921486890057,2.16480696948902,
7.47064156948864));
#91882=CARTESIAN_POINT('Ctrl Pts',(-0.968957980969866,2.16479063514436,
7.47064426260116));
#91883=CARTESIAN_POINT('Ctrl Pts',(-0.968976095937338,2.16478252681324,
7.47064559940449));
#91884=CARTESIAN_POINT('Ctrl Pts',(-0.969012065982602,2.16476642593671,
7.47064825381953));
#91885=CARTESIAN_POINT('Ctrl Pts',(-0.969029921085812,2.16475843338769,
7.47064957143328));
#91886=CARTESIAN_POINT('Ctrl Pts',(-0.969065375594583,2.16474256222202,
7.47065218777907));
#91887=CARTESIAN_POINT('Ctrl Pts',(-0.969082975010155,2.16473468360843,
7.47065348651202));
#91888=CARTESIAN_POINT('Ctrl Pts',(-0.969117922355154,2.16471903845079,
7.47065606540751));
#91889=CARTESIAN_POINT('Ctrl Pts',(-0.969135270244155,2.16471127193214,
7.47065734556724));
#91890=CARTESIAN_POINT('Ctrl Pts',(-0.969169718411262,2.16469584925127,
7.47065988760279));
#91891=CARTESIAN_POINT('Ctrl Pts',(-0.969186818747928,2.16468819306992,
7.4706611494831));
#91892=CARTESIAN_POINT('Ctrl Pts',(-0.969220775905205,2.16467298925146,
7.47066365526249));
#91893=CARTESIAN_POINT('Ctrl Pts',(-0.969237632698956,2.16466544163324,
7.47066489915975));
#91894=CARTESIAN_POINT('Ctrl Pts',(-0.969271106567646,2.16465045326136,
7.47066736925373));
#91895=CARTESIAN_POINT('Ctrl Pts',(-0.969287723673151,2.16464301250068,
7.47066859545286));
#91896=CARTESIAN_POINT('Ctrl Pts',(-0.969320722029739,2.16462823613338,
7.47067103043623));
#91897=CARTESIAN_POINT('Ctrl Pts',(-0.969337103265034,2.1646209005403,7.47067223921946));
#91898=CARTESIAN_POINT('Ctrl Pts',(-0.96936963373478,2.16460633280188,7.47067463965583));
#91899=CARTESIAN_POINT('Ctrl Pts',(-0.969385782906217,2.16459910069103,
7.47067583130448));
#91900=CARTESIAN_POINT('Ctrl Pts',(-0.969417852722957,2.1645847383797,7.47067819772855));
#91901=CARTESIAN_POINT('Ctrl Pts',(-0.969433773430796,2.16457760815732,
7.47067937250873));
#91902=CARTESIAN_POINT('Ctrl Pts',(-0.969465390112604,2.1645634479427,7.47068170547613));
#91903=CARTESIAN_POINT('Ctrl Pts',(-0.969481086033776,2.16455641798003,
7.47068286365958));
#91904=CARTESIAN_POINT('Ctrl Pts',(-0.969512256604615,2.16454245675176,
7.47068516368945));
#91905=CARTESIAN_POINT('Ctrl Pts',(-0.969527731275321,2.16453552548246,
7.47068630553754));
#91906=CARTESIAN_POINT('Ctrl Pts',(-0.969558974099726,2.16452153108746,
7.47068861087973));
#91907=CARTESIAN_POINT('Ctrl Pts',(-0.969574742306731,2.16451446793025,
7.47068977437758));
#91908=CARTESIAN_POINT('Ctrl Pts',(-0.969606231288884,2.16450036244915,
7.47069209786356));
#91909=CARTESIAN_POINT('Ctrl Pts',(-0.969621951977121,2.16449332016544,
7.47069325784531));
#91910=CARTESIAN_POINT('Ctrl Pts',(-0.969653346075856,2.16447925636603,
7.47069557431056));
#91911=CARTESIAN_POINT('Ctrl Pts',(-0.969669019503406,2.16447223484393,
7.47069673079534));
#91912=CARTESIAN_POINT('Ctrl Pts',(-0.969700319320073,2.16445821246421,
7.47069904028441));
#91913=CARTESIAN_POINT('Ctrl Pts',(-0.969715945747083,2.16445121159084,
7.47070019329151));
#91914=CARTESIAN_POINT('Ctrl Pts',(-0.969747151920878,2.16443723035176,
7.47070249585174));
#91915=CARTESIAN_POINT('Ctrl Pts',(-0.969762731654559,2.16443024999313,
7.47070364540392));
#91916=CARTESIAN_POINT('Ctrl Pts',(-0.96979384469873,2.16441630967201,7.47070594107336));
#91917=CARTESIAN_POINT('Ctrl Pts',(-0.969809378019336,2.16440934970617,
7.47070708719139));
#91918=CARTESIAN_POINT('Ctrl Pts',(-0.969840398475935,2.16439545006731,
7.4707093760102));
#91919=CARTESIAN_POINT('Ctrl Pts',(-0.969855885643577,2.16438851038129,
7.47071051871336));
#91920=CARTESIAN_POINT('Ctrl Pts',(-0.969886814101103,2.16437465116812,
7.47071280072515));
#91921=CARTESIAN_POINT('Ctrl Pts',(-0.969902255387046,2.16436773164392,
7.47071394003353));
#91922=CARTESIAN_POINT('Ctrl Pts',(-0.969933092459339,2.16435391258844,
7.47071621528377));
#91923=CARTESIAN_POINT('Ctrl Pts',(-0.969948488187533,2.1643470130844,7.47071735122136));
#91924=CARTESIAN_POINT('Ctrl Pts',(-0.969979234282175,2.16433323401096,
7.47071961974028));
#91925=CARTESIAN_POINT('Ctrl Pts',(-0.969994584680246,2.16432635442855,
7.47072075232397));
#91926=CARTESIAN_POINT('Ctrl Pts',(-0.970025240459214,2.16431261504741,
7.47072301416059));
#91927=CARTESIAN_POINT('Ctrl Pts',(-0.970040545821809,2.16430575525803,
7.4707241434122));
#91928=CARTESIAN_POINT('Ctrl Pts',(-0.97007111179331,2.1642920553483,7.47072639860418));
#91929=CARTESIAN_POINT('Ctrl Pts',(-0.970086372399844,2.16428521523014,
7.47072752454441));
#91930=CARTESIAN_POINT('Ctrl Pts',(-0.970116849044107,2.16427155458339,
7.47072977312735));
#91931=CARTESIAN_POINT('Ctrl Pts',(-0.970132065120514,2.16426473403857,
7.47073089577295));
#91932=CARTESIAN_POINT('Ctrl Pts',(-0.975890890559293,2.16168329085297,
7.4711557815007));
#91933=CARTESIAN_POINT('Ctrl Pts',(-0.981624312343408,2.15908577688989,
7.47157814153987));
#91934=CARTESIAN_POINT('Ctrl Pts',(-0.998369713610735,2.15141881950578,
7.47280999994709));
#91935=CARTESIAN_POINT('Ctrl Pts',(-1.00935345471363,2.14628764170618,7.47361583151524));
#91936=CARTESIAN_POINT('Ctrl Pts',(-1.03453348052094,2.1342884575082,7.47545926161316));
#91937=CARTESIAN_POINT('Ctrl Pts',(-1.04870173042696,2.1273625580462,7.47649362354299));
#91938=CARTESIAN_POINT('Ctrl Pts',(-1.20186067440457,2.05059148676722,7.48765488850947));
#91939=CARTESIAN_POINT('Ctrl Pts',(-1.33374647243368,1.96736585007179,7.49710094675346));
#91940=CARTESIAN_POINT('Ctrl Pts',(-1.57626001286983,1.77865467242176,7.51593822353582));
#91941=CARTESIAN_POINT('Ctrl Pts',(-1.68674752221328,1.67424096733691,7.52528955580757));
#91942=CARTESIAN_POINT('Ctrl Pts',(-1.80566593341802,1.53805636379962,7.53700254907519));
#91943=CARTESIAN_POINT('Ctrl Pts',(-1.82442178815007,1.51576114831558,7.53890532760568));
#91944=CARTESIAN_POINT('Ctrl Pts',(-1.85016868956254,1.4839852819524,7.54159998222408));
#91945=CARTESIAN_POINT('Ctrl Pts',(-1.85750757462526,1.47478883189998,7.54237787851772));
#91946=CARTESIAN_POINT('Ctrl Pts',(-1.87014944143273,1.45870309031739,7.54373530864932));
#91947=CARTESIAN_POINT('Ctrl Pts',(-1.87548357993214,1.45183848170299,7.54431359192015));
#91948=CARTESIAN_POINT('Ctrl Pts',(-1.88654756158331,1.43743729941374,7.54552477550449));
#91949=CARTESIAN_POINT('Ctrl Pts',(-1.89227024922733,1.42989544766634,7.54615794336183));
#91950=CARTESIAN_POINT('Ctrl Pts',(-1.90575234386216,1.41190490034321,7.54766578293109));
#91951=CARTESIAN_POINT('Ctrl Pts',(-1.91347113405706,1.4014262917159,7.54854201620449));
#91952=CARTESIAN_POINT('Ctrl Pts',(-1.93920219614779,1.36588630856477,7.55150756280816));
#91953=CARTESIAN_POINT('Ctrl Pts',(-1.95681077813004,1.34053794697499,7.55361221960913));
#91954=CARTESIAN_POINT('Ctrl Pts',(-2.02043138975053,1.24502778759721,7.56150767920599));
#91955=CARTESIAN_POINT('Ctrl Pts',(-2.06320064658656,1.1727904492665,7.56741410073814));
#91956=CARTESIAN_POINT('Ctrl Pts',(-2.1362946858041,1.03291352832711,7.57871912391117));
#91957=CARTESIAN_POINT('Ctrl Pts',(-2.16745445830077,0.965818513013279,
7.58408824787615));
#91958=CARTESIAN_POINT('Ctrl Pts',(-2.22509976008393,0.824790273751776,
7.59520399922622));
#91959=CARTESIAN_POINT('Ctrl Pts',(-2.25115318195857,0.750771356717332,
7.60094729694803));
#91960=CARTESIAN_POINT('Ctrl Pts',(-2.29750938951388,0.594775286730919,
7.61273704543889));
#91961=CARTESIAN_POINT('Ctrl Pts',(-2.31720265793425,0.51272039465409,7.61876580320549));
#91962=CARTESIAN_POINT('Ctrl Pts',(-2.33475443212655,0.417464582372106,
7.62544747915636));
#91963=CARTESIAN_POINT('Ctrl Pts',(-2.33692651305717,0.405128900106705,
7.62630669642189));
#91964=CARTESIAN_POINT('Ctrl Pts',(-2.34007301325301,0.386391345390974,
7.62760205377453));
#91965=CARTESIAN_POINT('Ctrl Pts',(-2.34111906580965,0.380001975506996,
7.62804204273221));
#91966=CARTESIAN_POINT('Ctrl Pts',(-2.34295550212509,0.368489412840857,
7.628831638922));
#91967=CARTESIAN_POINT('Ctrl Pts',(-2.34375526114331,0.363367871113592,
7.62918176122784));
#91968=CARTESIAN_POINT('Ctrl Pts',(-2.3452845483387,0.35335939506694,7.62986373736462));
#91969=CARTESIAN_POINT('Ctrl Pts',(-2.34601559299617,0.348472830088667,
7.63019567854787));
#91970=CARTESIAN_POINT('Ctrl Pts',(-2.34762075728033,0.337509310768287,
7.63093819007921));
#91971=CARTESIAN_POINT('Ctrl Pts',(-2.34848656618602,0.331431147298305,
7.63134830091514));
#91972=CARTESIAN_POINT('Ctrl Pts',(-2.35060748290207,0.316116142845398,
7.63237793594942));
#91973=CARTESIAN_POINT('Ctrl Pts',(-2.3518317696138,0.306875037714167,7.63299582431652));
#91974=CARTESIAN_POINT('Ctrl Pts',(-2.35823918987495,0.256218741601184,
7.63636546432904));
#91975=CARTESIAN_POINT('Ctrl Pts',(-2.36238186104507,0.214687524790751,
7.63906453097502));
#91976=CARTESIAN_POINT('Ctrl Pts',(-2.36542649614281,0.173076728203254,
7.64172477676247));
#91977=CARTESIAN_POINT('Origin',(0.,0.,-1.84858989190503));
#91978=CARTESIAN_POINT('',(-2.36542648836857,0.173076834453233,8.83818724301668));
#91979=CARTESIAN_POINT('',(-2.36542651242649,0.173076505655319,8.63818628587103));
#91980=CARTESIAN_POINT('',(-2.36542649454111,0.173076750093529,-1.84858989190503));
#91981=CARTESIAN_POINT('',(-2.37174984266889,0.000863886614090527,7.85072532400096));
#91982=CARTESIAN_POINT('Ctrl Pts',(-2.36542648836857,0.173076834453233,
8.83818724301668));
#91983=CARTESIAN_POINT('Ctrl Pts',(-2.35876889342097,0.264065622684951,
8.83249593822389));
#91984=CARTESIAN_POINT('Ctrl Pts',(-2.34686578487537,0.354611150249955,
8.82670376988962));
#91985=CARTESIAN_POINT('Ctrl Pts',(-2.32629063658811,0.462509364048279,
8.81953001257228));
#91986=CARTESIAN_POINT('Ctrl Pts',(-2.32259742656982,0.480712179483354,
8.81831050730852));
#91987=CARTESIAN_POINT('Ctrl Pts',(-2.31623859978643,0.510267321550908,
8.81631444510768));
#91988=CARTESIAN_POINT('Ctrl Pts',(-2.3137023336149,0.5216469052677,8.81554202140753));
#91989=CARTESIAN_POINT('Ctrl Pts',(-2.30902450150786,0.541929662981707,
8.81415811915313));
#91990=CARTESIAN_POINT('Ctrl Pts',(-2.3069150664522,0.550840067815803,8.81354768413038));
#91991=CARTESIAN_POINT('Ctrl Pts',(-2.30234449119464,0.569659682490639,
8.81225304335078));
#91992=CARTESIAN_POINT('Ctrl Pts',(-2.29987086093921,0.579565636772957,
8.81156844553908));
#91993=CARTESIAN_POINT('Ctrl Pts',(-2.29310521796342,0.605933947780758,
8.80973757438763));
#91994=CARTESIAN_POINT('Ctrl Pts',(-2.28869997504526,0.622366361225135,
8.80858766082402));
#91995=CARTESIAN_POINT('Ctrl Pts',(-2.26626953676803,0.702575848602684,
8.80292974437382));
#91996=CARTESIAN_POINT('Ctrl Pts',(-2.2457549291516,0.765619830370065,8.79834157775914));
#91997=CARTESIAN_POINT('Ctrl Pts',(-2.13286566276937,1.06875600474037,8.77556502443014));
#91998=CARTESIAN_POINT('Ctrl Pts',(-2.00451654065907,1.29353476881524,8.75619300901502));
#91999=CARTESIAN_POINT('Ctrl Pts',(-1.82575394459939,1.51411287992846,8.7362863785228));
#92000=CARTESIAN_POINT('Ctrl Pts',(-1.80853997549951,1.53463304732701,8.73442714537895));
#92001=CARTESIAN_POINT('Ctrl Pts',(-1.78517098548093,1.56155088444538,8.73198324857461));
#92002=CARTESIAN_POINT('Ctrl Pts',(-1.77932316163247,1.56821098865054,8.73137815513024));
#92003=CARTESIAN_POINT('Ctrl Pts',(-1.76975442316424,1.5789864217645,8.7303987134258));
#92004=CARTESIAN_POINT('Ctrl Pts',(-1.76605623044131,1.58312167282589,8.73002272594953));
#92005=CARTESIAN_POINT('Ctrl Pts',(-1.7588332155937,1.59114150698706,8.72929339289365));
#92006=CARTESIAN_POINT('Ctrl Pts',(-1.75530998635767,1.59502740664373,8.72893994248078));
#92007=CARTESIAN_POINT('Ctrl Pts',(-1.74676597404571,1.60438831873584,8.72808826386245));
#92008=CARTESIAN_POINT('Ctrl Pts',(-1.74173224656889,1.60985155539242,8.7275910062397));
#92009=CARTESIAN_POINT('Ctrl Pts',(-1.72403117362975,1.62888278259217,8.72585772063192));
#92010=CARTESIAN_POINT('Ctrl Pts',(-1.71122988842416,1.64232607273957,8.72463141666329));
#92011=CARTESIAN_POINT('Ctrl Pts',(-1.63161718176271,1.72398982781426,8.71715937238237));
#92012=CARTESIAN_POINT('Ctrl Pts',(-1.56088621668562,1.78828246408518,8.71117651172074));
#92013=CARTESIAN_POINT('Ctrl Pts',(-1.42878393351868,1.89453254393126,8.70070126151164));
#92014=CARTESIAN_POINT('Ctrl Pts',(-1.3689638637378,1.93819900896571,8.69618242963897));
#92015=CARTESIAN_POINT('Ctrl Pts',(-1.17525104806262,2.06615330351451,8.6819439599089));
#92016=CARTESIAN_POINT('Ctrl Pts',(-1.03493810967471,2.13988258034999,8.67215654690258));
#92017=CARTESIAN_POINT('Ctrl Pts',(-0.870985476867069,2.20611261868149,
8.66061009057379));
#92018=CARTESIAN_POINT('Ctrl Pts',(-0.853544047491532,2.21291913841129,
8.65938096467967));
#92019=CARTESIAN_POINT('Ctrl Pts',(-0.825071909566361,2.22364371690574,
8.65737227909002));
#92020=CARTESIAN_POINT('Ctrl Pts',(-0.814089336649769,2.2276879447796,8.65659694110482));
#92021=CARTESIAN_POINT('Ctrl Pts',(-0.794456834981467,2.23475285846302,
8.65520979757175));
#92022=CARTESIAN_POINT('Ctrl Pts',(-0.785818426973752,2.23780503995142,
8.65459905440992));
#92023=CARTESIAN_POINT('Ctrl Pts',(-0.767540112934206,2.24414437336899,
8.65330582884267));
#92024=CARTESIAN_POINT('Ctrl Pts',(-0.757896306951808,2.24741962609871,
8.65262296643389));
#92025=CARTESIAN_POINT('Ctrl Pts',(-0.732197274724079,2.25596337235392,
8.65080165307633));
#92026=CARTESIAN_POINT('Ctrl Pts',(-0.716106579494251,2.26112249280876,
8.64965962853309));
#92027=CARTESIAN_POINT('Ctrl Pts',(-0.637987453753924,2.28525215939675,
8.64410608392915));
#92028=CARTESIAN_POINT('Ctrl Pts',(-0.575259000557079,2.30184297636762,
8.63961793987635));
#92029=CARTESIAN_POINT('Ctrl Pts',(-0.279153485851427,2.36729937622403,
8.61828198487702));
#92030=CARTESIAN_POINT('Ctrl Pts',(-0.0399982439119246,2.38335918752959,
8.60043946926061));
#92031=CARTESIAN_POINT('Ctrl Pts',(0.241216999428088,2.35985938088234,8.5803867455497));
#92032=CARTESIAN_POINT('Ctrl Pts',(0.284820498405838,2.35499465639849,8.57731028643348));
#92033=CARTESIAN_POINT('Ctrl Pts',(0.338629641142923,2.34747470812399,8.57357408241161));
#92034=CARTESIAN_POINT('Ctrl Pts',(0.348982594264789,2.34595794896039,8.57285801840938));
#92035=CARTESIAN_POINT('Ctrl Pts',(0.365220566769256,2.34346913130864,8.57173964947988));
#92036=CARTESIAN_POINT('Ctrl Pts',(0.371112377254393,2.34254332665123,8.5713348393428));
#92037=CARTESIAN_POINT('Ctrl Pts',(0.382057495152985,2.34078114456698,8.57058473251952));
#92038=CARTESIAN_POINT('Ctrl Pts',(0.387111544944955,2.33995062959239,8.5702391253836));
#92039=CARTESIAN_POINT('Ctrl Pts',(0.398648027104586,2.33801647778497,8.56945194466544));
#92040=CARTESIAN_POINT('Ctrl Pts',(0.405128582778107,2.33690225169225,8.56901097549462));
#92041=CARTESIAN_POINT('Ctrl Pts',(0.425115921310742,2.33338011110503,8.56765448665391));
#92042=CARTESIAN_POINT('Ctrl Pts',(0.438606809088545,2.33088188862414,8.56674390393655));
#92043=CARTESIAN_POINT('Ctrl Pts',(0.567195089944457,2.30591411662454,8.55810596860091));
#92044=CARTESIAN_POINT('Ctrl Pts',(0.680515752676439,2.27505086800216,8.55080612054963));
#92045=CARTESIAN_POINT('Ctrl Pts',(0.98799911929464,2.16625893379207,8.53073319167251));
#92046=CARTESIAN_POINT('Ctrl Pts',(1.17480939033113,2.07090186645032,8.51814212041526));
#92047=CARTESIAN_POINT('Ctrl Pts',(1.3683783238774,1.93737744295705,8.50286380845404));
#92048=CARTESIAN_POINT('Ctrl Pts',(1.38978954523985,1.92207583697046,8.50114130932855));
#92049=CARTESIAN_POINT('Ctrl Pts',(1.42057046738588,1.89929490219257,8.49861480063135));
#92050=CARTESIAN_POINT('Ctrl Pts',(1.43014559536455,1.89209543772177,8.49782163396893));
#92051=CARTESIAN_POINT('Ctrl Pts',(1.44699769638005,1.87922347067598,8.49641256373866));
#92052=CARTESIAN_POINT('Ctrl Pts',(1.45429693751029,1.87358042247481,8.49579782838899));
#92053=CARTESIAN_POINT('Ctrl Pts',(1.46939857081102,1.86176391876256,8.49451665440732));
#92054=CARTESIAN_POINT('Ctrl Pts',(1.47719540021764,1.85558367999035,8.4938499530639));
#92055=CARTESIAN_POINT('Ctrl Pts',(1.49729287859935,1.83944626087682,8.4921176334833));
#92056=CARTESIAN_POINT('Ctrl Pts',(1.50953299652158,1.82941483052731,8.49104903856798));
#92057=CARTESIAN_POINT('Ctrl Pts',(1.56250548174605,1.78510745215525,8.48636397954637));
#92058=CARTESIAN_POINT('Ctrl Pts',(1.6021748125262,1.74959054456431,8.48269701622513));
#92059=CARTESIAN_POINT('Ctrl Pts',(1.70704027012669,1.64914303044285,8.47255037412201));
#92060=CARTESIAN_POINT('Ctrl Pts',(1.76970252691558,1.58171075697425,8.46597227153812));
#92061=CARTESIAN_POINT('Ctrl Pts',(1.91170094895162,1.40987415689578,8.44981530758467));
#92062=CARTESIAN_POINT('Ctrl Pts',(1.98661126025481,1.30219848747345,8.44016550861144));
#92063=CARTESIAN_POINT('Ctrl Pts',(2.05906393767271,1.17713145764383,8.42974857155937));
#92064=CARTESIAN_POINT('Ctrl Pts',(2.06577544222655,1.16531309167152,8.42877172448446));
#92065=CARTESIAN_POINT('Ctrl Pts',(2.10036778901294,1.10316090489159,8.42367586822666));
#92066=CARTESIAN_POINT('Ctrl Pts',(2.12651441470661,1.05187762720501,8.41961165031398));
#92067=CARTESIAN_POINT('Ctrl Pts',(2.15513346251164,0.990305459410694,8.41493595426291));
#92068=CARTESIAN_POINT('Ctrl Pts',(2.15943378223277,0.980892906555262,8.41422668229754));
#92069=CARTESIAN_POINT('Ctrl Pts',(2.16633105318418,0.96553092199153,8.41307838007262));
#92070=CARTESIAN_POINT('Ctrl Pts',(2.16896537157686,0.959598568553732,8.41263717656038));
#92071=CARTESIAN_POINT('Ctrl Pts',(2.17363214511731,0.9489718259161,8.41185093082263));
#92072=CARTESIAN_POINT('Ctrl Pts',(2.17567379245244,0.944281620699652,8.41150533877518));
#92073=CARTESIAN_POINT('Ctrl Pts',(2.18008747530667,0.934051911191164,8.41075468265436));
#92074=CARTESIAN_POINT('Ctrl Pts',(2.18245357690786,0.928509967358067,8.41034997935679));
#92075=CARTESIAN_POINT('Ctrl Pts',(2.18909317251914,0.912792932091501,8.40920762206317));
#92076=CARTESIAN_POINT('Ctrl Pts',(2.19331687699893,0.902596778058855,8.40847290886138));
#92077=CARTESIAN_POINT('Ctrl Pts',(2.22000570597938,0.836875383718948,8.40377567745109));
#92078=CARTESIAN_POINT('Ctrl Pts',(2.24043396472986,0.780540077435654,8.39992512984583));
#92079=CARTESIAN_POINT('Ctrl Pts',(2.3128200488446,0.554552274222488,8.38493956171926));
#92080=CARTESIAN_POINT('Ctrl Pts',(2.3478113708967,0.380072681827114,8.3743378858184));
#92081=CARTESIAN_POINT('Ctrl Pts',(2.37186095108942,0.100554209268612,8.35690583426247));
#92082=CARTESIAN_POINT('Ctrl Pts',(2.37398912139002,-0.00265914512425559,
8.35038293476816));
#92083=CARTESIAN_POINT('Ctrl Pts',(2.36859164943295,-0.123678800109922,
8.3424665500662));
#92084=CARTESIAN_POINT('Ctrl Pts',(2.36758351739713,-0.141672530689988,
8.34128272957081));
#92085=CARTESIAN_POINT('Ctrl Pts',(2.36559687395829,-0.171118550420209,
8.33933354068602));
#92086=CARTESIAN_POINT('Ctrl Pts',(2.36473998606553,-0.182578527741134,
8.33857198474456));
#92087=CARTESIAN_POINT('Ctrl Pts',(2.36305216669293,-0.203140467344562,
8.33720005823731));
#92088=CARTESIAN_POINT('Ctrl Pts',(2.36225183797834,-0.212244768903336,
8.33659066098494));
#92089=CARTESIAN_POINT('Ctrl Pts',(2.36043664863537,-0.231610028606325,
8.33529020313934));
#92090=CARTESIAN_POINT('Ctrl Pts',(2.35940745846572,-0.24186942070689,8.3345987033529));
#92091=CARTESIAN_POINT('Ctrl Pts',(2.35645420963427,-0.269493707664435,
8.33272976843025));
#92092=CARTESIAN_POINT('Ctrl Pts',(2.35440515101737,-0.286844307729571,
8.33154842272809));
#92093=CARTESIAN_POINT('Ctrl Pts',(2.34289546637464,-0.375849296777698,
8.32544862964116));
#92094=CARTESIAN_POINT('Ctrl Pts',(2.33035567060752,-0.447059686599547,
8.32043405970765));
#92095=CARTESIAN_POINT('Ctrl Pts',(2.27777143017788,-0.682213004957853,
8.30341206738335));
#92096=CARTESIAN_POINT('Ctrl Pts',(2.22349953377891,-0.842433419120874,
8.29100927223934));
#92097=CARTESIAN_POINT('Ctrl Pts',(2.11026041442282,-1.08730179754128,8.2713781832903));
#92098=CARTESIAN_POINT('Ctrl Pts',(2.06198217251954,-1.17629027647838,8.26409827929705));
#92099=CARTESIAN_POINT('Ctrl Pts',(2.00145534194759,-1.27260894965185,8.25624975431905));
#92100=CARTESIAN_POINT('Ctrl Pts',(1.99466180926581,-1.28323080886447,8.25538474084757));
#92101=CARTESIAN_POINT('Ctrl Pts',(1.98427135987478,-1.2991946313424,8.25408605884288));
#92102=CARTESIAN_POINT('Ctrl Pts',(1.98073699658057,-1.30457674078761,8.25364845284415));
#92103=CARTESIAN_POINT('Ctrl Pts',(1.97435726533354,-1.3142060661623,8.25286603772219));
#92104=CARTESIAN_POINT('Ctrl Pts',(1.97152005631048,-1.31845851837971,8.25252070184516));
#92105=CARTESIAN_POINT('Ctrl Pts',(1.9652857622723,-1.32773745085457,8.25176759482862));
#92106=CARTESIAN_POINT('Ctrl Pts',(1.96188313840014,-1.33276007561216,8.25136020325772));
#92107=CARTESIAN_POINT('Ctrl Pts',(1.95212915438269,-1.34703966358553,8.25020254034004));
#92108=CARTESIAN_POINT('Ctrl Pts',(1.94573118338759,-1.35626482115504,8.24945533597536));
#92109=CARTESIAN_POINT('Ctrl Pts',(1.90233027635461,-1.41790481135023,8.24446482271152));
#92110=CARTESIAN_POINT('Ctrl Pts',(1.86327531870815,-1.46885034293609,8.24035023002256));
#92111=CARTESIAN_POINT('Ctrl Pts',(1.68289114297404,-1.68536047254136,8.22260247412023));
#92112=CARTESIAN_POINT('Ctrl Pts',(1.52123285040937,-1.83260045205038,8.20972833868825));
#92113=CARTESIAN_POINT('Ctrl Pts',(1.28977074012306,-1.99139731878356,8.19195582127505));
#92114=CARTESIAN_POINT('Ctrl Pts',(1.23639293640038,-2.02496993568435,8.18790440629867));
#92115=CARTESIAN_POINT('Ctrl Pts',(1.16662423612708,-2.06506418658737,8.18263168299683));
#92116=CARTESIAN_POINT('Ctrl Pts',(1.1514085504619,-2.07358639220383,8.18148317239406));
#92117=CARTESIAN_POINT('Ctrl Pts',(1.12705565001879,-2.08687560652988,8.17964650319509));
#92118=CARTESIAN_POINT('Ctrl Pts',(1.11797875783969,-2.09175231006692,8.1789622704766));
#92119=CARTESIAN_POINT('Ctrl Pts',(1.10159859758542,-2.10041573628207,8.17772796926519));
#92120=CARTESIAN_POINT('Ctrl Pts',(1.09430681774201,-2.10422392371223,8.17717867315257));
#92121=CARTESIAN_POINT('Ctrl Pts',(1.07715976245044,-2.11306587041922,8.17588727331216));
#92122=CARTESIAN_POINT('Ctrl Pts',(1.0672888443581,-2.11806870569773,8.17514409528101));
#92123=CARTESIAN_POINT('Ctrl Pts',(1.03859135786244,-2.13236178855202,8.17298392631309));
#92124=CARTESIAN_POINT('Ctrl Pts',(1.01967640112659,-2.14147117499374,8.17156067936806));
#92125=CARTESIAN_POINT('Ctrl Pts',(0.836290734516628,-2.22680870456615,
8.15776344523456));
#92126=CARTESIAN_POINT('Ctrl Pts',(0.663746004042504,-2.28417906291392,
8.14472321476231));
#92127=CARTESIAN_POINT('Ctrl Pts',(0.344160640759544,-2.35114227672244,
8.12088072388546));
#92128=CARTESIAN_POINT('Ctrl Pts',(0.199476075607933,-2.36781203045311,
8.11021703771134));
#92129=CARTESIAN_POINT('Ctrl Pts',(0.0353569518289831,-2.37156105958021,
8.09880003056622));
#92130=CARTESIAN_POINT('Ctrl Pts',(0.0165441405859353,-2.37176691956004,
8.09750167556997));
#92131=CARTESIAN_POINT('Ctrl Pts',(-0.00995573825995391,-2.37174155814028,
8.0956892207875));
#92132=CARTESIAN_POINT('Ctrl Pts',(-0.0176416755835647,-2.3716968420938,
8.09516548809294));
#92133=CARTESIAN_POINT('Ctrl Pts',(-0.0305692244275301,-2.37155878378138,
8.0942880073471));
#92134=CARTESIAN_POINT('Ctrl Pts',(-0.0358109398957473,-2.37148542497318,
8.09393316368678));
#92135=CARTESIAN_POINT('Ctrl Pts',(-0.0465069566268487,-2.37130026060064,
8.09321107532711));
#92136=CARTESIAN_POINT('Ctrl Pts',(-0.0519611810340661,-2.37118701500951,
8.09284391253337));
#92137=CARTESIAN_POINT('Ctrl Pts',(-0.0658565801804263,-2.37085053826371,
8.09191108360727));
#92138=CARTESIAN_POINT('Ctrl Pts',(-0.0742971329552926,-2.37060104307359,
8.09134686699118));
#92139=CARTESIAN_POINT('Ctrl Pts',(-0.108581203077959,-2.36940434622817,
8.0890642777744));
#92140=CARTESIAN_POINT('Ctrl Pts',(-0.134410921354802,-2.36807953309005,
8.08736572004124));
#92141=CARTESIAN_POINT('Ctrl Pts',(-0.360520509866732,-2.35277053793205,
8.07264165946409));
#92142=CARTESIAN_POINT('Ctrl Pts',(-0.558320797704371,-2.31382923208865,
8.06070309561615));
#92143=CARTESIAN_POINT('Ctrl Pts',(-0.860767319413871,-2.21318439430736,
8.04099562808946));
#92144=CARTESIAN_POINT('Ctrl Pts',(-0.969716783353863,-2.16765985527582,
8.03358012009086));
#92145=CARTESIAN_POINT('Ctrl Pts',(-1.0912807338481,-2.10585977164396,8.02467274331321));
#92146=CARTESIAN_POINT('Ctrl Pts',(-1.10764212331602,-2.09730014847816,
8.02346025613574));
#92147=CARTESIAN_POINT('Ctrl Pts',(-1.13413942925326,-2.08304128240529,
8.02147340620565));
#92148=CARTESIAN_POINT('Ctrl Pts',(-1.14433652488689,-2.07745689217284,
8.0207031126838));
#92149=CARTESIAN_POINT('Ctrl Pts',(-1.16226797640115,-2.0674647409578,8.01933828437396));
#92150=CARTESIAN_POINT('Ctrl Pts',(-1.17001940492398,-2.06308795073163,
8.01874486844552));
#92151=CARTESIAN_POINT('Ctrl Pts',(-1.1863607543088,-2.05373920650361,8.0174864791963));
#92152=CARTESIAN_POINT('Ctrl Pts',(-1.19494445140899,-2.04875677437307,
8.01682113541318));
#92153=CARTESIAN_POINT('Ctrl Pts',(-1.21245708504015,-2.03844401798555,
8.01545464581285));
#92154=CARTESIAN_POINT('Ctrl Pts',(-1.22138273210964,-2.03310855913109,
8.01475332309753));
#92155=CARTESIAN_POINT('Ctrl Pts',(-1.24339138801022,-2.01975527369345,
8.01301178948753));
#92156=CARTESIAN_POINT('Ctrl Pts',(-1.25643206796592,-2.01166894608116,
8.01196908684175));
#92157=CARTESIAN_POINT('Ctrl Pts',(-1.29264916749593,-1.98872174001718,
8.00904250121894));
#92158=CARTESIAN_POINT('Ctrl Pts',(-1.31564601595939,-1.97358341095718,
8.00714852719978));
#92159=CARTESIAN_POINT('Ctrl Pts',(-1.39066111803529,-1.92230878743477,
8.00084988638151));
#92160=CARTESIAN_POINT('Ctrl Pts',(-1.44149201230967,-1.88449170563035,
7.99638539179347));
#92161=CARTESIAN_POINT('Ctrl Pts',(-1.60078961471317,-1.75575880720873,
7.98175300785968));
#92162=CARTESIAN_POINT('Ctrl Pts',(-1.70264950944771,-1.65716481953111,
7.97135555914241));
#92163=CARTESIAN_POINT('Ctrl Pts',(-1.86194245144197,-1.47269351742679,
7.95361625203662));
#92164=CARTESIAN_POINT('Ctrl Pts',(-1.92371118887939,-1.39104146408768,
7.94625102844911));
#92165=CARTESIAN_POINT('Ctrl Pts',(-1.98696804917734,-1.29511207146093,
7.93832299433738));
#92166=CARTESIAN_POINT('Ctrl Pts',(-1.99383090314272,-1.28452156596603,
7.9374572047261));
#92167=CARTESIAN_POINT('Ctrl Pts',(-2.00406863443511,-1.26844332110184,
7.93615759046452));
#92168=CARTESIAN_POINT('Ctrl Pts',(-2.00750608479414,-1.26299599064703,
7.93571982015363));
#92169=CARTESIAN_POINT('Ctrl Pts',(-2.01363190087266,-1.25320020933298,
7.93493723099745));
#92170=CARTESIAN_POINT('Ctrl Pts',(-2.01632842653346,-1.24885702738557,
7.93459188434299));
#92171=CARTESIAN_POINT('Ctrl Pts',(-2.02219322290946,-1.23934233036292,
7.93383889343509));
#92172=CARTESIAN_POINT('Ctrl Pts',(-2.02535570431436,-1.23416737750688,
7.93343162787353));
#92173=CARTESIAN_POINT('Ctrl Pts',(-2.03431085518383,-1.21938641718053,
7.93227468406153));
#92174=CARTESIAN_POINT('Ctrl Pts',(-2.04005537293105,-1.20975120488291,
7.93152806680918));
#92175=CARTESIAN_POINT('Ctrl Pts',(-2.07808902374704,-1.14491641343749,
7.92655199813902));
#92176=CARTESIAN_POINT('Ctrl Pts',(-2.10820591393473,-1.08846548071594,
7.92245040934162));
#92177=CARTESIAN_POINT('Ctrl Pts',(-2.24113877611426,-0.813020374338387,
7.9031862369006));
#92178=CARTESIAN_POINT('Ctrl Pts',(-2.31233108382151,-0.580382811643949,
7.88895642212421));
#92179=CARTESIAN_POINT('Ctrl Pts',(-2.35336661572382,-0.297921456548396,
7.87066208574375));
#92180=CARTESIAN_POINT('Ctrl Pts',(-2.35843608009614,-0.254696857708671,
7.86784093345273));
#92181=CARTESIAN_POINT('Ctrl Pts',(-2.36366943302811,-0.196204919219565,
7.86398302944334));
#92182=CARTESIAN_POINT('Ctrl Pts',(-2.3648794395102,-0.181038055292338,
7.86297906487534));
#92183=CARTESIAN_POINT('Ctrl Pts',(-2.36662986864864,-0.156068839904069,
7.86131983878432));
#92184=CARTESIAN_POINT('Ctrl Pts',(-2.36725551966758,-0.146272750762116,
7.86066726308839));
#92185=CARTESIAN_POINT('Ctrl Pts',(-2.36832248139079,-0.127760882139914,
7.85943090178037));
#92186=CARTESIAN_POINT('Ctrl Pts',(-2.36877653456722,-0.119045976952484,
7.85884752688647));
#92187=CARTESIAN_POINT('Ctrl Pts',(-2.36960235079768,-0.101312545565581,
7.85765766889985));
#92188=CARTESIAN_POINT('Ctrl Pts',(-2.36997074746637,-0.0922940140209736,
7.85705108989024));
#92189=CARTESIAN_POINT('Ctrl Pts',(-2.37074905561044,-0.0701403924997397,
7.85555736416993));
#92190=CARTESIAN_POINT('Ctrl Pts',(-2.37110128939492,-0.0570037069790923,
7.8546684259942));
#92191=CARTESIAN_POINT('Ctrl Pts',(-2.371620102822,-0.0289566246185791,
7.85276350603436));
#92192=CARTESIAN_POINT('Ctrl Pts',(-2.37175527357193,-0.0140463379688937,
7.85174658567412));
#92193=CARTESIAN_POINT('Ctrl Pts',(-2.37174984266889,0.000863886614090527,
7.85072532400096));
#92194=CARTESIAN_POINT('Ctrl Pts',(-2.37174984331459,0.000862112068730794,
7.85072544554674));
#92195=CARTESIAN_POINT('Ctrl Pts',(-2.37172894381041,0.0583585763559521,
7.84678728115609));
#92196=CARTESIAN_POINT('Ctrl Pts',(-2.36961730594813,0.115801390350126,
7.8427874875871));
#92197=CARTESIAN_POINT('Ctrl Pts',(-2.36542646504704,0.173077153186224,
7.83873326832757));
#92198=CARTESIAN_POINT('',(-2.3717492188972,0.0019248793473943,7.65246806900456));
#92199=CARTESIAN_POINT('Ctrl Pts',(-2.36542649614281,0.173076728203254,
7.64172477676247));
#92200=CARTESIAN_POINT('Ctrl Pts',(-2.36959267265298,0.11613791033294,7.64536496783797));
#92201=CARTESIAN_POINT('Ctrl Pts',(-2.37170285684927,0.0590500966492621,
7.64893264892313));
#92202=CARTESIAN_POINT('Ctrl Pts',(-2.3717492188972,0.00192487934712052,
7.65246806900458));
#92203=CARTESIAN_POINT('Ctrl Pts',(-2.37174921666776,0.00192762440904576,
7.65246789911553));
#92204=CARTESIAN_POINT('Ctrl Pts',(-2.37192860088264,-0.218786726951562,
7.66612768429334));
#92205=CARTESIAN_POINT('Ctrl Pts',(-2.34130138544471,-0.43844049729506,
7.67932270627705));
#92206=CARTESIAN_POINT('Ctrl Pts',(-2.27218153710609,-0.680707332112222,
7.69562531301407));
#92207=CARTESIAN_POINT('Ctrl Pts',(-2.26303122594774,-0.710535664963517,
7.69766164811093));
#92208=CARTESIAN_POINT('Ctrl Pts',(-2.24921652196154,-0.752591482057263,
7.70057829124152));
#92209=CARTESIAN_POINT('Ctrl Pts',(-2.24503496904491,-0.764975083100874,
7.7014427783787));
#92210=CARTESIAN_POINT('Ctrl Pts',(-2.23764523888286,-0.786277092369439,
7.70293993684019));
#92211=CARTESIAN_POINT('Ctrl Pts',(-2.23448553535929,-0.795212090500742,
7.70357099320596));
#92212=CARTESIAN_POINT('Ctrl Pts',(-2.22832899839354,-0.812295085289945,
7.70478354842714));
#92213=CARTESIAN_POINT('Ctrl Pts',(-2.22534080625714,-0.820446051367029,
7.70536475100197));
#92214=CARTESIAN_POINT('Ctrl Pts',(-2.21821441266406,-0.839559516379358,
7.70673394995192));
#92215=CARTESIAN_POINT('Ctrl Pts',(-2.2140396190855,-0.850508035601309,
7.7075231597099));
#92216=CARTESIAN_POINT('Ctrl Pts',(-2.19930539126171,-0.888305243557391,
7.71026505002614));
#92217=CARTESIAN_POINT('Ctrl Pts',(-2.18833768312951,-0.914990965097235,
7.71223135801434));
#92218=CARTESIAN_POINT('Ctrl Pts',(-2.10917336351463,-1.09803653285982,
7.72593677724298));
#92219=CARTESIAN_POINT('Ctrl Pts',(-2.02477969696945,-1.24681300971397,
7.73824124994806));
#92220=CARTESIAN_POINT('Ctrl Pts',(-1.86186624881698,-1.47322976706895,
7.75860934982358));
#92221=CARTESIAN_POINT('Ctrl Pts',(-1.79258339652364,-1.55679129554724,
7.76654784187988));
#92222=CARTESIAN_POINT('Ctrl Pts',(-1.69595415681631,-1.65829537400793,
7.77652525571581));
#92223=CARTESIAN_POINT('Ctrl Pts',(-1.67362526589386,-1.68082798967231,
7.77876311605866));
#92224=CARTESIAN_POINT('Ctrl Pts',(-1.64060205390072,-1.71284169736762,
7.78196812842707));
#92225=CARTESIAN_POINT('Ctrl Pts',(-1.630264365805,-1.72268392360885,7.78295710178009));
#92226=CARTESIAN_POINT('Ctrl Pts',(-1.61176502101676,-1.73998095802047,
7.78470066641895));
#92227=CARTESIAN_POINT('Ctrl Pts',(-1.60363901473207,-1.7474730726551,7.78545776194948));
#92228=CARTESIAN_POINT('Ctrl Pts',(-1.59091844608578,-1.7590378751639,7.78662894665626));
#92229=CARTESIAN_POINT('Ctrl Pts',(-1.58636007589046,-1.76314986888534,
7.78704588081393));
#92230=CARTESIAN_POINT('Ctrl Pts',(-1.5817632737829,-1.76726427257486,7.7874635243222));
#92231=CARTESIAN_POINT('Ctrl Pts',(-1.58174082104448,-1.76728436830338,
7.78746556420386));
#92232=CARTESIAN_POINT('Ctrl Pts',(-1.58169573582957,-1.76732471908279,
7.78746966016217));
#92233=CARTESIAN_POINT('Ctrl Pts',(-1.58167310334443,-1.76734497412907,
7.78747171623854));
#92234=CARTESIAN_POINT('Ctrl Pts',(-1.58162765563735,-1.76738564619058,
7.78747584485546));
#92235=CARTESIAN_POINT('Ctrl Pts',(-1.58160484041494,-1.76740606319358,
7.78747791739495));
#92236=CARTESIAN_POINT('Ctrl Pts',(-1.58155902418017,-1.76744706186265,
7.78748207921214));
#92237=CARTESIAN_POINT('Ctrl Pts',(-1.58153602315364,-1.76746764352845,
7.78748416848999));
#92238=CARTESIAN_POINT('Ctrl Pts',(-1.58148983220547,-1.76750897426265,
7.78748836406255));
#92239=CARTESIAN_POINT('Ctrl Pts',(-1.58146664225343,-1.76752972334497,
7.78749047035887));
#92240=CARTESIAN_POINT('Ctrl Pts',(-1.58142007026705,-1.76757139172394,
7.78749470025433));
#92241=CARTESIAN_POINT('Ctrl Pts',(-1.58139668821649,-1.76759231102148,
7.78749682385378));
#92242=CARTESIAN_POINT('Ctrl Pts',(-1.58134972876095,-1.76763432271736,
7.78750108864911));
#92243=CARTESIAN_POINT('Ctrl Pts',(-1.58132615137002,-1.76765541508917,
7.78750322984251));
#92244=CARTESIAN_POINT('Ctrl Pts',(-1.57743751763007,-1.77113405301657,
7.78785636601053));
#92245=CARTESIAN_POINT('Ctrl Pts',(-1.57356118211384,-1.77457886918644,
7.78820639012734));
#92246=CARTESIAN_POINT('Ctrl Pts',(-1.56478425285835,-1.78232736593142,
7.78899446159449));
#92247=CARTESIAN_POINT('Ctrl Pts',(-1.55987719428778,-1.78662355818461,
7.78943195334877));
#92248=CARTESIAN_POINT('Ctrl Pts',(-1.54532731845717,-1.79925651951637,
7.79072022669069));
#92249=CARTESIAN_POINT('Ctrl Pts',(-1.53563475392933,-1.80753602028861,
7.79156692120089));
#92250=CARTESIAN_POINT('Ctrl Pts',(-1.44567199322042,-1.88313726106466,
7.79932543103659));
#92251=CARTESIAN_POINT('Ctrl Pts',(-1.36107906131502,-1.94515894084533,
7.80589398461622));
#92252=CARTESIAN_POINT('Ctrl Pts',(-1.13573497658213,-2.0884515400315,7.82239169432572));
#92253=CARTESIAN_POINT('Ctrl Pts',(-0.990252594035798,-2.16123178770184,
7.83216958849789));
#92254=CARTESIAN_POINT('Ctrl Pts',(-0.769153371904203,-2.24479261153157,
7.84705451056726));
#92255=CARTESIAN_POINT('Ctrl Pts',(-0.698642810193412,-2.26772733455831,
7.85179919609393));
#92256=CARTESIAN_POINT('Ctrl Pts',(-0.610046009439683,-2.29202040896952,
7.85781694461759));
#92257=CARTESIAN_POINT('Ctrl Pts',(-0.592860705422668,-2.29652560277634,
7.85898667980493));
#92258=CARTESIAN_POINT('Ctrl Pts',(-0.565470826512183,-2.30337804242389,
7.86085562220351));
#92259=CARTESIAN_POINT('Ctrl Pts',(-0.555298291578314,-2.30585157010133,
7.86155074862283));
#92260=CARTESIAN_POINT('Ctrl Pts',(-0.536086811353472,-2.3103884844237,
7.86286558426991));
#92261=CARTESIAN_POINT('Ctrl Pts',(-0.527051467169752,-2.31246638137894,
7.86348481334003));
#92262=CARTESIAN_POINT('Ctrl Pts',(-0.50663728074524,-2.31703526280935,
7.86488590661512));
#92263=CARTESIAN_POINT('Ctrl Pts',(-0.495251872755064,-2.31949548769823,
7.86566874061982));
#92264=CARTESIAN_POINT('Ctrl Pts',(-0.465980398223726,-2.32559529631513,
7.86768522608391));
#92265=CARTESIAN_POINT('Ctrl Pts',(-0.448069880514236,-2.32911239819154,
7.86892274457843));
#92266=CARTESIAN_POINT('Ctrl Pts',(-0.328360836412189,-2.35118789048866,
7.87722016717372));
#92267=CARTESIAN_POINT('Ctrl Pts',(-0.225496517827373,-2.36327129190197,
7.8844833949992));
#92268=CARTESIAN_POINT('Ctrl Pts',(0.0538466149963302,-2.37768121172518,
7.90454373892599));
#92269=CARTESIAN_POINT('Ctrl Pts',(0.230325737271339,-2.36711033042453,
7.91761175438503));
#92270=CARTESIAN_POINT('Ctrl Pts',(0.443561688708806,-2.33024959707788,
7.93312658520144));
#92271=CARTESIAN_POINT('Ctrl Pts',(0.48294823245229,-2.32240641399065,7.93597778851135));
#92272=CARTESIAN_POINT('Ctrl Pts',(0.538527055449659,-2.30986354852391,
7.93996398265532));
#92273=CARTESIAN_POINT('Ctrl Pts',(0.554895914538838,-2.30598602851345,
7.94113334416176));
#92274=CARTESIAN_POINT('Ctrl Pts',(0.583741168348567,-2.29882810880787,
7.9431841770056));
#92275=CARTESIAN_POINT('Ctrl Pts',(0.596234479738183,-2.29561950015035,
7.94406914674796));
#92276=CARTESIAN_POINT('Ctrl Pts',(0.614952451714953,-2.29064911681129,
7.94538948207015));
#92277=CARTESIAN_POINT('Ctrl Pts',(0.621196840156112,-2.28896360445724,
7.94582901771423));
#92278=CARTESIAN_POINT('Ctrl Pts',(0.631949179193921,-2.28601404522876,
7.94658415966411));
#92279=CARTESIAN_POINT('Ctrl Pts',(0.636460340536291,-2.28476217937959,
7.94690045797753));
#92280=CARTESIAN_POINT('Ctrl Pts',(0.646750228662881,-2.2818738514643,7.94762072521921));
#92281=CARTESIAN_POINT('Ctrl Pts',(0.652526458891404,-2.28022879438711,
7.94802419000673));
#92282=CARTESIAN_POINT('Ctrl Pts',(0.668309623487413,-2.27566889989062,
7.94912444201026));
#92283=CARTESIAN_POINT('Ctrl Pts',(0.678303840366494,-2.27270996938229,
7.94981873144103));
#92284=CARTESIAN_POINT('Ctrl Pts',(0.728555636433139,-2.257471191399,7.95329903446736));
#92285=CARTESIAN_POINT('Ctrl Pts',(0.768503642656891,-2.24418630722255,
7.956031232103));
#92286=CARTESIAN_POINT('Ctrl Pts',(1.03125768702466,-2.14896609673899,7.97390302597769));
#92287=CARTESIAN_POINT('Ctrl Pts',(1.2410444322419,-2.03503842775949,7.98782459160855));
#92288=CARTESIAN_POINT('Ctrl Pts',(1.48381414625764,-1.85147833532065,8.007064662004));
#92289=CARTESIAN_POINT('Ctrl Pts',(1.53545725290334,-1.80887980730665,8.0113615115092));
#92290=CARTESIAN_POINT('Ctrl Pts',(1.59803648104308,-1.75264772171217,8.01687589567338));
#92291=CARTESIAN_POINT('Ctrl Pts',(1.61071991894831,-1.74099854906542,8.01801027817766));
#92292=CARTESIAN_POINT('Ctrl Pts',(1.6308206832079,-1.72212922594299,8.01983577216126));
#92293=CARTESIAN_POINT('Ctrl Pts',(1.63831971673366,-1.71499669725583,8.02052312930039));
#92294=CARTESIAN_POINT('Ctrl Pts',(1.65246244522582,-1.7013677637352,8.02183165162688));
#92295=CARTESIAN_POINT('Ctrl Pts',(1.65911513084298,-1.69488093349532,8.02245239351364));
#92296=CARTESIAN_POINT('Ctrl Pts',(1.67416254690773,-1.6800351692993,8.02386847330971));
#92297=CARTESIAN_POINT('Ctrl Pts',(1.68253305669345,-1.6716521491691,8.02466486537424));
#92298=CARTESIAN_POINT('Ctrl Pts',(1.70410035296448,-1.64972652268232,8.02673971882568));
#92299=CARTESIAN_POINT('Ctrl Pts',(1.71719839197827,-1.63608840195997,8.02802243360856));
#92300=CARTESIAN_POINT('Ctrl Pts',(1.83688724967364,-1.50844366412966,8.03995840314521));
#92301=CARTESIAN_POINT('Ctrl Pts',(1.93212338863065,-1.38435502843599,8.05109492036227));
#92302=CARTESIAN_POINT('Ctrl Pts',(2.0743639600938,-1.15546021201152,8.0707105500214));
#92303=CARTESIAN_POINT('Ctrl Pts',(2.12726296739755,-1.05490624095178,8.07905072621117));
#92304=CARTESIAN_POINT('Ctrl Pts',(2.20010305575462,-0.888478979701357,
8.09212713522253));
#92305=CARTESIAN_POINT('Ctrl Pts',(2.2247410068928,-0.824850162908237,8.09696539607802));
#92306=CARTESIAN_POINT('Ctrl Pts',(2.25029175812542,-0.749344650721646,
8.10245456541853));
#92307=CARTESIAN_POINT('Ctrl Pts',(2.253899987388,-0.738420789667044,8.10324265207015));
#92308=CARTESIAN_POINT('Ctrl Pts',(2.25932372613631,-0.721590282000285,
8.10444710367688));
#92309=CARTESIAN_POINT('Ctrl Pts',(2.26119581323298,-0.715702264209388,
8.1048666439587));
#92310=CARTESIAN_POINT('Ctrl Pts',(2.26459672681886,-0.704859287063302,
8.10563579782369));
#92311=CARTESIAN_POINT('Ctrl Pts',(2.2661323075919,-0.699906647503912,8.10598579062392));
#92312=CARTESIAN_POINT('Ctrl Pts',(2.26955931475563,-0.688724157550284,
8.10677307175319));
#92313=CARTESIAN_POINT('Ctrl Pts',(2.27144133725613,-0.682491540135342,
8.10720980953822));
#92314=CARTESIAN_POINT('Ctrl Pts',(2.27691692184927,-0.664084719363218,
8.10849378687591));
#92315=CARTESIAN_POINT('Ctrl Pts',(2.28043851452818,-0.651889087697727,
8.10933697980915));
#92316=CARTESIAN_POINT('Ctrl Pts',(2.31616581103711,-0.524328312352295,
8.11808383156427));
#92317=CARTESIAN_POINT('Ctrl Pts',(2.33969111922926,-0.406691781487523,
8.12553671988815));
#92318=CARTESIAN_POINT('Ctrl Pts',(2.3699649896917,-0.159019687854613,8.14089061698964));
#92319=CARTESIAN_POINT('Ctrl Pts',(2.37511420731575,-0.0292037167191159,
8.14875802649651));
#92320=CARTESIAN_POINT('Ctrl Pts',(2.36711062306637,0.159731648666867,8.16057761604705));
#92321=CARTESIAN_POINT('Ctrl Pts',(2.36236770825756,0.218963284601689,8.16433398724319));
#92322=CARTESIAN_POINT('Ctrl Pts',(2.3508003038964,0.316987426391103,8.17068231363855));
#92323=CARTESIAN_POINT('Ctrl Pts',(2.34522436061761,0.355900976238753,8.17323716232165));
#92324=CARTESIAN_POINT('Ctrl Pts',(2.33630524755926,0.408754540364765,8.17676280494017));
#92325=CARTESIAN_POINT('Ctrl Pts',(2.3337987543899,0.422830749852764,8.1777071672099));
#92326=CARTESIAN_POINT('Ctrl Pts',(2.32937537323449,0.446433471574632,8.17930011228693));
#92327=CARTESIAN_POINT('Ctrl Pts',(2.32752690736601,0.455972548133588,8.17994650763121));
#92328=CARTESIAN_POINT('Ctrl Pts',(2.32376397221013,0.474772030843289,8.18122568152593));
#92329=CARTESIAN_POINT('Ctrl Pts',(2.32185263144854,0.484032884386455,8.18185834925603));
#92330=CARTESIAN_POINT('Ctrl Pts',(2.31752246192929,0.504397504801937,8.18325527716475));
#92331=CARTESIAN_POINT('Ctrl Pts',(2.31507911671761,0.515495761283541,8.1840203096959));
#92332=CARTESIAN_POINT('Ctrl Pts',(2.30620814969534,0.554454267931089,8.186719255279));
#92333=CARTESIAN_POINT('Ctrl Pts',(2.29935680906721,0.582214483461349,8.18866667231378));
#92334=CARTESIAN_POINT('Ctrl Pts',(2.24384275921103,0.790855894249398,8.20349341156407));
#92335=CARTESIAN_POINT('Ctrl Pts',(2.17441525541434,0.965491793292687,8.21706902191983));
#92336=CARTESIAN_POINT('Ctrl Pts',(2.02036184227032,1.24974074686779,8.24068413450164));
#92337=CARTESIAN_POINT('Ctrl Pts',(1.94534172660645,1.36358655212556,8.25060977062618));
#92338=CARTESIAN_POINT('Ctrl Pts',(1.85282875956584,1.48067409651524,8.26091026115462));
#92339=CARTESIAN_POINT('Ctrl Pts',(1.8446095353432,1.49090102765728,8.26181064853863));
#92340=CARTESIAN_POINT('Ctrl Pts',(1.83218401506842,1.50610165938006,8.26314931483075));
#92341=CARTESIAN_POINT('Ctrl Pts',(1.82804158145697,1.51112688167012,8.2635919330658));
#92342=CARTESIAN_POINT('Ctrl Pts',(1.82088280583333,1.51973873750585,8.26435047673394));
#92343=CARTESIAN_POINT('Ctrl Pts',(1.81787648893822,1.52333354693099,8.26466711330541));
#92344=CARTESIAN_POINT('Ctrl Pts',(1.81101366923395,1.53149052771232,8.26538558280907));
#92345=CARTESIAN_POINT('Ctrl Pts',(1.80715057696887,1.5360470503172,8.26578692680853));
#92346=CARTESIAN_POINT('Ctrl Pts',(1.79659103315127,1.54840707065965,8.26687577904613));
#92347=CARTESIAN_POINT('Ctrl Pts',(1.78986088544994,1.55618180725455,8.2675608742569));
#92348=CARTESIAN_POINT('Ctrl Pts',(1.75641457487899,1.59431530098481,8.27092347074607));
#92349=CARTESIAN_POINT('Ctrl Pts',(1.72897372689929,1.62403317956031,8.27355139607813));
#92350=CARTESIAN_POINT('Ctrl Pts',(1.53399854410094,1.82464016462,8.29146545822072));
#92351=CARTESIAN_POINT('Ctrl Pts',(1.34219277605546,1.97002747896156,8.30548813971534));
#92352=CARTESIAN_POINT('Ctrl Pts',(1.07304659711696,2.11618681682525,8.3248494805174));
#92353=CARTESIAN_POINT('Ctrl Pts',(1.01292294352818,2.14561446678293,8.32914595517858));
#92354=CARTESIAN_POINT('Ctrl Pts',(0.935866155060962,2.17936898076047,8.33465991717734));
#92355=CARTESIAN_POINT('Ctrl Pts',(0.920018041369216,2.18610644572128,8.33579426824626));
#92356=CARTESIAN_POINT('Ctrl Pts',(0.894530480204811,2.19661566720407,8.33761972359626));
#92357=CARTESIAN_POINT('Ctrl Pts',(0.884937067056213,2.20049802339901,8.3383070738224));
#92358=CARTESIAN_POINT('Ctrl Pts',(0.866682794901249,2.20774666431054,8.33961559072481));
#92359=CARTESIAN_POINT('Ctrl Pts',(0.858026940167629,2.21112509064001,8.34023633415188));
#92360=CARTESIAN_POINT('Ctrl Pts',(0.838290503027163,2.21869498591577,8.34165242822353));
#92361=CARTESIAN_POINT('Ctrl Pts',(0.827197991733631,2.22285444453782,8.34244883310317));
#92362=CARTESIAN_POINT('Ctrl Pts',(0.798319962038955,2.23343700927993,8.34452374195813));
#92363=CARTESIAN_POINT('Ctrl Pts',(0.780488254253281,2.23973071707422,8.34580649970427));
#92364=CARTESIAN_POINT('Ctrl Pts',(0.614948161600429,2.295941235759,8.35773166301482));
#92365=CARTESIAN_POINT('Ctrl Pts',(0.46275844444034,2.33138256170428,8.36885627705974));
#92366=CARTESIAN_POINT('Ctrl Pts',(0.195684482133528,2.36638706698536,8.38846172109897));
#92367=CARTESIAN_POINT('Ctrl Pts',(0.0822331865416702,2.37303995511256,
8.3968039434546));
#92368=CARTESIAN_POINT('Ctrl Pts',(-0.0995696787147946,2.37064358595411,
8.40989181736451));
#92369=CARTESIAN_POINT('Ctrl Pts',(-0.167816555524349,2.36679207601819,
8.41473907387445));
#92370=CARTESIAN_POINT('Ctrl Pts',(-0.247260229332893,2.35885414806334,
8.42023708203639));
#92371=CARTESIAN_POINT('Ctrl Pts',(-0.258703727371872,2.35762654120908,
8.42102550232202));
#92372=CARTESIAN_POINT('Ctrl Pts',(-0.27627728828819,2.35561183287246,8.42223035499623));
#92373=CARTESIAN_POINT('Ctrl Pts',(-0.282413767332848,2.35488401273431,
8.42264996593309));
#92374=CARTESIAN_POINT('Ctrl Pts',(-0.293694126550658,2.35350137222549,
8.4234191867187));
#92375=CARTESIAN_POINT('Ctrl Pts',(-0.298838685741296,2.35285366948261,
8.42376917626327));
#92376=CARTESIAN_POINT('Ctrl Pts',(-0.310436767805653,2.35135481063076,
8.42455637198977));
#92377=CARTESIAN_POINT('Ctrl Pts',(-0.31688892664277,2.35049395723892,8.42499302817472));
#92378=CARTESIAN_POINT('Ctrl Pts',(-0.335906663700115,2.34787686006161,
8.42627654097232));
#92379=CARTESIAN_POINT('Ctrl Pts',(-0.348462034237727,2.34604630497996,
8.42711935532858));
#92380=CARTESIAN_POINT('Ctrl Pts',(-0.4575920556738,2.32923987488406,8.43441013059238));
#92381=CARTESIAN_POINT('Ctrl Pts',(-0.553183364220935,2.30840683760629,
8.44055992959317));
#92382=CARTESIAN_POINT('Ctrl Pts',(-0.790172107251115,2.24118347439208,
8.45581457527896));
#92383=CARTESIAN_POINT('Ctrl Pts',(-0.92898848343422,2.1872943136355,8.4647755324396));
#92384=CARTESIAN_POINT('Ctrl Pts',(-1.11672165895345,2.09329794651781,8.47788145550354));
#92385=CARTESIAN_POINT('Ctrl Pts',(-1.17050135962174,2.06370764981427,8.48175709537557));
#92386=CARTESIAN_POINT('Ctrl Pts',(-1.24622957730996,2.0181279808486,8.48743803975325));
#92387=CARTESIAN_POINT('Ctrl Pts',(-1.26914793891468,2.003794431307,8.48918800053778));
#92388=CARTESIAN_POINT('Ctrl Pts',(-1.30980528736982,1.97738926464679,8.49235171782997));
#92389=CARTESIAN_POINT('Ctrl Pts',(-1.32763511780299,1.96546257635707,8.49376016772213));
#92390=CARTESIAN_POINT('Ctrl Pts',(-1.35457147497543,1.94691060670137,8.4959216170941));
#92391=CARTESIAN_POINT('Ctrl Pts',(-1.36379697557336,1.94045937687495,8.49666802771135));
#92392=CARTESIAN_POINT('Ctrl Pts',(-1.3797838419841,1.92910972120071,8.4979723906345));
#92393=CARTESIAN_POINT('Ctrl Pts',(-1.38656597413737,1.92424077582012,8.49852920472557));
#92394=CARTESIAN_POINT('Ctrl Pts',(-1.40176556114031,1.91320679333387,8.49978499549225));
#92395=CARTESIAN_POINT('Ctrl Pts',(-1.41016828185193,1.90702184918722,8.50048473607025));
#92396=CARTESIAN_POINT('Ctrl Pts',(-1.43263859721201,1.89025253199371,8.50237100638169));
#92397=CARTESIAN_POINT('Ctrl Pts',(-1.44662937794588,1.87956681142386,8.5035614835849));
#92398=CARTESIAN_POINT('Ctrl Pts',(-1.51028752365827,1.82981491280577,8.50905344744782));
#92399=CARTESIAN_POINT('Ctrl Pts',(-1.55849601299402,1.78893261151242,8.51342670799578));
#92400=CARTESIAN_POINT('Ctrl Pts',(-1.76462150752,1.59947094617974,8.53311995723026));
#92401=CARTESIAN_POINT('Ctrl Pts',(-1.90335367581959,1.43157781383691,8.54923751710816));
#92402=CARTESIAN_POINT('Ctrl Pts',(-2.04001914724145,1.21052969990413,8.56790986979901));
#92403=CARTESIAN_POINT('Ctrl Pts',(-2.06170774698637,1.17321008760432,8.57098062684834));
#92404=CARTESIAN_POINT('Ctrl Pts',(-2.09082889556275,1.11979688937596,8.57524215404591));
#92405=CARTESIAN_POINT('Ctrl Pts',(-2.09911716692401,1.10418191730466,8.57647232002537));
#92406=CARTESIAN_POINT('Ctrl Pts',(-2.11338497739413,1.07656019193318,8.5786191602735));
#92407=CARTESIAN_POINT('Ctrl Pts',(-2.11943861144178,1.06459283434656,8.57953978729675));
#92408=CARTESIAN_POINT('Ctrl Pts',(-2.12830648222711,1.04668655750896,8.58090247118137));
#92409=CARTESIAN_POINT('Ctrl Pts',(-2.13119794544306,1.04078650642126,8.58134909413646));
#92410=CARTESIAN_POINT('Ctrl Pts',(-2.13632888775373,1.03020574067668,8.58214569343673));
#92411=CARTESIAN_POINT('Ctrl Pts',(-2.13857755262276,1.02552963775957,8.582496228079));
#92412=CARTESIAN_POINT('Ctrl Pts',(-2.14344956230167,1.01531257161977,8.58325881612217));
#92413=CARTESIAN_POINT('Ctrl Pts',(-2.14606677335011,1.00976881052047,8.58367049097765));
#92414=CARTESIAN_POINT('Ctrl Pts',(-2.1533067591757,0.994277817243223,8.5848151531173));
#92415=CARTESIAN_POINT('Ctrl Pts',(-2.15788214205157,0.984308411828276,
8.58554530008407));
#92416=CARTESIAN_POINT('Ctrl Pts',(-2.18273764902182,0.929143831821751,
8.58955162580048));
#92417=CARTESIAN_POINT('Ctrl Pts',(-2.20166883701195,0.883349916415549,
8.59275267570003));
#92418=CARTESIAN_POINT('Ctrl Pts',(-2.27089344763987,0.699811890386293,
8.60522293157261));
#92419=CARTESIAN_POINT('Ctrl Pts',(-2.30980639830815,0.558117742458064,
8.61408114242414));
#92420=CARTESIAN_POINT('Ctrl Pts',(-2.34950444186218,0.334032260774997,
8.62807067485331));
#92421=CARTESIAN_POINT('Ctrl Pts',(-2.35952658917613,0.253710412752258,
8.63307805857323));
#92422=CARTESIAN_POINT('Ctrl Pts',(-2.36542651242649,0.173076505655319,
8.63818628587103));
#92423=CARTESIAN_POINT('Origin',(0.,0.,-1.84858989190503));
#92424=CARTESIAN_POINT('',(-2.36542649454068,0.173076750099461,9.83480414144792));
#92425=CARTESIAN_POINT('',(-2.36542652525385,0.173076330344439,9.63839747301829));
#92426=CARTESIAN_POINT('',(-2.36542649454111,0.173076750093529,-1.84858989190503));
#92427=CARTESIAN_POINT('Ctrl Pts',(-2.36542649454068,0.173076750099461,
9.83480414144792));
#92428=CARTESIAN_POINT('Ctrl Pts',(-2.36520189196563,0.176146376039912,
9.83460373033529));
#92429=CARTESIAN_POINT('Ctrl Pts',(-2.36497131147088,0.179215601897425,
9.83440358283108));
#92430=CARTESIAN_POINT('Ctrl Pts',(-2.35354069918992,0.327502370317676,
9.82474474557395));
#92431=CARTESIAN_POINT('Ctrl Pts',(-2.32899219074479,0.471400117259506,
9.8158733937563));
#92432=CARTESIAN_POINT('Ctrl Pts',(-2.26306492284725,0.718177746968243,
9.80022191436453));
#92433=CARTESIAN_POINT('Ctrl Pts',(-2.22741598848653,0.822105685596256,
9.79348664564198));
#92434=CARTESIAN_POINT('Ctrl Pts',(-2.16708713367593,0.964872791272013,
9.78369709492289));
#92435=CARTESIAN_POINT('Ctrl Pts',(-2.14828304071982,1.00604459915777,9.78080854905148));
#92436=CARTESIAN_POINT('Ctrl Pts',(-2.11419972312488,1.07535132719678,9.77581374263377));
#92437=CARTESIAN_POINT('Ctrl Pts',(-2.09950736217764,1.10376157850436,9.77372705491302));
#92438=CARTESIAN_POINT('Ctrl Pts',(-2.07799984048058,1.14336608750461,9.77075806051486));
#92439=CARTESIAN_POINT('Ctrl Pts',(-2.07165910538677,1.15481508761203,9.76989256217579));
#92440=CARTESIAN_POINT('Ctrl Pts',(-2.06061226594895,1.17437775826175,9.76840097692716));
#92441=CARTESIAN_POINT('Ctrl Pts',(-2.05595214116193,1.18251715361473,9.76777655166614));
#92442=CARTESIAN_POINT('Ctrl Pts',(-2.04696906422128,1.19799341717992,9.76658184145591));
#92443=CARTESIAN_POINT('Ctrl Pts',(-2.04265462618595,1.20533507885905,9.76601187248871));
#92444=CARTESIAN_POINT('Ctrl Pts',(-2.03138946095268,1.22427024845548,9.7645333909355));
#92445=CARTESIAN_POINT('Ctrl Pts',(-2.02437906953714,1.23582771976395,9.76362271000136));
#92446=CARTESIAN_POINT('Ctrl Pts',(-2.00405767501777,1.26869306460819,9.76100896875709));
#92447=CARTESIAN_POINT('Ctrl Pts',(-1.99050672531021,1.28984966128162,9.75929712727667));
#92448=CARTESIAN_POINT('Ctrl Pts',(-1.86907764731955,1.47296072131843,9.74421756642246));
#92449=CARTESIAN_POINT('Ctrl Pts',(-1.74200303042382,1.62125244916112,9.73008637235316));
#92450=CARTESIAN_POINT('Ctrl Pts',(-1.50247742827674,1.83972176791455,9.7064085107244));
#92451=CARTESIAN_POINT('Ctrl Pts',(-1.39964843200042,1.91911620584917,9.69696848790556));
#92452=CARTESIAN_POINT('Ctrl Pts',(-1.28292133501019,1.99484330885392,9.68736024983176));
#92453=CARTESIAN_POINT('Ctrl Pts',(-1.27497999778377,1.99992824651159,9.68671178875491));
#92454=CARTESIAN_POINT('Ctrl Pts',(-1.26021409805653,2.00925933778014,9.68551599387643));
#92455=CARTESIAN_POINT('Ctrl Pts',(-1.25339790479187,2.01351840230391,9.68496787610201));
#92456=CARTESIAN_POINT('Ctrl Pts',(-1.24203767474033,2.02053674431366,9.68406095336158));
#92457=CARTESIAN_POINT('Ctrl Pts',(-1.23750584331412,2.02331549932154,9.68370089515491));
#92458=CARTESIAN_POINT('Ctrl Pts',(-1.22860481534658,2.02873219466124,9.68299714712032));
#92459=CARTESIAN_POINT('Ctrl Pts',(-1.22423638900692,2.03137130400507,9.68265338328671));
#92460=CARTESIAN_POINT('Ctrl Pts',(-1.21327839092734,2.03794320251537,9.68179502696464));
#92461=CARTESIAN_POINT('Ctrl Pts',(-1.20667811319793,2.04185819434838,9.68128158563876));
#92462=CARTESIAN_POINT('Ctrl Pts',(-1.18403173280879,2.05514286081245,9.67953166228116));
#92463=CARTESIAN_POINT('Ctrl Pts',(-1.16789408199821,2.06435626503,9.67830476949922));
#92464=CARTESIAN_POINT('Ctrl Pts',(-1.0206219417993,2.14615790831986,9.66727346053435));
#92465=CARTESIAN_POINT('Ctrl Pts',(-0.882970506837756,2.2063633660639,9.65812785016056));
#92466=CARTESIAN_POINT('Ctrl Pts',(-0.625473537362864,2.2909934830777,9.6415209574469));
#92467=CARTESIAN_POINT('Ctrl Pts',(-0.507689059251745,2.31993901576067,
9.63409869145891));
#92468=CARTESIAN_POINT('Ctrl Pts',(-0.34699157199473,2.3466020146696,9.62377954905083));
#92469=CARTESIAN_POINT('Ctrl Pts',(-0.305597189333393,2.35235078384599,
9.62110585660863));
#92470=CARTESIAN_POINT('Ctrl Pts',(-0.234172470778824,2.3603530798215,9.61645085986825));
#92471=CARTESIAN_POINT('Ctrl Pts',(-0.204210733580883,2.36313377736749,
9.6144856860689));
#92472=CARTESIAN_POINT('Ctrl Pts',(-0.161464333748262,2.36628200846518,
9.61166069401964));
#92473=CARTESIAN_POINT('Ctrl Pts',(-0.1487162320301,2.36711739172401,9.61081552563933));
#92474=CARTESIAN_POINT('Ctrl Pts',(-0.126655034203364,2.36838414830745,
9.60934801565149));
#92475=CARTESIAN_POINT('Ctrl Pts',(-0.117344903516852,2.36886368138811,
9.60872719694399));
#92476=CARTESIAN_POINT('Ctrl Pts',(-0.0994612697117868,2.36967912039415,
9.60753167908212));
#92477=CARTESIAN_POINT('Ctrl Pts',(-0.0908882804715545,2.37002341653476,
9.60695725319674));
#92478=CARTESIAN_POINT('Ctrl Pts',(-0.0706803264661093,2.37072517444266,
9.60560003110327));
#92479=CARTESIAN_POINT('Ctrl Pts',(-0.0590443128458333,2.37104350908495,
9.60481602069325));
#92480=CARTESIAN_POINT('Ctrl Pts',(-0.018453770702516,2.37185499610628,
9.60207210368493));
#92481=CARTESIAN_POINT('Ctrl Pts',(0.0105060580608178,2.3719034881719,9.60009839474749));
#92482=CARTESIAN_POINT('Ctrl Pts',(0.199348752340831,2.36876130716535,9.58711812374626));
#92483=CARTESIAN_POINT('Ctrl Pts',(0.358530818626417,2.34993788862567,9.57562028805024));
#92484=CARTESIAN_POINT('Ctrl Pts',(0.629010982030408,2.2898219260021,9.55540219832456));
#92485=CARTESIAN_POINT('Ctrl Pts',(0.741403372251917,2.25593944473134,9.54679811897857));
#92486=CARTESIAN_POINT('Ctrl Pts',(0.881642877724792,2.20204298512529,9.53608940688557));
#92487=CARTESIAN_POINT('Ctrl Pts',(0.91220334418794,2.18955994830343,9.53375824717464));
#92488=CARTESIAN_POINT('Ctrl Pts',(0.962276262662096,2.16787618209389,9.52995362663431));
#92489=CARTESIAN_POINT('Ctrl Pts',(0.981940860696813,2.15904029043049,9.5284633827208));
#92490=CARTESIAN_POINT('Ctrl Pts',(1.00862514531156,2.14661022444421,9.52644917482649));
#92491=CARTESIAN_POINT('Ctrl Pts',(1.0157506886507,2.1432476950747,9.52591210702048));
#92492=CARTESIAN_POINT('Ctrl Pts',(1.02767198261674,2.13754925341554,9.52501506167504));
#92493=CARTESIAN_POINT('Ctrl Pts',(1.03247679351684,2.13523258387519,9.52465392047672));
#92494=CARTESIAN_POINT('Ctrl Pts',(1.04157043220184,2.13081015678448,9.52397125208002));
#92495=CARTESIAN_POINT('Ctrl Pts',(1.04586076690678,2.1287076236016,9.52364952299442));
#92496=CARTESIAN_POINT('Ctrl Pts',(1.05708453075358,2.12316515178113,9.52280870418981));
#92497=CARTESIAN_POINT('Ctrl Pts',(1.06400759976011,2.11970417718637,9.52229091402527));
#92498=CARTESIAN_POINT('Ctrl Pts',(1.08798775889966,2.10756894965,9.52049990127624));
#92499=CARTESIAN_POINT('Ctrl Pts',(1.10495727519752,2.09872192508316,9.51923692534458));
#92500=CARTESIAN_POINT('Ctrl Pts',(1.22821083714572,2.03255448285871,9.51008248028603));
#92501=CARTESIAN_POINT('Ctrl Pts',(1.33010087785581,1.96738889500319,9.50261310290126));
#92502=CARTESIAN_POINT('Ctrl Pts',(1.4489786919158,1.8778828294221,9.49347600666313));
#92503=CARTESIAN_POINT('Ctrl Pts',(1.47106272451258,1.8606336674621,9.4917594240051));
#92504=CARTESIAN_POINT('Ctrl Pts',(1.62676629172135,1.73451307769844,9.47948263031945));
#92505=CARTESIAN_POINT('Ctrl Pts',(1.74845382970668,1.61177010573905,9.46890531361234));
#92506=CARTESIAN_POINT('Ctrl Pts',(1.87074092980995,1.45811690787918,9.45612114315037));
#92507=CARTESIAN_POINT('Ctrl Pts',(1.88543076012493,1.4390716878166,9.45454465251164));
#92508=CARTESIAN_POINT('Ctrl Pts',(1.90682099968558,1.4104496440876,9.45218551511266));
#92509=CARTESIAN_POINT('Ctrl Pts',(1.91374467864785,1.40104097727905,9.45141160440398));
#92510=CARTESIAN_POINT('Ctrl Pts',(1.92597251759125,1.38416466384984,9.4500260497854));
#92511=CARTESIAN_POINT('Ctrl Pts',(1.93130349278154,1.37671666289269,9.44941545902557));
#92512=CARTESIAN_POINT('Ctrl Pts',(1.94247806415959,1.36091183212375,9.4481215475961));
#92513=CARTESIAN_POINT('Ctrl Pts',(1.9483111597683,1.35254784153293,9.44743784105016));
#92514=CARTESIAN_POINT('Ctrl Pts',(1.96369811552364,1.33017863186738,9.44561187905386));
#92515=CARTESIAN_POINT('Ctrl Pts',(1.9731559046308,1.31610836617445,9.44446601766467));
#92516=CARTESIAN_POINT('Ctrl Pts',(2.01435077393326,1.25338092329324,9.43936832574352));
#92517=CARTESIAN_POINT('Ctrl Pts',(2.04444230851287,1.20367246493395,9.43535623231626));
#92518=CARTESIAN_POINT('Ctrl Pts',(2.08873433556382,1.12404542988136,9.4289666005604));
#92519=CARTESIAN_POINT('Ctrl Pts',(2.10418634657431,1.09484652142193,9.42663124077175));
#92520=CARTESIAN_POINT('Ctrl Pts',(2.20569757851536,0.892933953617337,9.41053913073493));
#92521=CARTESIAN_POINT('Ctrl Pts',(2.27099862109687,0.7106234248208,9.39620940827867));
#92522=CARTESIAN_POINT('Ctrl Pts',(2.32710144998697,0.462181791152007,9.3779314621572));
#92523=CARTESIAN_POINT('Ctrl Pts',(2.33834956741056,0.401417499436738,9.37356259380762));
#92524=CARTESIAN_POINT('Ctrl Pts',(2.34880872559759,0.329270902366803,9.36854521282627));
#92525=CARTESIAN_POINT('Ctrl Pts',(2.35032698020423,0.318252816124755,9.36778362040301));
#92526=CARTESIAN_POINT('Ctrl Pts',(2.352550647189,0.3012308874422,9.36661462145224));
#92527=CARTESIAN_POINT('Ctrl Pts',(2.35331068267,0.295234530586414,9.36620426648454));
#92528=CARTESIAN_POINT('Ctrl Pts',(2.35467142248465,0.284159647507261,9.36544912624676));
#92529=CARTESIAN_POINT('Ctrl Pts',(2.35527862234446,0.279082111928869,9.36510399286932));
#92530=CARTESIAN_POINT('Ctrl Pts',(2.35661652340815,0.267578858182082,9.36432449836086));
#92531=CARTESIAN_POINT('Ctrl Pts',(2.35733736820994,0.261152098791384,9.36389069458228));
#92532=CARTESIAN_POINT('Ctrl Pts',(2.35913481146385,0.244512694488986,9.3627717312804));
#92533=CARTESIAN_POINT('Ctrl Pts',(2.36017139992501,0.234295729535626,9.3620887433842));
#92534=CARTESIAN_POINT('Ctrl Pts',(2.36642921652624,0.168354501121797,9.35770510325752));
#92535=CARTESIAN_POINT('Ctrl Pts',(2.36974344180738,0.112461846610562,9.35410177303053));
#92536=CARTESIAN_POINT('Ctrl Pts',(2.37140407190246,0.0427710456632706,
9.34969042645262));
#92537=CARTESIAN_POINT('Ctrl Pts',(2.37161196783422,0.029039983881964,9.34882520885645));
#92538=CARTESIAN_POINT('Ctrl Pts',(2.3725930481777,-0.122964073143172,9.3392834176185));
#92539=CARTESIAN_POINT('Ctrl Pts',(2.36139199002595,-0.261055317107764,
9.33093240578155));
#92540=CARTESIAN_POINT('Ctrl Pts',(2.31821498148863,-0.515106691217405,
9.31505383116086));
#92541=CARTESIAN_POINT('Ctrl Pts',(2.2893502809727,-0.631130404778904,9.30759351119729));
#92542=CARTESIAN_POINT('Ctrl Pts',(2.24312793718267,-0.770942248187741,
9.29803877405604));
#92543=CARTESIAN_POINT('Ctrl Pts',(2.23391370119492,-0.797247992177152,
9.29621612283714));
#92544=CARTESIAN_POINT('Ctrl Pts',(2.21993636764402,-0.835005474911228,
9.29356098745198));
#92545=CARTESIAN_POINT('Ctrl Pts',(2.21554344669009,-0.846592490807026,
9.29274081049707));
#92546=CARTESIAN_POINT('Ctrl Pts',(2.20771030289488,-0.866775051649364,
9.29130255072214));
#92547=CARTESIAN_POINT('Ctrl Pts',(2.20431014576016,-0.875385942765652,
9.29068582350849));
#92548=CARTESIAN_POINT('Ctrl Pts',(2.19762632783627,-0.892026819330015,
9.28948786743112));
#92549=CARTESIAN_POINT('Ctrl Pts',(2.19434884699582,-0.900059141069041,
9.2889068555393));
#92550=CARTESIAN_POINT('Ctrl Pts',(2.1864277805681,-0.919171337620204,9.28751766561146));
#92551=CARTESIAN_POINT('Ctrl Pts',(2.18174397115656,-0.930234176211502,
9.28670813182155));
#92552=CARTESIAN_POINT('Ctrl Pts',(2.16458174195331,-0.969927498892542,
9.28378364918555));
#92553=CARTESIAN_POINT('Ctrl Pts',(2.15162261820875,-0.998345339520149,
9.28165239554018));
#92554=CARTESIAN_POINT('Ctrl Pts',(2.05031897660155,-1.20935210231319,9.26553638234899));
#92555=CARTESIAN_POINT('Ctrl Pts',(1.93945180592142,-1.38015729330138,9.25072930718572));
#92556=CARTESIAN_POINT('Ctrl Pts',(1.80190608146297,-1.54221551038247,9.23522290546875));
#92557=CARTESIAN_POINT('Ctrl Pts',(1.79551481273734,-1.54965182077825,9.23450802531616));
#92558=CARTESIAN_POINT('Ctrl Pts',(1.72470893824493,-1.63100909300906,9.22665130722154));
#92559=CARTESIAN_POINT('Ctrl Pts',(1.65580844288439,-1.70091569263711,9.21957143679109));
#92560=CARTESIAN_POINT('Ctrl Pts',(1.56876772387876,-1.77890961465014,9.21144674283251));
#92561=CARTESIAN_POINT('Ctrl Pts',(1.55461543361571,-1.79129073525429,9.2101496888465));
#92562=CARTESIAN_POINT('Ctrl Pts',(1.53463913596735,-1.80835188380253,9.20835381458728));
#92563=CARTESIAN_POINT('Ctrl Pts',(1.52893845758087,-1.81317429114479,9.20784522651959));
#92564=CARTESIAN_POINT('Ctrl Pts',(1.51918905033865,-1.82134298764981,9.20698219471009));
#92565=CARTESIAN_POINT('Ctrl Pts',(1.51515183434381,-1.82470287179815,9.20662677256867));
#92566=CARTESIAN_POINT('Ctrl Pts',(1.50735621729631,-1.83114688995727,9.20594428490517));
#92567=CARTESIAN_POINT('Ctrl Pts',(1.50359947248328,-1.8342328984792,9.20561707614002));
#92568=CARTESIAN_POINT('Ctrl Pts',(1.49454753598834,-1.84162218744801,9.20483262764584));
#92569=CARTESIAN_POINT('Ctrl Pts',(1.48924317284971,-1.84591424330824,9.20437618918943));
#92570=CARTESIAN_POINT('Ctrl Pts',(1.46978982726902,-1.86151659589891,9.20271373241415));
#92571=CARTESIAN_POINT('Ctrl Pts',(1.45552947405767,-1.87268795389406,9.20151715240743));
#92572=CARTESIAN_POINT('Ctrl Pts',(1.31338811377681,-1.98143478227515,9.18979066995703));
#92573=CARTESIAN_POINT('Ctrl Pts',(1.17600210827924,-2.06593974715203,9.1800243688471));
#92574=CARTESIAN_POINT('Ctrl Pts',(0.881795074411039,-2.20796793785566,
9.16000188126156));
#92575=CARTESIAN_POINT('Ctrl Pts',(0.725367668171613,-2.26418109451874,
9.14977911098919));
#92576=CARTESIAN_POINT('Ctrl Pts',(0.543470229237293,-2.30874449922894,
9.13755865589627));
#92577=CARTESIAN_POINT('Ctrl Pts',(0.522502956301095,-2.31357983723299,
9.13614592234454));
#92578=CARTESIAN_POINT('Ctrl Pts',(0.490551404705045,-2.32049181277647,
9.13398561797963));
#92579=CARTESIAN_POINT('Ctrl Pts',(0.479613058329547,-2.32277726888243,
9.13324473605734));
#92580=CARTESIAN_POINT('Ctrl Pts',(0.459723931464479,-2.32678642145354,
9.13189501964167));
#92581=CARTESIAN_POINT('Ctrl Pts',(0.45077853689879,-2.32853598874835,9.13128702483692));
#92582=CARTESIAN_POINT('Ctrl Pts',(0.431473009342262,-2.33219640818158,
9.12997274569269));
#92583=CARTESIAN_POINT('Ctrl Pts',(0.421109820271893,-2.33408987769741,
9.12926592105249));
#92584=CARTESIAN_POINT('Ctrl Pts',(0.39299194474948,-2.33903397263712,9.12734437900463));
#92585=CARTESIAN_POINT('Ctrl Pts',(0.375214859107551,-2.3419514025647,9.12612546420861));
#92586=CARTESIAN_POINT('Ctrl Pts',(0.285959804033519,-2.35555690274467,
9.11998397377182));
#92587=CARTESIAN_POINT('Ctrl Pts',(0.214059881794555,-2.36317535496498,
9.11496578204031));
#92588=CARTESIAN_POINT('Ctrl Pts',(-0.0655618299436858,-2.37993856128543,
9.09516440347429));
#92589=CARTESIAN_POINT('Ctrl Pts',(-0.273782438354002,-2.36504308950549,
9.07971214783137));
#92590=CARTESIAN_POINT('Ctrl Pts',(-0.51898160293378,-2.31466257876956,
9.06173482832672));
#92591=CARTESIAN_POINT('Ctrl Pts',(-0.560382267570449,-2.30498957142429,
9.05871163232421));
#92592=CARTESIAN_POINT('Ctrl Pts',(-0.626572449331334,-2.28763561508439,
9.05392001808731));
#92593=CARTESIAN_POINT('Ctrl Pts',(-0.651533821969743,-2.2806520034939,
9.05212277039272));
#92594=CARTESIAN_POINT('Ctrl Pts',(-0.684476875384432,-2.27085025622631,
9.04976825552857));
#92595=CARTESIAN_POINT('Ctrl Pts',(-0.69256399944137,-2.2683969210278,9.04919165499968));
#92596=CARTESIAN_POINT('Ctrl Pts',(-0.705851263772948,-2.26428837223786,
9.04824680348178));
#92597=CARTESIAN_POINT('Ctrl Pts',(-0.711059024590557,-2.26265837110255,
9.04787711926342));
#92598=CARTESIAN_POINT('Ctrl Pts',(-0.721257578827817,-2.2594275905038,
9.04715446714972));
#92599=CARTESIAN_POINT('Ctrl Pts',(-0.726248753622761,-2.25782822209685,
9.04680142411276));
#92600=CARTESIAN_POINT('Ctrl Pts',(-0.738540945992169,-2.2538443431419,
9.04593339947194));
#92601=CARTESIAN_POINT('Ctrl Pts',(-0.745835845271915,-2.25144086044164,
9.04541952235339));
#92602=CARTESIAN_POINT('Ctrl Pts',(-0.77092710820583,-2.24303859621651,
9.04365593493442));
#92603=CARTESIAN_POINT('Ctrl Pts',(-0.788664384890333,-2.2368637180327,
9.04241605848102));
#92604=CARTESIAN_POINT('Ctrl Pts',(-0.944546952691713,-2.18051153217965,
9.03156427346055));
#92605=CARTESIAN_POINT('Ctrl Pts',(-1.07784418527555,-2.11779698370409,
9.0225844487537));
#92606=CARTESIAN_POINT('Ctrl Pts',(-1.35938433772344,-1.951820251428,9.00256000739569));
#92607=CARTESIAN_POINT('Ctrl Pts',(-1.50336804236012,-1.84320396967908,
8.99153373785449));
#92608=CARTESIAN_POINT('Ctrl Pts',(-1.64884126313963,-1.70498012457662,
8.97843151933963));
#92609=CARTESIAN_POINT('Ctrl Pts',(-1.6637988173455,-1.69038699284462,8.97705893090721));
#92610=CARTESIAN_POINT('Ctrl Pts',(-1.68636509985702,-1.6677808097898,8.97494759886285));
#92611=CARTESIAN_POINT('Ctrl Pts',(-1.6941141673487,-1.6599088108952,8.97421508177893));
#92612=CARTESIAN_POINT('Ctrl Pts',(-1.70753634483157,-1.64608181271799,
8.97293293578471));
#92613=CARTESIAN_POINT('Ctrl Pts',(-1.71323404026693,-1.64015085385968,
8.97238439351282));
#92614=CARTESIAN_POINT('Ctrl Pts',(-1.72601046993488,-1.62671214227964,
8.97114458379453));
#92615=CARTESIAN_POINT('Ctrl Pts',(-1.73307125040729,-1.61918762696858,
8.97045255751335));
#92616=CARTESIAN_POINT('Ctrl Pts',(-1.75197810223576,-1.59877367232673,
8.96858071473014));
#92617=CARTESIAN_POINT('Ctrl Pts',(-1.76373074192346,-1.58579896812263,
8.96739696667838));
#92618=CARTESIAN_POINT('Ctrl Pts',(-1.81760174686676,-1.52498665263576,
8.96187497913036));
#92619=CARTESIAN_POINT('Ctrl Pts',(-1.85792092575417,-1.47559780792352,
8.95746344392764));
#92620=CARTESIAN_POINT('Ctrl Pts',(-2.01351003323371,-1.2685096652912,8.93923915566434));
#92621=CARTESIAN_POINT('Ctrl Pts',(-2.1110752860731,-1.0984899039839,8.92480825251539));
#92622=CARTESIAN_POINT('Ctrl Pts',(-2.21655854128162,-0.847358704857114,
8.90507971733241));
#92623=CARTESIAN_POINT('Ctrl Pts',(-2.24294715210715,-0.774815532470435,
8.89956068515517));
#92624=CARTESIAN_POINT('Ctrl Pts',(-2.27069117934062,-0.685155802919529,
8.8930520889899));
#92625=CARTESIAN_POINT('Ctrl Pts',(-2.2754589910058,-0.669151198371343,
8.89190219002932));
#92626=CARTESIAN_POINT('Ctrl Pts',(-2.28201817632592,-0.646252119589848,
8.89027516723342));
#92627=CARTESIAN_POINT('Ctrl Pts',(-2.28394801826896,-0.639398320570791,
8.88979050839142));
#92628=CARTESIAN_POINT('Ctrl Pts',(-2.28723157933368,-0.627532244476332,
8.88895553632869));
#92629=CARTESIAN_POINT('Ctrl Pts',(-2.28859974949358,-0.622524059112043,
8.88860439746934));
#92630=CARTESIAN_POINT('Ctrl Pts',(-2.29142644237332,-0.612041676562383,
8.8878721402448));
#92631=CARTESIAN_POINT('Ctrl Pts',(-2.29288180459949,-0.606566720578268,
8.88749120401116));
#92632=CARTESIAN_POINT('Ctrl Pts',(-2.29669765174823,-0.592001820726257,
8.88648172038356));
#92633=CARTESIAN_POINT('Ctrl Pts',(-2.29902381830876,-0.582902864597313,
8.88585511915429));
#92634=CARTESIAN_POINT('Ctrl Pts',(-2.30883533425678,-0.543551889266812,
8.88316167265519));
#92635=CARTESIAN_POINT('Ctrl Pts',(-2.31577848234547,-0.513166161440208,
8.88112378289746));
#92636=CARTESIAN_POINT('Ctrl Pts',(-2.35497110526431,-0.324603234757285,
8.86868512712059));
#92637=CARTESIAN_POINT('Ctrl Pts',(-2.3716039949965,-0.16359555102086,8.85894060335103));
#92638=CARTESIAN_POINT('Ctrl Pts',(-2.37177458044386,0.0262972234964526,
8.84728189501136));
#92639=CARTESIAN_POINT('Ctrl Pts',(-2.3712890111722,0.0547228818911722,
8.84553307096252));
#92640=CARTESIAN_POINT('Ctrl Pts',(-2.36923976809993,0.113151281512263,
8.84192204702261));
#92641=CARTESIAN_POINT('Ctrl Pts',(-2.36761709190539,0.143138040807685,
8.84005990011078));
#92642=CARTESIAN_POINT('Ctrl Pts',(-2.36542648836857,0.173076834453233,
8.83818724301668));
#92643=CARTESIAN_POINT('Ctrl Pts',(-2.36542651242649,0.173076505655319,
8.63818628587103));
#92644=CARTESIAN_POINT('Ctrl Pts',(-2.36962632261321,0.115677944682464,
8.64182253402733));
#92645=CARTESIAN_POINT('Ctrl Pts',(-2.37173733137448,0.0581212205746936,
8.64550929040616));
#92646=CARTESIAN_POINT('Ctrl Pts',(-2.37175497626484,-0.0224685146569301,
8.65075947075785));
#92647=CARTESIAN_POINT('Ctrl Pts',(-2.37142580119415,-0.0454544850129582,
8.65226686390312));
#92648=CARTESIAN_POINT('Ctrl Pts',(-2.37042425669134,-0.0801523632701318,
8.65455888830174));
#92649=CARTESIAN_POINT('Ctrl Pts',(-2.36999902211517,-0.0918704786881775,
8.6553358016766));
#92650=CARTESIAN_POINT('Ctrl Pts',(-2.36908166996873,-0.112854776213844,
8.65673238966705));
#92651=CARTESIAN_POINT('Ctrl Pts',(-2.36862203074418,-0.122122196023677,
8.65735103490929));
#92652=CARTESIAN_POINT('Ctrl Pts',(-2.36753077267549,-0.141791002591501,
8.65866808656538));
#92653=CARTESIAN_POINT('Ctrl Pts',(-2.36688496297963,-0.15219137290288,
8.65936692527951));
#92654=CARTESIAN_POINT('Ctrl Pts',(-2.36496793368108,-0.180090394642471,
8.66124821789653));
#92655=CARTESIAN_POINT('Ctrl Pts',(-2.36357106943291,-0.197579473713945,
8.66243458326398));
#92656=CARTESIAN_POINT('Ctrl Pts',(-2.35553516918909,-0.285840558268255,
8.66845856914897));
#92657=CARTESIAN_POINT('Ctrl Pts',(-2.3459115789052,-0.356297308643696,
8.67338878018612));
#92658=CARTESIAN_POINT('Ctrl Pts',(-2.30635524148394,-0.572835056575161,
8.68892982256238));
#92659=CARTESIAN_POINT('Ctrl Pts',(-2.2658105080888,-0.716594330411137,
8.6998280447763));
#92660=CARTESIAN_POINT('Ctrl Pts',(-2.20053914221121,-0.885349883215016,
8.71303297864381));
#92661=CARTESIAN_POINT('Ctrl Pts',(-2.1884245001186,-0.914885347992949,
8.71535883541839));
#92662=CARTESIAN_POINT('Ctrl Pts',(-2.16660252609903,-0.965171378149387,
8.71933637498095));
#92663=CARTESIAN_POINT('Ctrl Pts',(-2.15718397326766,-0.986042414329511,
8.72099254777867));
#92664=CARTESIAN_POINT('Ctrl Pts',(-2.13821088330868,-1.02651230058111,
8.72421066881572));
#92665=CARTESIAN_POINT('Ctrl Pts',(-2.12868532350061,-1.04612242540049,
8.72577318698067));
#92666=CARTESIAN_POINT('Ctrl Pts',(-2.09734896757605,-1.10843321121665,
8.73074253412488));
#92667=CARTESIAN_POINT('Ctrl Pts',(-2.07451162863634,-1.15060816663103,
8.73411298027638));
#92668=CARTESIAN_POINT('Ctrl Pts',(-2.04494996107893,-1.20145566246044,
8.73816000155135));
#92669=CARTESIAN_POINT('Ctrl Pts',(-2.03942587868433,-1.21080888208674,
8.7389037264827));
#92670=CARTESIAN_POINT('Ctrl Pts',(-2.03069630302183,-1.22536030356853,
8.74005928066867));
#92671=CARTESIAN_POINT('Ctrl Pts',(-2.02753475108883,-1.2305844887444,8.74047383616278));
#92672=CARTESIAN_POINT('Ctrl Pts',(-2.02164832336969,-1.24022702121712,
8.74123834963527));
#92673=CARTESIAN_POINT('Ctrl Pts',(-2.0189291356747,-1.24464860646999,8.74158865283869));
#92674=CARTESIAN_POINT('Ctrl Pts',(-2.01271849882378,-1.25467362009719,
8.74238232236784));
#92675=CARTESIAN_POINT('Ctrl Pts',(-2.00921815909397,-1.26027141533578,
8.74282509780112));
#92676=CARTESIAN_POINT('Ctrl Pts',(-1.99845141842993,-1.27733087203546,
8.74417349284185));
#92677=CARTESIAN_POINT('Ctrl Pts',(-1.99110982302307,-1.28874509607784,
8.74507432908905));
#92678=CARTESIAN_POINT('Ctrl Pts',(-1.90625401701813,-1.41821703789537,
8.75528466789832));
#92679=CARTESIAN_POINT('Ctrl Pts',(-1.81842875071117,-1.52920678757551,
8.76397154266167));
#92680=CARTESIAN_POINT('Ctrl Pts',(-1.59684677354469,-1.76294258663607,
8.78372151378255));
#92681=CARTESIAN_POINT('Ctrl Pts',(-1.4578819743076,-1.87948316306415,8.79474049263908));
#92682=CARTESIAN_POINT('Ctrl Pts',(-1.28333160107688,-1.99475940035968,
8.80830047156384));
#92683=CARTESIAN_POINT('Ctrl Pts',(-1.25934829473174,-2.00998677191907,
8.81015661926821));
#92684=CARTESIAN_POINT('Ctrl Pts',(-1.22515973721308,-2.03084150125402,
8.81279578483931));
#92685=CARTESIAN_POINT('Ctrl Pts',(-1.21517703997988,-2.03683046380086,
8.81356558613831));
#92686=CARTESIAN_POINT('Ctrl Pts',(-1.19768972217314,-2.04714738975556,
8.81491290231444));
#92687=CARTESIAN_POINT('Ctrl Pts',(-1.19020466524666,-2.05150821528912,
8.81548921353275));
#92688=CARTESIAN_POINT('Ctrl Pts',(-1.1744668651392,-2.0605620047019,8.81670024755024));
#92689=CARTESIAN_POINT('Ctrl Pts',(-1.16620951489329,-2.06524660885105,
8.81733525835841));
#92690=CARTESIAN_POINT('Ctrl Pts',(-1.14643828797032,-2.07630694534312,
8.81885489271948));
#92691=CARTESIAN_POINT('Ctrl Pts',(-1.13489913327376,-2.08263660404983,
8.81974114352013));
#92692=CARTESIAN_POINT('Ctrl Pts',(-1.09534574361167,-2.10390678712963,
8.82277715546308));
#92693=CARTESIAN_POINT('Ctrl Pts',(-1.06708552786829,-2.11838012938699,
8.82494326916661));
#92694=CARTESIAN_POINT('Ctrl Pts',(-0.998388615044404,-2.15183950443047,
8.83020408755262));
#92695=CARTESIAN_POINT('Ctrl Pts',(-0.957690724404734,-2.17025830378376,
8.83331702416739));
#92696=CARTESIAN_POINT('Ctrl Pts',(-0.797154893031354,-2.23751768285175,
8.84558287365063));
#92697=CARTESIAN_POINT('Ctrl Pts',(-0.673931672605224,-2.27766332592869,
8.85498532734097));
#92698=CARTESIAN_POINT('Ctrl Pts',(-0.416445526935439,-2.33881853555108,
8.87431531214732));
#92699=CARTESIAN_POINT('Ctrl Pts',(-0.28237934662137,-2.35876413175264,
8.88421102616375));
#92700=CARTESIAN_POINT('Ctrl Pts',(-0.128208483058595,-2.36835972722455,
8.89495821683115));
#92701=CARTESIAN_POINT('Ctrl Pts',(-0.10906982688684,-2.36931826574877,
8.89628103808177));
#92702=CARTESIAN_POINT('Ctrl Pts',(-0.0821183035926551,-2.37034082252714,
8.89812601441873));
#92703=CARTESIAN_POINT('Ctrl Pts',(-0.0743141473511144,-2.37059833008507,
8.8986581453927));
#92704=CARTESIAN_POINT('Ctrl Pts',(-0.0611909234637201,-2.37096647690985,
8.89954926241502));
#92705=CARTESIAN_POINT('Ctrl Pts',(-0.0558725492665126,-2.37109776768551,
8.89990937936327));
#92706=CARTESIAN_POINT('Ctrl Pts',(-0.0450201580608888,-2.37132913820439,
8.90064207217382));
#92707=CARTESIAN_POINT('Ctrl Pts',(-0.039486163225334,-2.37142774312308,
8.90101456435898));
#92708=CARTESIAN_POINT('Ctrl Pts',(-0.0253823291256551,-2.37162966138745,
8.90196112153543));
#92709=CARTESIAN_POINT('Ctrl Pts',(-0.0168120891537472,-2.37170589929428,
8.90253369478753));
#92710=CARTESIAN_POINT('Ctrl Pts',(0.0180461933905542,-2.37182702708564,
8.90485265002706));
#92711=CARTESIAN_POINT('Ctrl Pts',(0.0443349192699614,-2.37148132396956,
8.90657859828215));
#92712=CARTESIAN_POINT('Ctrl Pts',(0.11378101368949,-2.36941279742469,8.91109027499615));
#92713=CARTESIAN_POINT('Ctrl Pts',(0.156907818014744,-2.36694814654502,
8.91384339670428));
#92714=CARTESIAN_POINT('Ctrl Pts',(0.416495358282921,-2.34498593478084,
8.93024855392571));
#92715=CARTESIAN_POINT('Ctrl Pts',(0.629501782824453,-2.29699064208031,
8.94310846051508));
#92716=CARTESIAN_POINT('Ctrl Pts',(0.89168089883922,-2.1986429226313,8.96084089238226));
#92717=CARTESIAN_POINT('Ctrl Pts',(0.949457878661102,-2.17431694421023,
8.96486891190848));
#92718=CARTESIAN_POINT('Ctrl Pts',(1.02209700695599,-2.14028594916207,8.97012465307386));
#92719=CARTESIAN_POINT('Ctrl Pts',(1.03791023769322,-2.13266231428339,8.97128069528669));
#92720=CARTESIAN_POINT('Ctrl Pts',(1.06297477228998,-2.12023379092967,8.97313280939849));
#92721=CARTESIAN_POINT('Ctrl Pts',(1.07228175556549,-2.11554213512653,8.97382492829369));
#92722=CARTESIAN_POINT('Ctrl Pts',(1.0889891192128,-2.10698136965817,8.97507545698759));
#92723=CARTESIAN_POINT('Ctrl Pts',(1.0964006049871,-2.10313420973515,8.97563308689087));
#92724=CARTESIAN_POINT('Ctrl Pts',(1.1137693626783,-2.09400165966002,8.97694677865921));
#92725=CARTESIAN_POINT('Ctrl Pts',(1.12370950261315,-2.08868429639477,8.97770396368377));
#92726=CARTESIAN_POINT('Ctrl Pts',(1.15251948421948,-2.07300754541329,8.97991442872988));
#92727=CARTESIAN_POINT('Ctrl Pts',(1.17128624230547,-2.0624621039113,8.98137431009816));
#92728=CARTESIAN_POINT('Ctrl Pts',(1.34065740498663,-1.96423163348068,8.99473678233262));
#92729=CARTESIAN_POINT('Ctrl Pts',(1.48128218888033,-1.860469746035,9.00724920071136));
#92730=CARTESIAN_POINT('Ctrl Pts',(1.64497509807223,-1.70927472136154,9.02351044388771));
#92731=CARTESIAN_POINT('Ctrl Pts',(1.6796766227282,-1.67518643919963,9.0270669025429));
#92732=CARTESIAN_POINT('Ctrl Pts',(1.79051095765451,-1.55940188045593,9.03875070838621));
#92733=CARTESIAN_POINT('Ctrl Pts',(1.86193490647083,-1.47338669467082,9.04682115229852));
#92734=CARTESIAN_POINT('Ctrl Pts',(1.93448386768207,-1.37227304613091,9.05540904303976));
#92735=CARTESIAN_POINT('Ctrl Pts',(1.94184490158232,-1.36183682720062,9.05628533974151));
#92736=CARTESIAN_POINT('Ctrl Pts',(1.95284029734137,-1.34597750213653,9.05760123061125));
#92737=CARTESIAN_POINT('Ctrl Pts',(1.95653701051005,-1.34059822179549,9.05804485387336));
#92738=CARTESIAN_POINT('Ctrl Pts',(1.96313110165603,-1.33091744141755,9.05883826814351));
#92739=CARTESIAN_POINT('Ctrl Pts',(1.96603660770064,-1.32662165556134,9.05918859794148));
#92740=CARTESIAN_POINT('Ctrl Pts',(1.97236517538594,-1.31719842202372,9.05995326957908));
#92741=CARTESIAN_POINT('Ctrl Pts',(1.97578234046013,-1.31206715276877,9.06036721680782));
#92742=CARTESIAN_POINT('Ctrl Pts',(1.98548368259754,-1.29737561833183,9.06154562784371));
#92743=CARTESIAN_POINT('Ctrl Pts',(1.99171885554696,-1.28778296404881,9.06230690528831));
#92744=CARTESIAN_POINT('Ctrl Pts',(2.033778286188,-1.22203935582186,9.06747174443961));
#92745=CARTESIAN_POINT('Ctrl Pts',(2.06729661304694,-1.16444016649089,9.07173687960242));
#92746=CARTESIAN_POINT('Ctrl Pts',(2.21595558095432,-0.882270802454319,
9.09179224375771));
#92747=CARTESIAN_POINT('Ctrl Pts',(2.29718953497639,-0.641712378138874,
9.10662158362829));
#92748=CARTESIAN_POINT('Ctrl Pts',(2.34448585980821,-0.360119479720636,
9.12506045220821));
#92749=CARTESIAN_POINT('Ctrl Pts',(2.34929619407533,-0.327272365608154,
9.12722363898407));
#92750=CARTESIAN_POINT('Ctrl Pts',(2.35512525281256,-0.280665160301797,
9.13031531517297));
#92751=CARTESIAN_POINT('Ctrl Pts',(2.35671589341879,-0.266979536440849,
9.13122584416864));
#92752=CARTESIAN_POINT('Ctrl Pts',(2.35911096424843,-0.244680099184098,
9.13271417619122));
#92753=CARTESIAN_POINT('Ctrl Pts',(2.35998767860667,-0.23607423833236,9.13328969659055));
#92754=CARTESIAN_POINT('Ctrl Pts',(2.36172887365599,-0.218002606303909,
9.13450072547387));
#92755=CARTESIAN_POINT('Ctrl Pts',(2.36258356729768,-0.208536068825818,
9.13513653047752));
#92756=CARTESIAN_POINT('Ctrl Pts',(2.3644911755096,-0.185888135289726,9.13666117663078));
#92757=CARTESIAN_POINT('Ctrl Pts',(2.36549079185537,-0.172702690214517,
9.13755167303423));
#92758=CARTESIAN_POINT('Ctrl Pts',(2.36854097440014,-0.127452235392275,
9.14061793002016));
#92759=CARTESIAN_POINT('Ctrl Pts',(2.37005011931908,-0.0953555181348098,
9.14281048671159));
#92760=CARTESIAN_POINT('Ctrl Pts',(2.3721164954073,-0.0178850345327514,
9.14814766429079));
#92761=CARTESIAN_POINT('Ctrl Pts',(2.37202450810648,0.0274918853529142,
9.15131122205681));
#92762=CARTESIAN_POINT('Ctrl Pts',(2.36654545312782,0.205822125817044,9.16389161436422));
#92763=CARTESIAN_POINT('Ctrl Pts',(2.35127696754213,0.338214631970212,9.17357235665783));
#92764=CARTESIAN_POINT('Ctrl Pts',(2.29924680597671,0.596359174655232,9.19280747632642));
#92765=CARTESIAN_POINT('Ctrl Pts',(2.26301158391534,0.721779510893022,9.20232486185348));
#92766=CARTESIAN_POINT('Ctrl Pts',(2.20981690241613,0.861554682222548,9.21273077038045));
#92767=CARTESIAN_POINT('Ctrl Pts',(2.20276478514976,0.879428549291975,9.21405724569522));
#92768=CARTESIAN_POINT('Ctrl Pts',(2.19253888584593,0.904451436174484,9.2159064167852));
#92769=CARTESIAN_POINT('Ctrl Pts',(2.18954600424891,0.911672894195848,9.21643914756089));
#92770=CARTESIAN_POINT('Ctrl Pts',(2.18445569023125,0.923785537526782,9.21733097998198));
#92771=CARTESIAN_POINT('Ctrl Pts',(2.18237741984973,0.928684651099779,9.21769121649204));
#92772=CARTESIAN_POINT('Ctrl Pts',(2.17810495260959,0.938662604725189,9.21842387195382));
#92773=CARTESIAN_POINT('Ctrl Pts',(2.17590944741803,0.943740826889446,9.2187962087721));
#92774=CARTESIAN_POINT('Ctrl Pts',(2.17027195784503,0.956656132955809,9.21974189108977));
#92775=CARTESIAN_POINT('Ctrl Pts',(2.16680524346824,0.964482436476965,9.22031375029429));
#92776=CARTESIAN_POINT('Ctrl Pts',(2.15255621023962,0.996185817704722,9.22262609215604));
#92777=CARTESIAN_POINT('Ctrl Pts',(2.14142049797384,1.01990333591292,9.22434628745731));
#92778=CARTESIAN_POINT('Ctrl Pts',(2.11098443126376,1.08203056511512,9.22883923747315));
#92779=CARTESIAN_POINT('Ctrl Pts',(2.0910284398587,1.12010978881651,9.23157972017456));
#92780=CARTESIAN_POINT('Ctrl Pts',(1.96566184749095,1.34428785871322,9.24775714819749));
#92781=CARTESIAN_POINT('Ctrl Pts',(1.83650935308992,1.51597513370259,9.26042220332708));
#92782=CARTESIAN_POINT('Ctrl Pts',(1.63980411836318,1.71480915078621,9.27810206327147));
#92783=CARTESIAN_POINT('Ctrl Pts',(1.59160325287495,1.75963797673998,9.28232564652624));
#92784=CARTESIAN_POINT('Ctrl Pts',(1.5280081836301,1.81403118618313,9.2878065983153));
#92785=CARTESIAN_POINT('Ctrl Pts',(1.51428108923734,1.82550565798871,9.28898445816654));
#92786=CARTESIAN_POINT('Ctrl Pts',(1.49229675273782,1.84346376125227,9.29086338480878));
#92787=CARTESIAN_POINT('Ctrl Pts',(1.48412382836435,1.85004991644244,9.29156029416924));
#92788=CARTESIAN_POINT('Ctrl Pts',(1.46937868866442,1.86177170892422,9.29281490488252));
#92789=CARTESIAN_POINT('Ctrl Pts',(1.46282255230251,1.8669273698413,9.29337179253914));
#92790=CARTESIAN_POINT('Ctrl Pts',(1.44742237804409,1.87890694384315,9.29467777707004));
#92791=CARTESIAN_POINT('Ctrl Pts',(1.43855711548826,1.88570312142178,9.2954279550198));
#92792=CARTESIAN_POINT('Ctrl Pts',(1.41286165109868,1.90511480462051,9.29759786609441));
#92793=CARTESIAN_POINT('Ctrl Pts',(1.39591157639649,1.91756910828018,9.29902383426654));
#92794=CARTESIAN_POINT('Ctrl Pts',(1.23429796531139,2.03303862780482,9.31257303714797));
#92795=CARTESIAN_POINT('Ctrl Pts',(1.07868877385576,2.11970354443408,9.32533261465925));
#92796=CARTESIAN_POINT('Ctrl Pts',(0.777641943609366,2.24557477326343,9.34914951043757));
#92797=CARTESIAN_POINT('Ctrl Pts',(0.635270787945736,2.28992841935837,9.36007722903795));
#92798=CARTESIAN_POINT('Ctrl Pts',(0.471345468078818,2.32451764902733,9.3717278269597));
#92799=CARTESIAN_POINT('Ctrl Pts',(0.452973753577782,2.32816745201715,9.37302038375747));
#92800=CARTESIAN_POINT('Ctrl Pts',(0.427708913268281,2.33287627537178,9.37477813671027));
#92801=CARTESIAN_POINT('Ctrl Pts',(0.420852098504893,2.33412299268297,9.37525319544622));
#92802=CARTESIAN_POINT('Ctrl Pts',(0.409121321794179,2.33620252830729,9.37606242005481));
#92803=CARTESIAN_POINT('Ctrl Pts',(0.404250120019786,2.33705035265215,9.37639741610734));
#92804=CARTESIAN_POINT('Ctrl Pts',(0.394131223301339,2.33877894517377,9.37709110375955));
#92805=CARTESIAN_POINT('Ctrl Pts',(0.388883184150452,2.33965729227496,9.37744964475139));
#92806=CARTESIAN_POINT('Ctrl Pts',(0.376195269292256,2.34173695695617,9.37831358652662));
#92807=CARTESIAN_POINT('Ctrl Pts',(0.368752451929149,2.34292050426898,9.37881798971167));
#92808=CARTESIAN_POINT('Ctrl Pts',(0.342684314513197,2.34693852754792,9.38057667982159));
#92809=CARTESIAN_POINT('Ctrl Pts',(0.324030374661536,2.34958663666366,9.38182096909038));
#92810=CARTESIAN_POINT('Ctrl Pts',(0.208803179687195,2.36454581840011,9.38943069511205));
#92811=CARTESIAN_POINT('Ctrl Pts',(0.111567831877113,2.37112481919005,9.39552395343879));
#92812=CARTESIAN_POINT('Ctrl Pts',(-0.158034189348343,2.3727381803667,9.41217307620285));
#92813=CARTESIAN_POINT('Ctrl Pts',(-0.329852312699817,2.35500684364521,
9.42254311645145));
#92814=CARTESIAN_POINT('Ctrl Pts',(-0.559948787033967,2.30556713860022,
9.43744291146647));
#92815=CARTESIAN_POINT('Ctrl Pts',(-0.621103668563766,2.28984968856897,
9.44149924988571));
#92816=CARTESIAN_POINT('Ctrl Pts',(-0.698410960853611,2.26665610282416,
9.44678723255796));
#92817=CARTESIAN_POINT('Ctrl Pts',(-0.715209687019322,2.26141169064095,
9.4479460862781));
#92818=CARTESIAN_POINT('Ctrl Pts',(-0.741871104669624,2.25276145144577,
9.44980165574627));
#92819=CARTESIAN_POINT('Ctrl Pts',(-0.75177259382262,2.24947657340868,9.45049439239136));
#92820=CARTESIAN_POINT('Ctrl Pts',(-0.769558860075498,2.24344532612811,
9.45174543990293));
#92821=CARTESIAN_POINT('Ctrl Pts',(-0.777451462484111,2.24072242610582,
9.45230296648972));
#92822=CARTESIAN_POINT('Ctrl Pts',(-0.793679845935531,2.23502766883712,
9.45345430773837));
#92823=CARTESIAN_POINT('Ctrl Pts',(-0.802013688984742,2.23205072014589,
9.45404828429249));
#92824=CARTESIAN_POINT('Ctrl Pts',(-0.826656222314673,2.22309228393259,
9.45581282414033));
#92825=CARTESIAN_POINT('Ctrl Pts',(-0.842915779074156,2.21697829807081,
9.45698778294039));
#92826=CARTESIAN_POINT('Ctrl Pts',(-0.92593641094033,2.18471521853626,9.46304330273811));
#92827=CARTESIAN_POINT('Ctrl Pts',(-0.991547559256512,2.15572965950817,
9.46801827281449));
#92828=CARTESIAN_POINT('Ctrl Pts',(-1.19255304698623,2.0558108882291,9.483873936327));
#92829=CARTESIAN_POINT('Ctrl Pts',(-1.32246130990822,1.97474731860099,9.49505906586337));
#92830=CARTESIAN_POINT('Ctrl Pts',(-1.53618215957587,1.81078504311349,9.51470779779012));
#92831=CARTESIAN_POINT('Ctrl Pts',(-1.62335960850776,1.73306332172986,9.52315324084593));
#92832=CARTESIAN_POINT('Ctrl Pts',(-1.71335438094739,1.64005425639804,9.53208431524276));
#92833=CARTESIAN_POINT('Ctrl Pts',(-1.72216187966619,1.63080338396,9.53296075133178));
#92834=CARTESIAN_POINT('Ctrl Pts',(-1.73535697456397,1.61671792208454,9.53427680962436));
#92835=CARTESIAN_POINT('Ctrl Pts',(-1.73979987481099,1.61193581353731,9.5347204624079));
#92836=CARTESIAN_POINT('Ctrl Pts',(-1.74773724408093,1.60332139137802,9.5355139078793));
#92837=CARTESIAN_POINT('Ctrl Pts',(-1.75123892213695,1.59949591986223,9.53586423954936));
#92838=CARTESIAN_POINT('Ctrl Pts',(-1.75887548206202,1.59109808069195,9.53662889003227));
#92839=CARTESIAN_POINT('Ctrl Pts',(-1.76300509074128,1.58652107328972,9.53704281439525));
#92840=CARTESIAN_POINT('Ctrl Pts',(-1.77151072676885,1.57701972218525,9.5378963771138));
#92841=CARTESIAN_POINT('Ctrl Pts',(-1.77588418336301,1.5720931362526,9.53833582740061));
#92842=CARTESIAN_POINT('Ctrl Pts',(-1.79859711824453,1.54629187080716,9.54062140092057));
#92843=CARTESIAN_POINT('Ctrl Pts',(-1.81659018403407,1.52511324645551,9.54244349859954));
#92844=CARTESIAN_POINT('Ctrl Pts',(-1.89607076218975,1.42815810455137,9.55057102023391));
#92845=CARTESIAN_POINT('Ctrl Pts',(-1.95322441610578,1.34893971075471,9.55663748857416));
#92846=CARTESIAN_POINT('Ctrl Pts',(-2.05489644764827,1.18794466448773,9.56835860503939));
#92847=CARTESIAN_POINT('Ctrl Pts',(-2.09980461433089,1.10663117327879,9.57400927256932));
#92848=CARTESIAN_POINT('Ctrl Pts',(-2.19357494328737,0.910469576203566,
9.58742649032757));
#92849=CARTESIAN_POINT('Ctrl Pts',(-2.23836674049381,0.793998641665065,
9.59524060475712));
#92850=CARTESIAN_POINT('Ctrl Pts',(-2.27915308345591,0.656516160423915,
9.60460404083347));
#92851=CARTESIAN_POINT('Ctrl Pts',(-2.28429062017896,0.638410977156685,
9.60583949042992));
#92852=CARTESIAN_POINT('Ctrl Pts',(-2.29230306591027,0.608838585120078,
9.60786220334127));
#92853=CARTESIAN_POINT('Ctrl Pts',(-2.2953087255795,0.597407410754678,9.60864523114045));
#92854=CARTESIAN_POINT('Ctrl Pts',(-2.30052362662366,0.576953540634747,
9.6100485738735));
#92855=CARTESIAN_POINT('Ctrl Pts',(-2.30276555769597,0.567939368923619,
9.61066781937295));
#92856=CARTESIAN_POINT('Ctrl Pts',(-2.3073969372521,0.548839560944614,9.61198167872364));
#92857=CARTESIAN_POINT('Ctrl Pts',(-2.30977333362695,0.538750991688016,
9.61267669833822));
#92858=CARTESIAN_POINT('Ctrl Pts',(-2.3144740352816,0.518192077350102,9.61409527194614));
#92859=CARTESIAN_POINT('Ctrl Pts',(-2.31679359562083,0.507720905336232,
9.61481896064311));
#92860=CARTESIAN_POINT('Ctrl Pts',(-2.32239524507094,0.481595485183429,
9.61662762177996));
#92861=CARTESIAN_POINT('Ctrl Pts',(-2.32559010917364,0.465923285432438,
9.61771534497657));
#92862=CARTESIAN_POINT('Ctrl Pts',(-2.34634386083236,0.35858088256934,9.62518513949623));
#92863=CARTESIAN_POINT('Ctrl Pts',(-2.35862460268534,0.266037904201847,
9.63172812560892));
#92864=CARTESIAN_POINT('Ctrl Pts',(-2.36542652525385,0.173076330344439,
9.63839747301829));
#92865=CARTESIAN_POINT('Origin',(0.,0.,-1.84858989190503));
#92866=CARTESIAN_POINT('',(-2.36516017494062,0.173060140022867,10.8371116396001));
#92867=CARTESIAN_POINT('',(-2.36916488281964,0.173362644194442,10.6397478783738));
#92868=CARTESIAN_POINT('',(-2.36542649454111,0.173076750093529,-1.84858989190503));
#92869=CARTESIAN_POINT('',(-2.37536570805869,0.000359094737715843,9.84846194679725));
#92870=CARTESIAN_POINT('Ctrl Pts',(-2.37558966658059,0.000367530682965326,
9.84859046225436));
#92871=CARTESIAN_POINT('Ctrl Pts',(-2.37390141785161,-0.765575782524014,
9.90022107850398));
#92872=CARTESIAN_POINT('Ctrl Pts',(-1.55507573763911,-2.32069515122134,
10.0048399834818));
#92873=CARTESIAN_POINT('Ctrl Pts',(1.09527631218182,-2.58173452929509,10.162447177188));
#92874=CARTESIAN_POINT('Ctrl Pts',(2.7636678171772,-0.476574837858771,10.3214120433727));
#92875=CARTESIAN_POINT('Ctrl Pts',(1.89670849126738,2.06578805276227,10.4803769095575));
#92876=CARTESIAN_POINT('Ctrl Pts',(-0.710265108221614,2.71302540640962,
10.6393417757422));
#92877=CARTESIAN_POINT('Ctrl Pts',(-2.17296599975294,1.33539974380505,10.7582533524231));
#92878=CARTESIAN_POINT('Ctrl Pts',(-2.35302712705762,0.365443290256533,
10.8241766403757));
#92879=CARTESIAN_POINT('Ctrl Pts',(-2.36516017494062,0.173060140022867,
10.8371116396001));
#92880=CARTESIAN_POINT('Ctrl Pts',(-2.3717499895258,0.000222899859654739,
9.84638711742221));
#92881=CARTESIAN_POINT('Ctrl Pts',(-2.37174950122911,0.00541858581568568,
9.84602924011033));
#92882=CARTESIAN_POINT('Ctrl Pts',(-2.37173193999369,0.0106143209615235,
9.84567219836226));
#92883=CARTESIAN_POINT('Ctrl Pts',(-2.3716568922996,0.0218723968884325,
9.8449004406146));
#92884=CARTESIAN_POINT('Ctrl Pts',(-2.3715932349913,0.0279346790041509,
9.84448604178746));
#92885=CARTESIAN_POINT('Ctrl Pts',(-2.37143325691739,0.0390942518433647,
9.84372546045836));
#92886=CARTESIAN_POINT('Ctrl Pts',(-2.37134374517283,0.044191583019491,
9.84337891679726));
#92887=CARTESIAN_POINT('Ctrl Pts',(-2.37113535589589,0.0542170263237478,
9.84269908764649));
#92888=CARTESIAN_POINT('Ctrl Pts',(-2.37101754869356,0.0591451400162158,
9.84236574627927));
#92889=CARTESIAN_POINT('Ctrl Pts',(-2.37075013236532,0.0690403132418933,
9.84169814098856));
#92890=CARTESIAN_POINT('Ctrl Pts',(-2.37060027827655,0.0740072750536078,
9.84136388963095));
#92891=CARTESIAN_POINT('Ctrl Pts',(-2.37014416960029,0.0876975882252386,
9.8404448768716));
#92892=CARTESIAN_POINT('Ctrl Pts',(-2.36980536385545,0.0964198896047411,
9.83986190791111));
#92893=CARTESIAN_POINT('Ctrl Pts',(-2.36841278027883,0.127802845351948,
9.8377729058658));
#92894=CARTESIAN_POINT('Ctrl Pts',(-2.36708203068683,0.150450666234089,
9.83628136334072));
#92895=CARTESIAN_POINT('Ctrl Pts',(-2.36542649454068,0.173076750099461,
9.83480414144792));
#92896=CARTESIAN_POINT('',(-2.37115431906008,-0.00217150823245576,9.65141047674274));
#92897=CARTESIAN_POINT('Ctrl Pts',(-2.36542652525385,0.173076330344439,
9.63839747301829));
#92898=CARTESIAN_POINT('Ctrl Pts',(-2.36969210259616,0.114778874124177,
9.64257991069099));
#92899=CARTESIAN_POINT('Ctrl Pts',(-2.37180304718333,0.0563167111270467,
9.64681082413871));
#92900=CARTESIAN_POINT('Ctrl Pts',(-2.37174898760129,-0.00219141786265223,
9.65106845735155));
#92901=CARTESIAN_POINT('Ctrl Pts',(-2.37115431906008,-0.00217150823245576,
9.65141047674274));
#92902=CARTESIAN_POINT('Ctrl Pts',(-2.37298013798662,-0.205892024950704,
9.66507633933387));
#92903=CARTESIAN_POINT('Ctrl Pts',(-2.25564024368453,-1.1970881612814,9.73170618041963));
#92904=CARTESIAN_POINT('Ctrl Pts',(-0.868335570250338,-2.66618442166349,
9.8513));
#92905=CARTESIAN_POINT('Ctrl Pts',(1.77076269460301,-2.17415397621359,10.0101919354839));
#92906=CARTESIAN_POINT('Ctrl Pts',(2.78675196561196,0.310740269422676,10.1690838709677));
#92907=CARTESIAN_POINT('Ctrl Pts',(1.24836046454784,2.51080508670764,10.3279758064516));
#92908=CARTESIAN_POINT('Ctrl Pts',(-1.40046442942458,2.41070497057955,10.4848638089203));
#92909=CARTESIAN_POINT('Ctrl Pts',(-2.31145126867504,0.927232679798168,
10.5887878328943));
#92910=CARTESIAN_POINT('Ctrl Pts',(-2.36916488281964,0.173362644194442,
10.6397478783738));
#92911=CARTESIAN_POINT('Origin',(0.,0.,-1.84858989190503));
#92912=CARTESIAN_POINT('',(-2.36542649454111,0.173076750093535,11.8369288124872));
#92913=CARTESIAN_POINT('',(-2.36542649946083,0.173076682856166,11.6396027579113));
#92914=CARTESIAN_POINT('',(-2.36542649454111,0.173076750093529,-1.84858989190503));
#92915=CARTESIAN_POINT('',(-2.37174919443444,0.00195478888988407,10.848589891905));
#92916=CARTESIAN_POINT('Ctrl Pts',(-2.37174919443444,0.00195478888988407,
10.848589891905));
#92917=CARTESIAN_POINT('Ctrl Pts',(-2.37181439280241,-0.0771505188548095,
10.8538849196891));
#92918=CARTESIAN_POINT('Ctrl Pts',(-2.36791767540096,-0.156314771560316,
10.8591799474733));
#92919=CARTESIAN_POINT('Ctrl Pts',(-2.36006804502609,-0.23511036843734,
10.8644749752574));
#92920=CARTESIAN_POINT('Ctrl Pts',(-2.35222055250515,-0.313884505262257,
10.869768560936));
#92921=CARTESIAN_POINT('Ctrl Pts',(-2.34042233132756,-0.392289716004928,
10.8750621466145));
#92922=CARTESIAN_POINT('Ctrl Pts',(-2.32473434191077,-0.469902438853748,
10.880355732293));
#92923=CARTESIAN_POINT('Ctrl Pts',(-2.30904565535801,-0.547518610622591,
10.8856495532056));
#92924=CARTESIAN_POINT('Ctrl Pts',(-2.28946695249902,-0.624341762057178,
10.8909433741181));
#92925=CARTESIAN_POINT('Ctrl Pts',(-2.26611021311493,-0.699958973452166,
10.8962371950307));
#92926=CARTESIAN_POINT('Ctrl Pts',(-2.24272845082305,-0.775657196262196,
10.9015366874024));
#92927=CARTESIAN_POINT('Ctrl Pts',(-2.21556070906728,-0.850146446906356,
10.906836179774));
#92928=CARTESIAN_POINT('Ctrl Pts',(-2.18476855053317,-0.923030033694034,
10.9121356721457));
#92929=CARTESIAN_POINT('Ctrl Pts',(-2.15395976457295,-0.995952976814975,
10.9174380261848));
#92930=CARTESIAN_POINT('Ctrl Pts',(-2.11952287114002,-1.06726810453033,
10.9227403802239));
#92931=CARTESIAN_POINT('Ctrl Pts',(-2.08166607241455,-1.1366021403544,10.9280427342631));
#92932=CARTESIAN_POINT('Ctrl Pts',(-2.04373945114354,-1.20606405489607,
10.9333548678892));
#92933=CARTESIAN_POINT('Ctrl Pts',(-2.0023805726807,-1.27353717604168,10.9386670015153));
#92934=CARTESIAN_POINT('Ctrl Pts',(-1.95784158605713,-1.33867635610901,
10.9439791351414));
#92935=CARTESIAN_POINT('Ctrl Pts',(-1.92069211758932,-1.39300821454088,
10.9484099261315));
#92936=CARTESIAN_POINT('Ctrl Pts',(-1.8813310926315,-1.44571678485983,10.9528407171216));
#92937=CARTESIAN_POINT('Ctrl Pts',(-1.83992524872408,-1.49662057369516,
10.9572715081117));
#92938=CARTESIAN_POINT('Ctrl Pts',(-1.79010081493234,-1.5578740639572,10.9626031625715));
#92939=CARTESIAN_POINT('Ctrl Pts',(-1.73711971794155,-1.61675294397844,
10.9679348170314));
#92940=CARTESIAN_POINT('Ctrl Pts',(-1.68123688280041,-1.67291380722725,
10.9732664714912));
#92941=CARTESIAN_POINT('Ctrl Pts',(-1.62543493638254,-1.72899337931546,
10.9785904085415));
#92942=CARTESIAN_POINT('Ctrl Pts',(-1.56673992068801,-1.78236241789962,
10.9839143455918));
#92943=CARTESIAN_POINT('Ctrl Pts',(-1.50544717353461,-1.8327102526577,10.9892382826422));
#92944=CARTESIAN_POINT('Ctrl Pts',(-1.44422591298779,-1.88299936601688,
10.9945560103087));
#92945=CARTESIAN_POINT('Ctrl Pts',(-1.38041330222577,-1.93027398176313,
10.9998737379752));
#92946=CARTESIAN_POINT('Ctrl Pts',(-1.31434060260554,-1.97426108781045,
11.0051914656416));
#92947=CARTESIAN_POINT('Ctrl Pts',(-1.24831011197238,-2.01822009373169,
11.0105057962031));
#92948=CARTESIAN_POINT('Ctrl Pts',(-1.18002278741972,-2.05889549922399,
11.0158201267646));
#92949=CARTESIAN_POINT('Ctrl Pts',(-1.10984098717517,-2.09605606930875,
11.0211344573261));
#92950=CARTESIAN_POINT('Ctrl Pts',(-1.03968214854198,-2.13320448144707,
11.0264470491805));
#92951=CARTESIAN_POINT('Ctrl Pts',(-0.967630479063115,-2.16684012240153,
11.031759641035));
#92952=CARTESIAN_POINT('Ctrl Pts',(-0.894073896701073,-2.19677716888577,
11.0370722328894));
#92953=CARTESIAN_POINT('Ctrl Pts',(-0.820518456434641,-2.22671375054458,
11.0423847422564));
#92954=CARTESIAN_POINT('Ctrl Pts',(-0.745458584526182,-2.25295167635402,
11.0476972516235));
#92955=CARTESIAN_POINT('Ctrl Pts',(-0.669301793910461,-2.2753534167615,
11.0530097609906));
#92956=CARTESIAN_POINT('Ctrl Pts',(-0.593068959586898,-2.29777752564577,
11.0583275749786));
#92957=CARTESIAN_POINT('Ctrl Pts',(-0.515737469459638,-2.31635766453079,
11.0636453889667));
#92958=CARTESIAN_POINT('Ctrl Pts',(-0.437729032617402,-2.33100651146749,
11.0689632029547));
#92959=CARTESIAN_POINT('Ctrl Pts',(-0.359683267706368,-2.3456623680712,
11.0742835615871));
#92960=CARTESIAN_POINT('Ctrl Pts',(-0.280960376007474,-2.35638312176981,
11.0796039202195));
#92961=CARTESIAN_POINT('Ctrl Pts',(-0.201988715865797,-2.36313322120504,
11.0849242788519));
#92962=CARTESIAN_POINT('Ctrl Pts',(-0.122872789652276,-2.36989565177687,
11.0902543567587));
#92963=CARTESIAN_POINT('Ctrl Pts',(-0.0435076567296367,-2.37267291702921,
11.0955844346656));
#92964=CARTESIAN_POINT('Ctrl Pts',(0.035676974233163,-2.37148164994157,
11.1009145125724));
#92965=CARTESIAN_POINT('Ctrl Pts',(0.111551785538755,-2.37034017634511,
11.1060217998138));
#92966=CARTESIAN_POINT('Ctrl Pts',(0.187260521157683,-2.36555539903782,
11.1111290870551));
#92967=CARTESIAN_POINT('Ctrl Pts',(0.262431960950489,-2.35718635843068,
11.1162363742965));
#92968=CARTESIAN_POINT('Ctrl Pts',(0.340905742291385,-2.34844965916766,
11.1215680287563));
#92969=CARTESIAN_POINT('Ctrl Pts',(0.419091615225448,-2.33577336537002,
11.1268996832161));
#92970=CARTESIAN_POINT('Ctrl Pts',(0.496562842236019,-2.31918593610139,
11.1322313376759));
#92971=CARTESIAN_POINT('Ctrl Pts',(0.573921931975342,-2.30262251663778,
11.1375552747263));
#92972=CARTESIAN_POINT('Ctrl Pts',(0.650567975390163,-2.28215930145448,
11.1428792117766));
#92973=CARTESIAN_POINT('Ctrl Pts',(0.726079884680871,-2.25787645002153,
11.1482031488269));
#92974=CARTESIAN_POINT('Ctrl Pts',(0.801503723353056,-2.23362192002509,
11.1535208764934));
#92975=CARTESIAN_POINT('Ctrl Pts',(0.87579561244242,-2.20555674940822,11.1588386041599));
#92976=CARTESIAN_POINT('Ctrl Pts',(0.948546682480867,-2.17381168771689,
11.1641563318264));
#92977=CARTESIAN_POINT('Ctrl Pts',(1.02125127721261,-2.14208690561014,11.1694706623879));
#92978=CARTESIAN_POINT('Ctrl Pts',(1.09241657798509,-2.10668708537788,11.1747849929494));
#92979=CARTESIAN_POINT('Ctrl Pts',(1.161652009621,-2.06779173783132,11.1800993235109));
#92980=CARTESIAN_POINT('Ctrl Pts',(1.23086478927222,-2.02890911580401,11.1854119153653));
#92981=CARTESIAN_POINT('Ctrl Pts',(1.29814854507141,-1.98653346686885,11.1907245072197));
#92982=CARTESIAN_POINT('Ctrl Pts',(1.363137049472,-1.94089037476535,11.1960370990742));
#92983=CARTESIAN_POINT('Ctrl Pts',(1.42812454481162,-1.89524799135122,11.2013496084412));
#92984=CARTESIAN_POINT('Ctrl Pts',(1.49081647664435,-1.84633853618342,11.2066621178083));
#92985=CARTESIAN_POINT('Ctrl Pts',(1.55087661711426,-1.79443021067642,11.2119746271754));
#92986=CARTESIAN_POINT('Ctrl Pts',(1.61099672854311,-1.74247005392106,11.2172924411634));
#92987=CARTESIAN_POINT('Ctrl Pts',(1.66847944342655,-1.68750535237616,11.2226102551515));
#92988=CARTESIAN_POINT('Ctrl Pts',(1.7230230652465,-1.62984342166006,11.2279280691395));
#92989=CARTESIAN_POINT('Ctrl Pts',(1.77759278691089,-1.57215389894746,11.2332484277719));
#92990=CARTESIAN_POINT('Ctrl Pts',(1.82922030863834,-1.51176493275674,11.2385687864043));
#92991=CARTESIAN_POINT('Ctrl Pts',(1.87764386463513,-1.44901745334487,11.2438891450367));
#92992=CARTESIAN_POINT('Ctrl Pts',(1.92615588117835,-1.38615534632663,11.2492192229435));
#92993=CARTESIAN_POINT('Ctrl Pts',(1.97145196796719,-1.3209265026474,11.2545493008504));
#92994=CARTESIAN_POINT('Ctrl Pts',(2.0133135061698,-1.25370123569145,11.2598793787572));
#92995=CARTESIAN_POINT('Ctrl Pts',(2.05342528383996,-1.189285901766,11.2649866659986));
#92996=CARTESIAN_POINT('Ctrl Pts',(2.09038378236208,-1.12303806308547,11.2700939532399));
#92997=CARTESIAN_POINT('Ctrl Pts',(2.12403770038088,-1.05530180984433,11.2752012404812));
#92998=CARTESIAN_POINT('Ctrl Pts',(2.15917006196871,-0.984589848754286,
11.280532894941));
#92999=CARTESIAN_POINT('Ctrl Pts',(2.190834066755,-0.911987438658024,11.2858645494009));
#93000=CARTESIAN_POINT('Ctrl Pts',(2.21882264788155,-0.83786879626103,11.2911962038607));
#93001=CARTESIAN_POINT('Ctrl Pts',(2.24677071637878,-0.763857438369515,
11.296520140911));
#93002=CARTESIAN_POINT('Ctrl Pts',(2.27105376183779,-0.688334641479644,
11.3018440779614));
#93003=CARTESIAN_POINT('Ctrl Pts',(2.29151124663089,-0.611697857658614,
11.3071680150117));
#93004=CARTESIAN_POINT('Ctrl Pts',(2.31194487156715,-0.535150456413677,
11.3124857426782));
#93005=CARTESIAN_POINT('Ctrl Pts',(2.32856168209565,-0.457492100816392,
11.3178034703447));
#93006=CARTESIAN_POINT('Ctrl Pts',(2.3412502918617,-0.379137354210184,11.3231211980112));
#93007=CARTESIAN_POINT('Ctrl Pts',(2.35393079580842,-0.300832662687369,
11.3284355285727));
#93008=CARTESIAN_POINT('Ctrl Pts',(2.36268800501659,-0.221832924754916,
11.3337498591342));
#93009=CARTESIAN_POINT('Ctrl Pts',(2.36746143565309,-0.142563716265519,
11.3390641896957));
#93010=CARTESIAN_POINT('Ctrl Pts',(2.37223330455052,-0.0633204425448197,
11.3443767815501));
#93011=CARTESIAN_POINT('Ctrl Pts',(2.37302395483914,0.0161916589820648,
11.3496893734045));
#93012=CARTESIAN_POINT('Ctrl Pts',(2.36982482150072,0.0955425449686583,
11.3550019652589));
#93013=CARTESIAN_POINT('Ctrl Pts',(2.36662573783448,0.174892198893011,11.360314474626));
#93014=CARTESIAN_POINT('Ctrl Pts',(2.35943701388961,0.254080173799275,11.365626983993));
#93015=CARTESIAN_POINT('Ctrl Pts',(2.34830215769798,0.332678581593434,11.3709394933601));
#93016=CARTESIAN_POINT('Ctrl Pts',(2.33715618318396,0.411355471087036,11.3762573073482));
#93017=CARTESIAN_POINT('Ctrl Pts',(2.32205627107895,0.489441152109287,11.3815751213362));
#93018=CARTESIAN_POINT('Ctrl Pts',(2.30309750967023,0.566515598594419,11.3868929353243));
#93019=CARTESIAN_POINT('Ctrl Pts',(2.28412967624341,0.643626926221623,11.3922132939566));
#93020=CARTESIAN_POINT('Ctrl Pts',(2.26129944989605,0.719725605594071,11.397533652589));
#93021=CARTESIAN_POINT('Ctrl Pts',(2.23475179772338,0.7944069895665,11.4028540112214));
#93022=CARTESIAN_POINT('Ctrl Pts',(2.20815564808352,0.869224802099382,11.4081840891283));
#93023=CARTESIAN_POINT('Ctrl Pts',(2.17782868193531,0.942619710985243,11.4135141670351));
#93024=CARTESIAN_POINT('Ctrl Pts',(2.14396392819246,1.01420744283878,11.418844244942));
#93025=CARTESIAN_POINT('Ctrl Pts',(2.11151467928016,1.08280289602355,11.4239515321833));
#93026=CARTESIAN_POINT('Ctrl Pts',(2.07581772266374,1.14973894035833,11.4290588194247));
#93027=CARTESIAN_POINT('Ctrl Pts',(2.03708047755367,1.2147020994753,11.434166106666));
#93028=CARTESIAN_POINT('Ctrl Pts',(1.99664147424469,1.28251914219552,11.4394977611258));
#93029=CARTESIAN_POINT('Ctrl Pts',(1.95273548854899,1.34844321648543,11.4448294155856));
#93030=CARTESIAN_POINT('Ctrl Pts',(1.90556508455358,1.41209764925458,11.4501610700454));
#93031=CARTESIAN_POINT('Ctrl Pts',(1.85846295829933,1.47565994414665,11.4554850070958));
#93032=CARTESIAN_POINT('Ctrl Pts',(1.80810607400236,1.53695874797413,11.4608089441461));
#93033=CARTESIAN_POINT('Ctrl Pts',(1.75474171921775,1.59564393313068,11.4661328811964));
#93034=CARTESIAN_POINT('Ctrl Pts',(1.70143960404243,1.65426067291746,11.4714506088629));
#93035=CARTESIAN_POINT('Ctrl Pts',(1.64513730265756,1.71026950655098,11.4767683365294));
#93036=CARTESIAN_POINT('Ctrl Pts',(1.5861230961311,1.76335237159777,11.4820860641959));
#93037=CARTESIAN_POINT('Ctrl Pts',(1.52714658943978,1.81640132590716,11.4874003947574));
#93038=CARTESIAN_POINT('Ctrl Pts',(1.46546196384419,1.86652770889706,11.4927147253189));
#93039=CARTESIAN_POINT('Ctrl Pts',(1.40139431389172,1.9134502971052,11.4980290558804));
#93040=CARTESIAN_POINT('Ctrl Pts',(1.33734762516381,1.96035753349522,11.5033416477348));
#93041=CARTESIAN_POINT('Ctrl Pts',(1.2709198382455,2.00406277965911,11.5086542395892));
#93042=CARTESIAN_POINT('Ctrl Pts',(1.20246790807677,2.04432604849263,11.5139668314436));
#93043=CARTESIAN_POINT('Ctrl Pts',(1.1340170407448,2.08458869216798,11.5192793408107));
#93044=CARTESIAN_POINT('Ctrl Pts',(1.06354249746166,2.12140922816019,11.5245918501778));
#93045=CARTESIAN_POINT('Ctrl Pts',(0.991427608477204,2.15459262034594,11.5299043595448));
#93046=CARTESIAN_POINT('Ctrl Pts',(0.919240711684985,2.18780914665085,11.5352221735329));
#93047=CARTESIAN_POINT('Ctrl Pts',(0.845410624200989,2.21738107774086,11.5405399875209));
#93048=CARTESIAN_POINT('Ctrl Pts',(0.770341986431395,2.24316100323649,11.545857801509));
#93049=CARTESIAN_POINT('Ctrl Pts',(0.695237427325773,2.26895326476743,11.5511781601414));
#93050=CARTESIAN_POINT('Ctrl Pts',(0.618893588439674,2.29094977588689,11.5564985187737));
#93051=CARTESIAN_POINT('Ctrl Pts',(0.541729178938679,2.30905339028495,11.5618188774061));
#93052=CARTESIAN_POINT('Ctrl Pts',(0.464423804866006,2.32719007651323,11.567148955313));
#93053=CARTESIAN_POINT('Ctrl Pts',(0.386295327264472,2.3414195710149,11.5724790332198));
#93054=CARTESIAN_POINT('Ctrl Pts',(0.307771340723714,2.35169616752019,11.5778091111267));
#93055=CARTESIAN_POINT('Ctrl Pts',(0.232529559720264,2.36154321499924,11.582916398368));
#93056=CARTESIAN_POINT('Ctrl Pts',(0.156925044820003,2.3677612588708,11.5880236856094));
#93057=CARTESIAN_POINT('Ctrl Pts',(0.0813336522693424,2.37035501550053,
11.5931309728507));
#93058=CARTESIAN_POINT('Ctrl Pts',(0.00242146930970082,2.37306271793611,
11.5984626273105));
#93059=CARTESIAN_POINT('Ctrl Pts',(-0.0767757596815532,2.37183061769798,
11.6037942817703));
#93060=CARTESIAN_POINT('Ctrl Pts',(-0.155831669178614,2.36662514002134,
11.6091259362302));
#93061=CARTESIAN_POINT('Ctrl Pts',(-0.234773147624385,2.36142719711707,
11.6144498732805));
#93062=CARTESIAN_POINT('Ctrl Pts',(-0.313573248870372,2.35226732864514,
11.6197738103308));
#93063=CARTESIAN_POINT('Ctrl Pts',(-0.391803718379393,2.33916393370881,
11.6250977473812));
#93064=CARTESIAN_POINT('Ctrl Pts',(-0.469942946574139,2.32607582144921,
11.6304154750477));
#93065=CARTESIAN_POINT('Ctrl Pts',(-0.547513403230365,2.30905339975424,
11.6357332027142));
#93066=CARTESIAN_POINT('Ctrl Pts',(-0.624091604942801,2.28816689320074,
11.6410509303807));
#93067=CARTESIAN_POINT('Ctrl Pts',(-0.700620886475727,2.26729372949973,
11.6463652609422));
#93068=CARTESIAN_POINT('Ctrl Pts',(-0.776158720056143,2.24256150346772,
11.6516795915036));
#93069=CARTESIAN_POINT('Ctrl Pts',(-0.850292670021049,2.21409133456786,
11.6569939220651));
#93070=CARTESIAN_POINT('Ctrl Pts',(-0.924402365336662,2.1856304803472,11.6623065139195));
#93071=CARTESIAN_POINT('Ctrl Pts',(-0.99710865170529,2.15343427964622,11.667619105774));
#93072=CARTESIAN_POINT('Ctrl Pts',(-1.06801651977944,2.11767296247041,11.6729316976284));
#93073=CARTESIAN_POINT('Ctrl Pts',(-1.13892328688408,2.08191220055203,11.6782442069954));
#93074=CARTESIAN_POINT('Ctrl Pts',(-1.20803127313806,2.0425866445149,11.6835567163625));
#93075=CARTESIAN_POINT('Ctrl Pts',(-1.27496898797061,1.99991303366252,11.6888692257296));
#93076=CARTESIAN_POINT('Ctrl Pts',(-1.34197354112422,1.95719681256403,11.6941870397176));
#93077=CARTESIAN_POINT('Ctrl Pts',(-1.40680309753799,1.91112611101221,11.6995048537057));
#93078=CARTESIAN_POINT('Ctrl Pts',(-1.46911467622812,1.86196136656783,11.7048226676937));
#93079=CARTESIAN_POINT('Ctrl Pts',(-1.53145607183287,1.81277309614292,11.7101430263261));
#93080=CARTESIAN_POINT('Ctrl Pts',(-1.59127673585833,1.76048814235256,11.7154633849585));
#93081=CARTESIAN_POINT('Ctrl Pts',(-1.6482683350962,1.7054059804103,11.7207837435909));
#93082=CARTESIAN_POINT('Ctrl Pts',(-1.70536404705162,1.65022319392607,11.7261138214977));
#93083=CARTESIAN_POINT('Ctrl Pts',(-1.75962004570391,1.59223333156763,11.7314438994046));
#93084=CARTESIAN_POINT('Ctrl Pts',(-1.81076644018087,1.53177118448374,11.7367739773114));
#93085=CARTESIAN_POINT('Ctrl Pts',(-1.85977497861462,1.47383628038247,11.7418812645528));
#93086=CARTESIAN_POINT('Ctrl Pts',(-1.90592851005167,1.41363197589522,11.7469885517941));
#93087=CARTESIAN_POINT('Ctrl Pts',(-1.94902754655883,1.35147685339219,11.7520958390355));
#93088=CARTESIAN_POINT('Ctrl Pts',(-1.99459973994361,1.28575507647748,11.7574961983172));
#93089=CARTESIAN_POINT('Ctrl Pts',(-2.03692704740659,1.21760624616623,11.7628965575989));
#93090=CARTESIAN_POINT('Ctrl Pts',(-2.07574541907485,1.1473791952488,11.7682969168806));
#93091=CARTESIAN_POINT('Ctrl Pts',(-2.11450324092046,1.07726168616158,11.773688852553));
#93092=CARTESIAN_POINT('Ctrl Pts',(-2.14976278316903,1.00507278974043,11.7790807882254));
#93093=CARTESIAN_POINT('Ctrl Pts',(-2.1813026563105,0.931191056697159,11.7844727238978));
#93094=CARTESIAN_POINT('Ctrl Pts',(-2.21279447910213,0.85742188095884,11.7898564450668));
#93095=CARTESIAN_POINT('Ctrl Pts',(-2.24057772870709,0.781965413353284,
11.7952401662358));
#93096=CARTESIAN_POINT('Ctrl Pts',(-2.26447718931189,0.705224164068507,
11.8006238874048));
#93097=CARTESIAN_POINT('Ctrl Pts',(-2.2883555098361,0.628550795654401,11.8060028464455));
#93098=CARTESIAN_POINT('Ctrl Pts',(-2.30835673213667,0.550595334368634,
11.8113818054861));
#93099=CARTESIAN_POINT('Ctrl Pts',(-2.32435427522725,0.471778831374215,
11.8167607645267));
#93100=CARTESIAN_POINT('Ctrl Pts',(-2.34034131720126,0.393014065154663,
11.8221361927079));
#93101=CARTESIAN_POINT('Ctrl Pts',(-2.3523298160296,0.313389824482069,11.8275116208891));
#93102=CARTESIAN_POINT('Ctrl Pts',(-2.36024378681681,0.233339515069065,
11.8328870490703));
#93103=CARTESIAN_POINT('Ctrl Pts',(-2.36222728137341,0.213276343591111,
11.8342343035426));
#93104=CARTESIAN_POINT('Ctrl Pts',(-2.36395508028738,0.193186454362623,
11.8355815580149));
#93105=CARTESIAN_POINT('Ctrl Pts',(-2.36542649454111,0.173076750093539,
11.8369288124873));
#93106=CARTESIAN_POINT('Ctrl Pts',(-2.36516017494062,0.173060140022867,
10.8371116396001));
#93107=CARTESIAN_POINT('Ctrl Pts',(-2.36874872137079,0.116159691458484,
10.8409373761948));
#93108=CARTESIAN_POINT('Ctrl Pts',(-2.3703080243951,0.0590785852099101,
10.8447631127894));
#93109=CARTESIAN_POINT('Ctrl Pts',(-2.36986628361774,0.00196879943266851,
10.8485888493841));
#93110=CARTESIAN_POINT('',(-2.37530980438986,0.000525500814253238,10.6515288999801));
#93111=CARTESIAN_POINT('Ctrl Pts',(-2.36916488281964,0.173362644194442,
10.6397478783738));
#93112=CARTESIAN_POINT('Ctrl Pts',(-2.37143439054323,0.143717752018713,
10.641751811389));
#93113=CARTESIAN_POINT('Ctrl Pts',(-2.37467009649357,0.0861306150212709,
10.645639221296));
#93114=CARTESIAN_POINT('Ctrl Pts',(-2.37559956836887,0.0284615660624313,
10.6495266312031));
#93115=CARTESIAN_POINT('Ctrl Pts',(-2.37551677123795,0.000517782250847756,
10.651410108095));
#93116=CARTESIAN_POINT('Ctrl Pts',(-2.37174990865192,0.000658262564380199,
10.6535721582573));
#93117=CARTESIAN_POINT('Ctrl Pts',(-2.37177855672722,-0.102562053547647,
10.6603515320337));
#93118=CARTESIAN_POINT('Ctrl Pts',(-2.36506879052359,-0.205690967288313,
10.6668060514094));
#93119=CARTESIAN_POINT('Ctrl Pts',(-2.34197585620198,-0.38197192072136,
10.6777762038329));
#93120=CARTESIAN_POINT('Ctrl Pts',(-2.32881606256741,-0.455378403733495,
10.6823250941134));
#93121=CARTESIAN_POINT('Ctrl Pts',(-2.27881465861748,-0.674326638542228,
10.6961102588934));
#93122=CARTESIAN_POINT('Ctrl Pts',(-2.23160731925022,-0.817087733319469,
10.7054176415574));
#93123=CARTESIAN_POINT('Ctrl Pts',(-2.16230900018982,-0.974735953336503,
10.716647787053));
#93124=CARTESIAN_POINT('Ctrl Pts',(-2.15309571846237,-0.994921687018294,
10.7181039410699));
#93125=CARTESIAN_POINT('Ctrl Pts',(-2.13871840384251,-1.02528621285605,
10.7203235351299));
#93126=CARTESIAN_POINT('Ctrl Pts',(-2.13376170475477,-1.03556226698929,
10.7210798203346));
#93127=CARTESIAN_POINT('Ctrl Pts',(-2.1246515962004,-1.05410590289595,10.7224540779902));
#93128=CARTESIAN_POINT('Ctrl Pts',(-2.12052355982764,-1.0623857528218,10.7230711561611));
#93129=CARTESIAN_POINT('Ctrl Pts',(-2.11154677544505,-1.08013025387168,
10.7244011880773));
#93130=CARTESIAN_POINT('Ctrl Pts',(-2.10668262037068,-1.08958683951847,
10.7251146729013));
#93131=CARTESIAN_POINT('Ctrl Pts',(-2.09339287495878,-1.11500224390189,
10.7270450469932));
#93132=CARTESIAN_POINT('Ctrl Pts',(-2.08484860798215,-1.13089786593802,
10.7282661091733));
#93133=CARTESIAN_POINT('Ctrl Pts',(-2.04193293605268,-1.20859797680012,
10.7343041385278));
#93134=CARTESIAN_POINT('Ctrl Pts',(-2.0049938152364,-1.26893544663137,10.7392122268613));
#93135=CARTESIAN_POINT('Ctrl Pts',(-1.85958502749163,-1.48421459737501,
10.757562006479));
#93136=CARTESIAN_POINT('Ctrl Pts',(-1.73540061895271,-1.62767234238671,
10.7715377553805));
#93137=CARTESIAN_POINT('Ctrl Pts',(-1.55431056427747,-1.79232279465742,
10.7892498975896));
#93138=CARTESIAN_POINT('Ctrl Pts',(-1.5117757750581,-1.82834274679318,10.7932450418659));
#93139=CARTESIAN_POINT('Ctrl Pts',(-1.45150583049823,-1.87583857981293,
10.798644656267));
#93140=CARTESIAN_POINT('Ctrl Pts',(-1.43482995696554,-1.88862453060262,
10.8001123835859));
#93141=CARTESIAN_POINT('Ctrl Pts',(-1.40942806208962,-1.90757033221001,
10.8023062709012));
#93142=CARTESIAN_POINT('Ctrl Pts',(-1.40082720587638,-1.91389529079522,
10.8030420073151));
#93143=CARTESIAN_POINT('Ctrl Pts',(-1.38676238195868,-1.92409277318672,
10.8042332712554));
#93144=CARTESIAN_POINT('Ctrl Pts',(-1.38132431680734,-1.92800052861667,
10.8046910087846));
#93145=CARTESIAN_POINT('Ctrl Pts',(-1.37085666863622,-1.93545548475865,
10.8055665222849));
#93146=CARTESIAN_POINT('Ctrl Pts',(-1.36582969442947,-1.93900623707863,
10.8059845302999));
#93147=CARTESIAN_POINT('Ctrl Pts',(-1.36076363840581,-1.94255511732426,
10.806403288096));
#93148=CARTESIAN_POINT('Ctrl Pts',(-1.36073839288779,-1.9425728016142,10.8064053748164));
#93149=CARTESIAN_POINT('Ctrl Pts',(-1.36068774231298,-1.94260828047789,
10.8064095613193));
#93150=CARTESIAN_POINT('Ctrl Pts',(-1.36066233724572,-1.94262607504972,
10.8064116611019));
#93151=CARTESIAN_POINT('Ctrl Pts',(-1.36061136416369,-1.94266177683688,
10.8064158740086));
#93152=CARTESIAN_POINT('Ctrl Pts',(-1.36058579616253,-1.94267968403316,
10.8064179871308));
#93153=CARTESIAN_POINT('Ctrl Pts',(-1.36053449373456,-1.94271561347654,
10.8064222270018));
#93154=CARTESIAN_POINT('Ctrl Pts',(-1.36050875931149,-1.94273363571123,
10.8064243537494));
#93155=CARTESIAN_POINT('Ctrl Pts',(-1.36045712051414,-1.94276979767096,
10.8064286211599));
#93156=CARTESIAN_POINT('Ctrl Pts',(-1.36043121610644,-1.94278793740934,
10.8064307618248));
#93157=CARTESIAN_POINT('Ctrl Pts',(-1.36037923366798,-1.94282433691737,
10.8064350573708));
#93158=CARTESIAN_POINT('Ctrl Pts',(-1.36035315568065,-1.94284259664626,
10.8064372122475));
#93159=CARTESIAN_POINT('Ctrl Pts',(-1.36030082241604,-1.94287923867169,
10.8064415365173));
#93160=CARTESIAN_POINT('Ctrl Pts',(-1.36027456707164,-1.94289762100459,
10.8064437059152));
#93161=CARTESIAN_POINT('Ctrl Pts',(-1.36022187528905,-1.9429345108692,10.8064480595391));
#93162=CARTESIAN_POINT('Ctrl Pts',(-1.36019543884565,-1.94295301839363,
10.8064502437646));
#93163=CARTESIAN_POINT('Ctrl Pts',(-1.36014238094027,-1.94299016135598,
10.8064546273652));
#93164=CARTESIAN_POINT('Ctrl Pts',(-1.36011575949941,-1.94300879676787,
10.8064568267376));
#93165=CARTESIAN_POINT('Ctrl Pts',(-1.36006232760328,-1.94304619826841,
10.8064612409593));
#93166=CARTESIAN_POINT('Ctrl Pts',(-1.36003551718488,-1.94306496431968,
10.8064634558045));
#93167=CARTESIAN_POINT('Ctrl Pts',(-1.35998541134579,-1.94310003454148,
10.806467594985));
#93168=CARTESIAN_POINT('Ctrl Pts',(-1.35996211603031,-1.94311633884101,
10.8064695193288));
#93169=CARTESIAN_POINT('Ctrl Pts',(-1.35991474648953,-1.94314949132684,
10.8064734322516));
#93170=CARTESIAN_POINT('Ctrl Pts',(-1.35989067217942,-1.94316633953011,
10.8064754208341));
#93171=CARTESIAN_POINT('Ctrl Pts',(-1.35984171027439,-1.94320060375164,
10.8064794650627));
#93172=CARTESIAN_POINT('Ctrl Pts',(-1.35981682265666,-1.94321801974011,
10.8064815207069));
#93173=CARTESIAN_POINT('Ctrl Pts',(-1.35976619771028,-1.94325344488342,
10.8064857020559));
#93174=CARTESIAN_POINT('Ctrl Pts',(-1.35974046038036,-1.94327145398973,
10.8064878277565));
#93175=CARTESIAN_POINT('Ctrl Pts',(-1.3596880974565,-1.94330809219513,10.8064921523899));
#93176=CARTESIAN_POINT('Ctrl Pts',(-1.35966147181243,-1.94332672127587,
10.8064943513222));
#93177=CARTESIAN_POINT('Ctrl Pts',(-1.35960729133036,-1.94336462790497,
10.8064988257853));
#93178=CARTESIAN_POINT('Ctrl Pts',(-1.35957973645772,-1.94338390541973,
10.806501101314));
#93179=CARTESIAN_POINT('Ctrl Pts',(-1.35952365400987,-1.94342313917986,
10.806505732548));
#93180=CARTESIAN_POINT('Ctrl Pts',(-1.35949512643571,-1.94344309536184,
10.8065080882479));
#93181=CARTESIAN_POINT('Ctrl Pts',(-1.35943705237479,-1.94348371859161,
10.8065128836238));
#93182=CARTESIAN_POINT('Ctrl Pts',(-1.35940750584423,-1.94350438560208,
10.8065153232977));
#93183=CARTESIAN_POINT('Ctrl Pts',(-1.35934734466194,-1.94354646470216,
10.8065202906673));
#93184=CARTESIAN_POINT('Ctrl Pts',(-1.35931672999974,-1.94356787672531,
10.8065228183576));
#93185=CARTESIAN_POINT('Ctrl Pts',(-1.35925438013928,-1.94361148228545,
10.8065279660684));
#93186=CARTESIAN_POINT('Ctrl Pts',(-1.35922264490275,-1.94363367576899,
10.8065305860854));
#93187=CARTESIAN_POINT('Ctrl Pts',(-1.35915799801078,-1.94367888308644,
10.8065359230424));
#93188=CARTESIAN_POINT('Ctrl Pts',(-1.35912508628047,-1.9437018968854,10.8065386399813));
#93189=CARTESIAN_POINT('Ctrl Pts',(-1.35905802666991,-1.94374878633537,
10.8065441756904));
#93190=CARTESIAN_POINT('Ctrl Pts',(-1.35902387876052,-1.94377266191158,
10.8065469944551));
#93191=CARTESIAN_POINT('Ctrl Pts',(-1.3589542829551,-1.94382131925974,10.8065527390607));
#93192=CARTESIAN_POINT('Ctrl Pts',(-1.35891883499726,-1.94384610097105,
10.8065556648979));
#93193=CARTESIAN_POINT('Ctrl Pts',(-1.35884657077098,-1.94389661803854,
10.806561629261));
#93194=CARTESIAN_POINT('Ctrl Pts',(-1.35880975442627,-1.94392235333456,
10.8065646677836));
#93195=CARTESIAN_POINT('Ctrl Pts',(-1.35873468015481,-1.94397482844385,
10.8065708635353));
#93196=CARTESIAN_POINT('Ctrl Pts',(-1.35869642217958,-1.94400156816683,
10.8065740207579));
#93197=CARTESIAN_POINT('Ctrl Pts',(-1.35861838601825,-1.94405610670789,
10.8065804603662));
#93198=CARTESIAN_POINT('Ctrl Pts',(-1.35857860776842,-1.94408390543441,
10.8065837427457));
#93199=CARTESIAN_POINT('Ctrl Pts',(-1.35849744653652,-1.94414062063485,
10.8065904396068));
#93200=CARTESIAN_POINT('Ctrl Pts',(-1.35845606350983,-1.94416953699056,
10.8065938540795));
#93201=CARTESIAN_POINT('Ctrl Pts',(-1.35427288750917,-1.94709232899285,
10.8069389868935));
#93202=CARTESIAN_POINT('Ctrl Pts',(-1.3501219320337,-1.94997291280233,10.8072797771417));
#93203=CARTESIAN_POINT('Ctrl Pts',(-1.34042327662125,-1.9566575447366,10.8080721621889));
#93204=CARTESIAN_POINT('Ctrl Pts',(-1.33486856848885,-1.9604512785472,10.8085230579424));
#93205=CARTESIAN_POINT('Ctrl Pts',(-1.32000824304342,-1.97050808614307,
10.8097217575619));
#93206=CARTESIAN_POINT('Ctrl Pts',(-1.31067407003795,-1.97672895805159,
10.8104668286348));
#93207=CARTESIAN_POINT('Ctrl Pts',(-1.23701135038108,-2.02507117940273,
10.8162882146222));
#93208=CARTESIAN_POINT('Ctrl Pts',(-1.17070558587072,-2.06411276854797,
10.8211803458188));
#93209=CARTESIAN_POINT('Ctrl Pts',(-0.976450919664753,-2.16611333880979,
10.8348906635437));
#93210=CARTESIAN_POINT('Ctrl Pts',(-0.844572163153181,-2.22085670258079,
10.8434847809167));
#93211=CARTESIAN_POINT('Ctrl Pts',(-0.59548473626215,-2.29883408201945,
10.8596255141512));
#93212=CARTESIAN_POINT('Ctrl Pts',(-0.479918009171846,-2.32570702472925,
10.8670794224785));
#93213=CARTESIAN_POINT('Ctrl Pts',(-0.343099502869632,-2.34688723851706,
10.8761275621036));
#93214=CARTESIAN_POINT('Ctrl Pts',(-0.323324416631526,-2.34969322689631,
10.8774403677106));
#93215=CARTESIAN_POINT('Ctrl Pts',(-0.292659917557485,-2.35364994597511,
10.8794848910023));
#93216=CARTESIAN_POINT('Ctrl Pts',(-0.281793686033334,-2.35497562773259,
10.8802110890818));
#93217=CARTESIAN_POINT('Ctrl Pts',(-0.26264991655199,-2.35717677795537,
10.8814936418762));
#93218=CARTESIAN_POINT('Ctrl Pts',(-0.254376158224509,-2.3580839909304,
10.8820489862936));
#93219=CARTESIAN_POINT('Ctrl Pts',(-0.235477565867177,-2.36005559198576,
10.8833199321225));
#93220=CARTESIAN_POINT('Ctrl Pts',(-0.224850038448066,-2.36109180995202,
10.8840364077769));
#93221=CARTESIAN_POINT('Ctrl Pts',(-0.196053529897931,-2.36370337929788,
10.8859827443179));
#93222=CARTESIAN_POINT('Ctrl Pts',(-0.177873098454385,-2.36514096414576,
10.887216895677));
#93223=CARTESIAN_POINT('Ctrl Pts',(-0.086739341266469,-2.3712905071774,
10.8934314899476));
#93224=CARTESIAN_POINT('Ctrl Pts',(-0.0136194423552338,-2.37283688671384,
10.8985096179776));
#93225=CARTESIAN_POINT('Ctrl Pts',(0.2195631141867,-2.36699024645351,10.9150063657144));
#93226=CARTESIAN_POINT('Ctrl Pts',(0.378844997908836,-2.34676716671444,
10.9267627423823));
#93227=CARTESIAN_POINT('Ctrl Pts',(0.630116044658595,-2.28860518083762,
10.9455482804648));
#93228=CARTESIAN_POINT('Ctrl Pts',(0.723937916130801,-2.26068086315785,
10.9526083175941));
#93229=CARTESIAN_POINT('Ctrl Pts',(0.833504231121622,-2.22054615047882,
10.9607207934211));
#93230=CARTESIAN_POINT('Ctrl Pts',(0.851154649697953,-2.21384062855498,
10.9620233016448));
#93231=CARTESIAN_POINT('Ctrl Pts',(0.875742191003425,-2.20416210104155,
10.9638297776904));
#93232=CARTESIAN_POINT('Ctrl Pts',(0.882747486997461,-2.20136590119113,
10.9643435533696));
#93233=CARTESIAN_POINT('Ctrl Pts',(0.894672872541858,-2.19653974207446,
10.9652164705167));
#93234=CARTESIAN_POINT('Ctrl Pts',(0.899599651557467,-2.1945265677448,10.9655766029113));
#93235=CARTESIAN_POINT('Ctrl Pts',(0.909088931904526,-2.19061174274308,
10.9662692245031));
#93236=CARTESIAN_POINT('Ctrl Pts',(0.913652292164789,-2.18871240315491,
10.9666018549363));
#93237=CARTESIAN_POINT('Ctrl Pts',(0.924629923519784,-2.18410303167298,
10.9674010272745));
#93238=CARTESIAN_POINT('Ctrl Pts',(0.931038311020611,-2.18137897095283,
10.9678667298372));
#93239=CARTESIAN_POINT('Ctrl Pts',(0.954601457577117,-2.17124005563474,
10.9695763584362));
#93240=CARTESIAN_POINT('Ctrl Pts',(0.971680963947044,-2.16365049862781,
10.9708102298911));
#93241=CARTESIAN_POINT('Ctrl Pts',(1.12509251781218,-2.09329649848442,10.9818604945114));
#93242=CARTESIAN_POINT('Ctrl Pts',(1.25528997691375,-2.01791570185769,10.9910179840959));
#93243=CARTESIAN_POINT('Ctrl Pts',(1.5207523723073,-1.82851758322732,11.0110010064882));
#93244=CARTESIAN_POINT('Ctrl Pts',(1.65216231956746,-1.71070528831344,11.0218081618593));
#93245=CARTESIAN_POINT('Ctrl Pts',(1.78347217173396,-1.56360997290639,11.0346784623678));
#93246=CARTESIAN_POINT('Ctrl Pts',(1.7974019591043,-1.54757723034504,11.0360731839114));
#93247=CARTESIAN_POINT('Ctrl Pts',(1.81835426685494,-1.52279728181172,11.0382178780451));
#93248=CARTESIAN_POINT('Ctrl Pts',(1.82553341708056,-1.51418345555346,11.0389614206063));
#93249=CARTESIAN_POINT('Ctrl Pts',(1.8379479943042,-1.49907133394873,11.0402626374283));
#93250=CARTESIAN_POINT('Ctrl Pts',(1.84321075281791,-1.49259566248446,11.040819191603));
#93251=CARTESIAN_POINT('Ctrl Pts',(1.85499633158649,-1.47793646289439,11.0420768589956));
#93252=CARTESIAN_POINT('Ctrl Pts',(1.86149934665385,-1.46973730811498,11.0427787505235));
#93253=CARTESIAN_POINT('Ctrl Pts',(1.87888411045545,-1.44751771776724,11.0446769001864));
#93254=CARTESIAN_POINT('Ctrl Pts',(1.8896629184369,-1.43341796715046,11.0458771922744));
#93255=CARTESIAN_POINT('Ctrl Pts',(1.93899187717406,-1.36736736419656,11.0514818078453));
#93256=CARTESIAN_POINT('Ctrl Pts',(1.97556114519041,-1.3139786028395,11.0559615453137));
#93257=CARTESIAN_POINT('Ctrl Pts',(2.12413037728108,-1.07683018355432,11.0756627160543));
#93258=CARTESIAN_POINT('Ctrl Pts',(2.21300974533638,-0.879804498679115,
11.0916583939711));
#93259=CARTESIAN_POINT('Ctrl Pts',(2.28632543187786,-0.632272086991002,
11.1102057817263));
#93260=CARTESIAN_POINT('Ctrl Pts',(2.29742756513531,-0.59065981831843,11.1132694871275));
#93261=CARTESIAN_POINT('Ctrl Pts',(2.31346054361505,-0.523246091727197,
11.1181233129115));
#93262=CARTESIAN_POINT('Ctrl Pts',(2.319106438672,-0.497625994748596,11.1199428559617));
#93263=CARTESIAN_POINT('Ctrl Pts',(2.32603031119974,-0.463523880779648,
11.1223269979846));
#93264=CARTESIAN_POINT('Ctrl Pts',(2.32768879956987,-0.455122241550293,
11.1229113453561));
#93265=CARTESIAN_POINT('Ctrl Pts',(2.33034395619426,-0.441277379507445,
11.1238690959426));
#93266=CARTESIAN_POINT('Ctrl Pts',(2.33136712796991,-0.435839415464244,
11.124243967043));
#93267=CARTESIAN_POINT('Ctrl Pts',(2.33333686830551,-0.42516518513809,11.1249771653168));
#93268=CARTESIAN_POINT('Ctrl Pts',(2.33428485943968,-0.419929245928414,
11.1253355673542));
#93269=CARTESIAN_POINT('Ctrl Pts',(2.33658141546411,-0.406996811739778,
11.1262178177399));
#93270=CARTESIAN_POINT('Ctrl Pts',(2.33790959851112,-0.399296668401241,
11.1267405206304));
#93271=CARTESIAN_POINT('Ctrl Pts',(2.34236875254388,-0.372659489656154,
11.1285401726563));
#93272=CARTESIAN_POINT('Ctrl Pts',(2.34530798860914,-0.353690493072396,
11.1298068562175));
#93273=CARTESIAN_POINT('Ctrl Pts',(2.36677574686537,-0.203082220411515,
11.1397611699796));
#93274=CARTESIAN_POINT('Ctrl Pts',(2.37443966949902,-0.0701137673008996,
11.1479364903347));
#93275=CARTESIAN_POINT('Ctrl Pts',(2.36744621573709,0.193863576813738,11.1641290464489));
#93276=CARTESIAN_POINT('Ctrl Pts',(2.35311514737728,0.324393138668978,11.1721235850249));
#93277=CARTESIAN_POINT('Ctrl Pts',(2.31505593657268,0.519959955708822,11.1847100432378));
#93278=CARTESIAN_POINT('Ctrl Pts',(2.2991617468733,0.586256108800425,11.1890835433532));
#93279=CARTESIAN_POINT('Ctrl Pts',(2.27567736287208,0.668423934099408,11.1946842220737));
#93280=CARTESIAN_POINT('Ctrl Pts',(2.27073580381394,0.685023283094217,11.1958249652052));
#93281=CARTESIAN_POINT('Ctrl Pts',(2.26254527836951,0.71147345789522,11.1976582764114));
#93282=CARTESIAN_POINT('Ctrl Pts',(2.25941265103047,0.721359885563684,11.198347032247));
#93283=CARTESIAN_POINT('Ctrl Pts',(2.25335188690899,0.740060535785525,11.1996566594698));
#93284=CARTESIAN_POINT('Ctrl Pts',(2.25043661090854,0.748878747803039,11.2002770971877));
#93285=CARTESIAN_POINT('Ctrl Pts',(2.24369713021494,0.768869757562372,11.2016903249018));
#93286=CARTESIAN_POINT('Ctrl Pts',(2.23984114709551,0.78003150143302,11.2024841530864));
#93287=CARTESIAN_POINT('Ctrl Pts',(2.22963599977951,0.808872190675591,11.2045479311926));
#93288=CARTESIAN_POINT('Ctrl Pts',(2.22315997791522,0.826505045049896,11.2058220598898));
#93289=CARTESIAN_POINT('Ctrl Pts',(2.17269392282489,0.959027545669819,11.2154937460931));
#93290=CARTESIAN_POINT('Ctrl Pts',(2.12004130056399,1.07039650467926,11.2241831913187));
#93291=CARTESIAN_POINT('Ctrl Pts',(2.0222061583261,1.24152155047438,11.2384173882982));
#93292=CARTESIAN_POINT('Ctrl Pts',(1.98241694261831,1.30411496245312,11.2438289013861));
#93293=CARTESIAN_POINT('Ctrl Pts',(1.86050162841416,1.47739843223089,11.2593049109378));
#93294=CARTESIAN_POINT('Ctrl Pts',(1.7715662487696,1.58295115751608,11.2693599836763));
#93295=CARTESIAN_POINT('Ctrl Pts',(1.66449802284079,1.68962208789066,11.2797958728282));
#93296=CARTESIAN_POINT('Ctrl Pts',(1.6549560191809,1.69896941212699,11.2807127519123));
#93297=CARTESIAN_POINT('Ctrl Pts',(1.6406107325798,1.71278647700723,11.282070992248));
#93298=CARTESIAN_POINT('Ctrl Pts',(1.63586725167142,1.71731750972871,11.2825168772102));
#93299=CARTESIAN_POINT('Ctrl Pts',(1.62733861081879,1.72539677278599,11.2833126902217));
#93300=CARTESIAN_POINT('Ctrl Pts',(1.62356056461951,1.72895230487403,11.2836631717741));
#93301=CARTESIAN_POINT('Ctrl Pts',(1.61528659344259,1.73668793039233,11.2844262602746));
#93302=CARTESIAN_POINT('Ctrl Pts',(1.61078610150729,1.74086297102386,11.2848384847793));
#93303=CARTESIAN_POINT('Ctrl Pts',(1.59817196586284,1.75247412362819,11.2859861380486));
#93304=CARTESIAN_POINT('Ctrl Pts',(1.59002256790987,1.75987142476776,11.2867187027113));
#93305=CARTESIAN_POINT('Ctrl Pts',(1.54449145517604,1.80062607637464,11.2907645736694));
#93306=CARTESIAN_POINT('Ctrl Pts',(1.50610847805551,1.83285194131579,11.2940009934202));
#93307=CARTESIAN_POINT('Ctrl Pts',(1.30102694656459,1.99423877474508,11.3105843018611));
#93308=CARTESIAN_POINT('Ctrl Pts',(1.11866633077756,2.10196591509147,11.3230613631996));
#93309=CARTESIAN_POINT('Ctrl Pts',(0.848706595088635,2.21622653481581,11.3414479702813));
#93310=CARTESIAN_POINT('Ctrl Pts',(0.771354097194692,2.24432027448511,11.3466963436107));
#93311=CARTESIAN_POINT('Ctrl Pts',(0.675197604079128,2.2736845301268,11.3532783993091));
#93312=CARTESIAN_POINT('Ctrl Pts',(0.657629539709259,2.27882787951193,11.3544831292475));
#93313=CARTESIAN_POINT('Ctrl Pts',(0.629809855633368,2.28662408200232,11.356395069229));
#93314=CARTESIAN_POINT('Ctrl Pts',(0.619596740980551,2.28941259257102,11.3570978640954));
#93315=CARTESIAN_POINT('Ctrl Pts',(0.600419709634012,2.29451082299095,11.3584193085699));
#93316=CARTESIAN_POINT('Ctrl Pts',(0.591460246160596,2.29683663275421,11.3590374234211));
#93317=CARTESIAN_POINT('Ctrl Pts',(0.57136509858727,2.3019278084078,11.3604255549814));
#93318=CARTESIAN_POINT('Ctrl Pts',(0.560222563250849,2.30466491763578,11.3611964673644));
#93319=CARTESIAN_POINT('Ctrl Pts',(0.531860436445721,2.31141410039507,11.3631620169667));
#93320=CARTESIAN_POINT('Ctrl Pts',(0.514615287644154,2.31531461004938,11.3643601978426));
#93321=CARTESIAN_POINT('Ctrl Pts',(0.408761535603934,2.33801560008784,11.3717349708054));
#93322=CARTESIAN_POINT('Ctrl Pts',(0.319190585564614,2.35191763971444,11.3780657518827));
#93323=CARTESIAN_POINT('Ctrl Pts',(0.0211372339985953,2.38083756738751,
11.3994253363191));
#93324=CARTESIAN_POINT('Ctrl Pts',(-0.188506739709662,2.37345469328646,
11.4150076524176));
#93325=CARTESIAN_POINT('Ctrl Pts',(-0.42283064741599,2.33393231051761,11.4318773788699));
#93326=CARTESIAN_POINT('Ctrl Pts',(-0.451112161884432,2.32863130775204,
11.4339022048689));
#93327=CARTESIAN_POINT('Ctrl Pts',(-0.498398188326327,2.31887427747176,
11.4372613320045));
#93328=CARTESIAN_POINT('Ctrl Pts',(-0.517456236963645,2.31469604352611,
11.4386079390715));
#93329=CARTESIAN_POINT('Ctrl Pts',(-0.543904654977684,2.30855456494735,
11.4404646187811));
#93330=CARTESIAN_POINT('Ctrl Pts',(-0.551339724609984,2.30679018664924,
11.4409852210558));
#93331=CARTESIAN_POINT('Ctrl Pts',(-0.563956642936235,2.30373164464393,
11.4418662265307));
#93332=CARTESIAN_POINT('Ctrl Pts',(-0.569142845125659,2.30245586487086,
11.4422276651516));
#93333=CARTESIAN_POINT('Ctrl Pts',(-0.57909769858926,2.29997132972138,11.4429200426354));
#93334=CARTESIAN_POINT('Ctrl Pts',(-0.583866933553731,2.29876524836399,
11.4432511379014));
#93335=CARTESIAN_POINT('Ctrl Pts',(-0.595292538389803,2.2958380005397,11.444042944065));
#93336=CARTESIAN_POINT('Ctrl Pts',(-0.601945292991285,2.29410270000961,
11.4445028493042));
#93337=CARTESIAN_POINT('Ctrl Pts',(-0.626015994683947,2.28771219491465,
11.4461630490712));
#93338=CARTESIAN_POINT('Ctrl Pts',(-0.64338881346191,2.28288720608032,11.4473540451668));
#93339=CARTESIAN_POINT('Ctrl Pts',(-0.817337143860965,2.23243265314062,
11.4592219516021));
#93340=CARTESIAN_POINT('Ctrl Pts',(-0.968890003654601,2.17095925573655,
11.4691145955441));
#93341=CARTESIAN_POINT('Ctrl Pts',(-1.25812779523953,2.0172606012759,11.4891947057542));
#93342=CARTESIAN_POINT('Ctrl Pts',(-1.39486856756935,1.92524203110561,11.499343595851));
#93343=CARTESIAN_POINT('Ctrl Pts',(-1.53703297539754,1.8064232512149,11.5114411077934));
#93344=CARTESIAN_POINT('Ctrl Pts',(-1.55289935963413,1.79280195859577,11.5128146386954));
#93345=CARTESIAN_POINT('Ctrl Pts',(-1.57694263880225,1.77160215253361,11.5149334510505));
#93346=CARTESIAN_POINT('Ctrl Pts',(-1.58524994161057,1.76417257896049,11.5156725441102));
#93347=CARTESIAN_POINT('Ctrl Pts',(-1.59968032694304,1.75108264797422,11.5169689112878));
#93348=CARTESIAN_POINT('Ctrl Pts',(-1.60582654567861,1.74544799137146,11.5175250934476));
#93349=CARTESIAN_POINT('Ctrl Pts',(-1.6196565730175,1.73263418752943,11.5187858389059));
#93350=CARTESIAN_POINT('Ctrl Pts',(-1.62732256226536,1.72543615195478,11.5194912036206));
#93351=CARTESIAN_POINT('Ctrl Pts',(-1.64796510647271,1.70579375062703,11.5214085604858));
#93352=CARTESIAN_POINT('Ctrl Pts',(-1.66084821713925,1.69325263335334,11.5226247280902));
#93353=CARTESIAN_POINT('Ctrl Pts',(-1.72095515472534,1.63339531856916,11.5283932516556));
#93354=CARTESIAN_POINT('Ctrl Pts',(-1.76630308487858,1.58424707079025,11.5330263867347));
#93355=CARTESIAN_POINT('Ctrl Pts',(-1.94707024446076,1.37090971740908,11.5527365772127));
#93356=CARTESIAN_POINT('Ctrl Pts',(-2.06214801574062,1.19079725388771,11.5685542276648));
#93357=CARTESIAN_POINT('Ctrl Pts',(-2.16969885759295,0.958877706868799,
11.5869189200287));
#93358=CARTESIAN_POINT('Ctrl Pts',(-2.18669386321987,0.919461798898741,
11.5899720803374));
#93359=CARTESIAN_POINT('Ctrl Pts',(-2.21231607607138,0.855301382189059,
11.5948111416863));
#93360=CARTESIAN_POINT('Ctrl Pts',(-2.22161890366568,0.830838411411903,
11.5966262597013));
#93361=CARTESIAN_POINT('Ctrl Pts',(-2.23342380052921,0.798178797977387,
11.5990055486539));
#93362=CARTESIAN_POINT('Ctrl Pts',(-2.23628869706746,0.790116532790123,
11.5995893693795));
#93363=CARTESIAN_POINT('Ctrl Pts',(-2.2409339050709,0.776816512772163,11.6005464813377));
#93364=CARTESIAN_POINT('Ctrl Pts',(-2.24273960143134,0.77158780653715,11.6009212366968));
#93365=CARTESIAN_POINT('Ctrl Pts',(-2.24624670962633,0.761316036843849,
11.6016543986206));
#93366=CARTESIAN_POINT('Ctrl Pts',(-2.24794946250798,0.756273497769942,
11.6020128790296));
#93367=CARTESIAN_POINT('Ctrl Pts',(-2.25211206999747,0.743808063695026,
11.6028956137971));
#93368=CARTESIAN_POINT('Ctrl Pts',(-2.25455224422846,0.736378566939867,
11.6034187198306));
#93369=CARTESIAN_POINT('Ctrl Pts',(-2.26286603288817,0.710637175936623,
11.6052212001177));
#93370=CARTESIAN_POINT('Ctrl Pts',(-2.268553841912,0.692265414048133,11.6064902657382));
#93371=CARTESIAN_POINT('Ctrl Pts',(-2.30894440194742,0.555955919685495,
11.6157922643299));
#93372=CARTESIAN_POINT('Ctrl Pts',(-2.33465867338339,0.4355321568156,11.6233886281484));
#93373=CARTESIAN_POINT('Ctrl Pts',(-2.35715246984246,0.266929441770081,
11.6338307018606));
#93374=CARTESIAN_POINT('Ctrl Pts',(-2.36198927731126,0.220052949231025,
11.636712856545));
#93375=CARTESIAN_POINT('Ctrl Pts',(-2.36542649946083,0.173076682856166,
11.6396027579113));
#93376=CARTESIAN_POINT('Origin',(0.,0.,-1.84858989190503));
#93377=CARTESIAN_POINT('',(-2.36542647041237,0.173077079858841,12.8360489723836));
#93378=CARTESIAN_POINT('',(-2.36542649456986,0.173076749700613,12.6375766332401));
#93379=CARTESIAN_POINT('',(-2.36542649454111,0.173076750093529,-1.84858989190503));
#93380=CARTESIAN_POINT('',(-2.37174963818669,-0.00131006156719779,11.848589891905));
#93381=CARTESIAN_POINT('Ctrl Pts',(-2.36542647041237,0.173077079858945,
12.8360489723835));
#93382=CARTESIAN_POINT('Ctrl Pts',(-2.35606773494392,0.300981945279007,
12.8281521841122));
#93383=CARTESIAN_POINT('Ctrl Pts',(-2.3363431353734,0.428017049067247,12.8203717055505));
#93384=CARTESIAN_POINT('Ctrl Pts',(-2.28464375495091,0.643667315178936,
12.8065390961138));
#93385=CARTESIAN_POINT('Ctrl Pts',(-2.25755720211513,0.733032737755073,
12.800615170079));
#93386=CARTESIAN_POINT('Ctrl Pts',(-2.21917847626778,0.837111715874048,
12.7933629177622));
#93387=CARTESIAN_POINT('Ctrl Pts',(-2.21289219884968,0.853590781881691,
12.7922039820895));
#93388=CARTESIAN_POINT('Ctrl Pts',(-2.20225036896525,0.880579787429406,
12.7902875255786));
#93389=CARTESIAN_POINT('Ctrl Pts',(-2.19800187463305,0.891131416285915,
12.789533600331));
#93390=CARTESIAN_POINT('Ctrl Pts',(-2.19020719438395,0.910095515251465,
12.7881699665518));
#93391=CARTESIAN_POINT('Ctrl Pts',(-2.18668800523133,0.918518897451735,
12.7875611820615));
#93392=CARTESIAN_POINT('Ctrl Pts',(-2.17906042183177,0.936483665279753,
12.7862560801617));
#93393=CARTESIAN_POINT('Ctrl Pts',(-2.17493780693871,0.946018766890751,
12.7855592881573));
#93394=CARTESIAN_POINT('Ctrl Pts',(-2.16357194478324,0.971839589622956,
12.7836610889731));
#93395=CARTESIAN_POINT('Ctrl Pts',(-2.15620766256164,0.988070965971559,
12.7824555578848));
#93396=CARTESIAN_POINT('Ctrl Pts',(-2.1159048721436,1.07430433019118,12.7759835140258));
#93397=CARTESIAN_POINT('Ctrl Pts',(-2.07974251957415,1.14273877256405,12.7706061953141));
#93398=CARTESIAN_POINT('Ctrl Pts',(-1.94880486517025,1.36365799016943,12.7524168287233));
#93399=CARTESIAN_POINT('Ctrl Pts',(-1.8400835003389,1.50714380891038,12.739166396794));
#93400=CARTESIAN_POINT('Ctrl Pts',(-1.65761357994921,1.69844996953126,12.7200089406634));
#93401=CARTESIAN_POINT('Ctrl Pts',(-1.59571137233223,1.75673666041239,12.7139331338335));
#93402=CARTESIAN_POINT('Ctrl Pts',(-1.52132145846156,1.81959702240994,12.7072155350567));
#93403=CARTESIAN_POINT('Ctrl Pts',(-1.51177224445391,1.82753850895172,12.7063636368404));
#93404=CARTESIAN_POINT('Ctrl Pts',(-1.49720938408593,1.83945727371353,12.7050807199793));
#93405=CARTESIAN_POINT('Ctrl Pts',(-1.49224148378928,1.84348972281503,12.7046459012025));
#93406=CARTESIAN_POINT('Ctrl Pts',(-1.48327676998334,1.8507064051526,12.7038664240597));
#93407=CARTESIAN_POINT('Ctrl Pts',(-1.4792859518208,1.8538978528328,12.7035212568702));
#93408=CARTESIAN_POINT('Ctrl Pts',(-1.47050864244129,1.86087065690813,12.7027661165795));
#93409=CARTESIAN_POINT('Ctrl Pts',(-1.4657178742443,1.86464645026411,12.7023565382014));
#93410=CARTESIAN_POINT('Ctrl Pts',(-1.45194618439726,1.87541459067877,12.7011863685152));
#93411=CARTESIAN_POINT('Ctrl Pts',(-1.44292926979051,1.88236094961915,12.7004289491399));
#93412=CARTESIAN_POINT('Ctrl Pts',(-1.37969775193045,1.93035124743972,12.6951753731801));
#93413=CARTESIAN_POINT('Ctrl Pts',(-1.32378416836302,1.96911637460261,12.6908240028276));
#93414=CARTESIAN_POINT('Ctrl Pts',(-1.17005891447933,2.06618221427086,12.679400865298));
#93415=CARTESIAN_POINT('Ctrl Pts',(-1.06958912676756,2.11993603110896,12.672479844408));
#93416=CARTESIAN_POINT('Ctrl Pts',(-0.82255275993492,2.23005571265998,12.6558891548033));
#93417=CARTESIAN_POINT('Ctrl Pts',(-0.673516270180621,2.27949717173543,
12.6461870604574));
#93418=CARTESIAN_POINT('Ctrl Pts',(-0.50242712754327,2.31799829278613,12.6347358987047));
#93419=CARTESIAN_POINT('Ctrl Pts',(-0.484100493126899,2.32189486912513,
12.6335058811391));
#93420=CARTESIAN_POINT('Ctrl Pts',(-0.454250284891734,2.32787280823238,
12.6314960258739));
#93421=CARTESIAN_POINT('Ctrl Pts',(-0.442753842407921,2.33008672785577,
12.6307204181275));
#93422=CARTESIAN_POINT('Ctrl Pts',(-0.422232100826143,2.33388133006991,
12.6293329739657));
#93423=CARTESIAN_POINT('Ctrl Pts',(-0.413213082437357,2.33549501268254,
12.6287222016824));
#93424=CARTESIAN_POINT('Ctrl Pts',(-0.394151465843454,2.33879164707092,
12.6274291042052));
#93425=CARTESIAN_POINT('Ctrl Pts',(-0.384106951172826,2.34046226008409,
12.6267464001119));
#93426=CARTESIAN_POINT('Ctrl Pts',(-0.357376503131531,2.3447313847967,12.6249259585009));
#93427=CARTESIAN_POINT('Ctrl Pts',(-0.340673302158004,2.34721641679052,
12.6237846534411));
#93428=CARTESIAN_POINT('Ctrl Pts',(-0.259814788672728,2.35836495300144,
12.618240506892));
#93429=CARTESIAN_POINT('Ctrl Pts',(-0.19535506929162,2.36457691001498,12.6137613558711));
#93430=CARTESIAN_POINT('Ctrl Pts',(-0.00485393088076005,2.37509301603323,
12.6003388772199));
#93431=CARTESIAN_POINT('Ctrl Pts',(0.121358647631846,2.37199399727277,12.5911966475466));
#93432=CARTESIAN_POINT('Ctrl Pts',(0.388785252323727,2.34402424437078,12.571560140891));
#93433=CARTESIAN_POINT('Ctrl Pts',(0.529238990277415,2.31635868357233,12.5610858361816));
#93434=CARTESIAN_POINT('Ctrl Pts',(0.684493093102304,2.2709082493408,12.5498341333594));
#93435=CARTESIAN_POINT('Ctrl Pts',(0.702563347279203,2.2653829413902,12.5485300207484));
#93436=CARTESIAN_POINT('Ctrl Pts',(0.72790197640617,2.25730282832479,12.5467109541578));
#93437=CARTESIAN_POINT('Ctrl Pts',(0.735226307769165,2.25492785396476,12.5461862754249));
#93438=CARTESIAN_POINT('Ctrl Pts',(0.747520226384744,2.25087518130282,12.5453076664023));
#93439=CARTESIAN_POINT('Ctrl Pts',(0.752496001043641,2.24921660604805,12.5449526343317));
#93440=CARTESIAN_POINT('Ctrl Pts',(0.76263239081832,2.24580044050981,12.5442306053293));
#93441=CARTESIAN_POINT('Ctrl Pts',(0.767792511293143,2.24404154223208,12.5438636878979));
#93442=CARTESIAN_POINT('Ctrl Pts',(0.780913427851679,2.2395185405404,12.5429322405364));
#93443=CARTESIAN_POINT('Ctrl Pts',(0.788865726378963,2.23672974370719,12.5423691516418));
#93444=CARTESIAN_POINT('Ctrl Pts',(0.821028324450116,2.22525775496071,12.5400969700308));
#93445=CARTESIAN_POINT('Ctrl Pts',(0.845112589981845,2.21622301019967,12.5384074654129));
#93446=CARTESIAN_POINT('Ctrl Pts',(1.05600421064026,2.13317299647554,12.5236793870371));
#93447=CARTESIAN_POINT('Ctrl Pts',(1.23287404369968,2.03607888089212,12.5117313107034));
#93448=CARTESIAN_POINT('Ctrl Pts',(1.49074142258947,1.84845630951112,12.4920147250766));
#93449=CARTESIAN_POINT('Ctrl Pts',(1.58076641462966,1.77208143429755,12.4846005599742));
#93450=CARTESIAN_POINT('Ctrl Pts',(1.67789638566955,1.67636610087405,12.4756936648348));
#93451=CARTESIAN_POINT('Ctrl Pts',(1.6909070854809,1.66324164860357,12.4744801846674));
#93452=CARTESIAN_POINT('Ctrl Pts',(1.71185400983552,1.64161176466272,12.4724920311026));
#93453=CARTESIAN_POINT('Ctrl Pts',(1.7198835383517,1.63319745995434,12.471721435965));
#93454=CARTESIAN_POINT('Ctrl Pts',(1.73412126837785,1.61805601823492,12.4703395612563));
#93455=CARTESIAN_POINT('Ctrl Pts',(1.74035306812792,1.61135131048464,12.4697293133933));
#93456=CARTESIAN_POINT('Ctrl Pts',(1.7534645154553,1.59708009659783,12.4684337546282));
#93457=CARTESIAN_POINT('Ctrl Pts',(1.76033433176788,1.58950485265617,12.4677480439879));
#93458=CARTESIAN_POINT('Ctrl Pts',(1.77855096422581,1.56915470088022,12.465911041696));
#93459=CARTESIAN_POINT('Ctrl Pts',(1.78980890449678,1.55630140599897,12.4647560668156));
#93460=CARTESIAN_POINT('Ctrl Pts',(1.8446541315599,1.49230189122682,12.4590298785491));
#93461=CARTESIAN_POINT('Ctrl Pts',(1.88618897482562,1.43944551079255,12.4543761387991));
#93462=CARTESIAN_POINT('Ctrl Pts',(2.02113660601206,1.25182860022656,12.4380949475774));
#93463=CARTESIAN_POINT('Ctrl Pts',(2.10278865374118,1.10920459075496,12.4260786076668));
#93464=CARTESIAN_POINT('Ctrl Pts',(2.21422658430922,0.857239424342937,12.4059936371435));
#93465=CARTESIAN_POINT('Ctrl Pts',(2.25212017600938,0.752076971148706,12.3979248669931));
#93466=CARTESIAN_POINT('Ctrl Pts',(2.28590605106344,0.632448935515872,12.3893479250914));
#93467=CARTESIAN_POINT('Ctrl Pts',(2.2892473344159,0.620245749674566,12.3884798672354));
#93468=CARTESIAN_POINT('Ctrl Pts',(2.29414390523984,0.601783500918453,12.3871775289299));
#93469=CARTESIAN_POINT('Ctrl Pts',(2.2957715147325,0.59554411640029,12.3867392788263));
#93470=CARTESIAN_POINT('Ctrl Pts',(2.29864398228552,0.584345825407138,12.3859561809711));
#93471=CARTESIAN_POINT('Ctrl Pts',(2.29989826553795,0.579389481063552,12.3856108023295));
#93472=CARTESIAN_POINT('Ctrl Pts',(2.30260404487247,0.568550250927201,12.3848581481269));
#93473=CARTESIAN_POINT('Ctrl Pts',(2.30404902610744,0.562665853478704,12.3844512487079));
#93474=CARTESIAN_POINT('Ctrl Pts',(2.30809865683415,0.545897333012012,12.3832963934355));
#93475=CARTESIAN_POINT('Ctrl Pts',(2.31064888673934,0.535000039638957,12.3825514812315));
#93476=CARTESIAN_POINT('Ctrl Pts',(2.32711912547624,0.462306330343109,12.3776169731133));
#93477=CARTESIAN_POINT('Ctrl Pts',(2.33863719708616,0.399985348311733,12.3735528005308));
#93478=CARTESIAN_POINT('Ctrl Pts',(2.37728317734301,0.130982429178014,12.3564287251144));
#93479=CARTESIAN_POINT('Ctrl Pts',(2.37960264702573,-0.0783174123443216,
12.3440742507437));
#93480=CARTESIAN_POINT('Ctrl Pts',(2.34591034384298,-0.356435490283239,
12.3264204073041));
#93481=CARTESIAN_POINT('Ctrl Pts',(2.33406101627076,-0.427199238427661,
12.32182770077));
#93482=CARTESIAN_POINT('Ctrl Pts',(2.31525624335746,-0.514888038666354,
12.3159560017653));
#93483=CARTESIAN_POINT('Ctrl Pts',(2.31128761459492,-0.532419663290725,
12.3147730170809));
#93484=CARTESIAN_POINT('Ctrl Pts',(2.30467974237471,-0.560142961923467,
12.3128871800042));
#93485=CARTESIAN_POINT('Ctrl Pts',(2.30217120102222,-0.570365328364844,
12.3121885351723));
#93486=CARTESIAN_POINT('Ctrl Pts',(2.29758651514182,-0.588524913025164,
12.3109414253755));
#93487=CARTESIAN_POINT('Ctrl Pts',(2.29553706142036,-0.59646874565259,12.3103938314597));
#93488=CARTESIAN_POINT('Ctrl Pts',(2.29069739161007,-0.614833226718215,
12.3091230737177));
#93489=CARTESIAN_POINT('Ctrl Pts',(2.28787722908984,-0.62524572331864,12.3083989486524));
#93490=CARTESIAN_POINT('Ctrl Pts',(2.27971428742474,-0.654589776074706,
12.3063478230348));
#93491=CARTESIAN_POINT('Ctrl Pts',(2.27420698443403,-0.673474244801376,
12.3050155035089));
#93492=CARTESIAN_POINT('Ctrl Pts',(2.23483163110694,-0.802498137360569,
12.2958257456054));
#93493=CARTESIAN_POINT('Ctrl Pts',(2.19321637907314,-0.910093476021869,
12.2877138794145));
#93494=CARTESIAN_POINT('Ctrl Pts',(2.09129036916141,-1.12555323577651,12.2705542391789));
#93495=CARTESIAN_POINT('Ctrl Pts',(2.03003559349758,-1.23260631517048,12.2615050221484));
#93496=CARTESIAN_POINT('Ctrl Pts',(1.90464445431768,-1.41685284445431,12.24529276088));
#93497=CARTESIAN_POINT('Ctrl Pts',(1.84338731891017,-1.49568398995831,12.2381178430359));
#93498=CARTESIAN_POINT('Ctrl Pts',(1.76900299540287,-1.57986867898435,12.2303673485928));
#93499=CARTESIAN_POINT('Ctrl Pts',(1.76058954843799,-1.58923915760572,12.2295033946705));
#93500=CARTESIAN_POINT('Ctrl Pts',(1.74776416978858,-1.60329656791619,12.2282059854648));
#93501=CARTESIAN_POINT('Ctrl Pts',(1.74340730599584,-1.60803309847282,12.2277686038911));
#93502=CARTESIAN_POINT('Ctrl Pts',(1.73555516583002,-1.61650006496254,12.2269864263259));
#93503=CARTESIAN_POINT('Ctrl Pts',(1.73206707478199,-1.62023697147171,12.2266411050223));
#93504=CARTESIAN_POINT('Ctrl Pts',(1.72441117933843,-1.62838600526204,12.2258878387564));
#93505=CARTESIAN_POINT('Ctrl Pts',(1.72023851783465,-1.6327934166372,12.2254802745631));
#93506=CARTESIAN_POINT('Ctrl Pts',(1.70829116152186,-1.64531628372208,12.2243216262572));
#93507=CARTESIAN_POINT('Ctrl Pts',(1.70047550841215,-1.65339270102136,12.2235736173354));
#93508=CARTESIAN_POINT('Ctrl Pts',(1.64745543957182,-1.70740809577045,12.2185631966282));
#93509=CARTESIAN_POINT('Ctrl Pts',(1.60044747670877,-1.7515482964563,12.2144306823717));
#93510=CARTESIAN_POINT('Ctrl Pts',(1.38441620311257,-1.93843036952047,12.1964443020986));
#93511=CARTESIAN_POINT('Ctrl Pts',(1.1977177272017,-2.05902993834745,12.1833703320896));
#93512=CARTESIAN_POINT('Ctrl Pts',(0.942756714893098,-2.17714994840492,
12.1655455347075));
#93513=CARTESIAN_POINT('Ctrl Pts',(0.887585217542133,-2.20021899945823,
12.1616979643798));
#93514=CARTESIAN_POINT('Ctrl Pts',(0.815566149410654,-2.22718279675057,
12.1566572614387));
#93515=CARTESIAN_POINT('Ctrl Pts',(0.799463421086969,-2.23301356174213,
12.1555291278441));
#93516=CARTESIAN_POINT('Ctrl Pts',(0.773638538234104,-2.24204956037999,
12.1537175022365));
#93517=CARTESIAN_POINT('Ctrl Pts',(0.763956123348106,-2.24536719826278,
12.1530377500073));
#93518=CARTESIAN_POINT('Ctrl Pts',(0.746443533552262,-2.25124142587276,
12.1518071974261));
#93519=CARTESIAN_POINT('Ctrl Pts',(0.738620895303357,-2.25382010737616,
12.1512571380354));
#93520=CARTESIAN_POINT('Ctrl Pts',(0.720162245803472,-2.25979846083852,
12.1499581981002));
#93521=CARTESIAN_POINT('Ctrl Pts',(0.709515421087032,-2.26316384817905,
12.1492082028278));
#93522=CARTESIAN_POINT('Ctrl Pts',(0.678322916728101,-2.27278184126134,
12.1470084213232));
#93523=CARTESIAN_POINT('Ctrl Pts',(0.657716059689079,-2.27883057928905,
12.1455520207085));
#93524=CARTESIAN_POINT('Ctrl Pts',(0.610867650235644,-2.29189364710916,
12.142232947073));
#93525=CARTESIAN_POINT('Ctrl Pts',(0.584582417250348,-2.29873858178577,
12.1403650455487));
#93526=CARTESIAN_POINT('Ctrl Pts',(0.49783069366546,-2.31974547509101,12.1341802218074));
#93527=CARTESIAN_POINT('Ctrl Pts',(0.436929231563304,-2.33198331257253,
12.1298058532488));
#93528=CARTESIAN_POINT('Ctrl Pts',(0.225629867591638,-2.36587525163351,
12.114529217183));
#93529=CARTESIAN_POINT('Ctrl Pts',(0.073680596841483,-2.37546600742856,
12.1033444936368));
#93530=CARTESIAN_POINT('Ctrl Pts',(-0.17207963563285,-2.36736646961638,
12.0854811719907));
#93531=CARTESIAN_POINT('Ctrl Pts',(-0.265780658862212,-2.35868615061329,
12.0787329602207));
#93532=CARTESIAN_POINT('Ctrl Pts',(-0.371103757731314,-2.34257055062827,
12.0713827347762));
#93533=CARTESIAN_POINT('Ctrl Pts',(-0.383463724610208,-2.34057906784625,
12.0705239228831));
#93534=CARTESIAN_POINT('Ctrl Pts',(-0.402137332892034,-2.33741841361116,
12.0692326926835));
#93535=CARTESIAN_POINT('Ctrl Pts',(-0.408462706337029,-2.33632135948874,
12.0687964021201));
#93536=CARTESIAN_POINT('Ctrl Pts',(-0.419815897497135,-2.33430477814219,
12.0680153769536));
#93537=CARTESIAN_POINT('Ctrl Pts',(-0.4248452432866,-2.3333946742645,12.0676701240523));
#93538=CARTESIAN_POINT('Ctrl Pts',(-0.435853078785655,-2.33136594027574,
12.0669160725928));
#93539=CARTESIAN_POINT('Ctrl Pts',(-0.441830213195607,-2.33024057096689,
12.0665076606881));
#93540=CARTESIAN_POINT('Ctrl Pts',(-0.458898566651858,-2.32695892307695,
12.0653441687326));
#93541=CARTESIAN_POINT('Ctrl Pts',(-0.46997898575835,-2.32474632805144,
12.0645922043718));
#93542=CARTESIAN_POINT('Ctrl Pts',(-0.545578830159945,-2.30908754625109,
12.0594819550371));
#93543=CARTESIAN_POINT('Ctrl Pts',(-0.609536025152879,-2.29303493789077,
12.0552595773158));
#93544=CARTESIAN_POINT('Ctrl Pts',(-0.904911489605285,-2.205663028194,12.0358813908219));
#93545=CARTESIAN_POINT('Ctrl Pts',(-1.12518949672044,-2.10185057478262,
12.0216307117774));
#93546=CARTESIAN_POINT('Ctrl Pts',(-1.36050765592221,-1.9431814559665,12.0034170239728));
#93547=CARTESIAN_POINT('Ctrl Pts',(-1.39444328665845,-1.91897442120173,
12.0007125620712));
#93548=CARTESIAN_POINT('Ctrl Pts',(-1.43968765107578,-1.88486659373644,
11.9969892736025));
#93549=CARTESIAN_POINT('Ctrl Pts',(-1.4515673593749,-1.8757331347399,11.9960002774887));
#93550=CARTESIAN_POINT('Ctrl Pts',(-1.47027699438294,-1.86106445018852,
11.9944240809229));
#93551=CARTESIAN_POINT('Ctrl Pts',(-1.47716420689636,-1.85560265958887,
11.9938398024196));
#93552=CARTESIAN_POINT('Ctrl Pts',(-1.49092078031622,-1.84456811508778,
11.9926644770238));
#93553=CARTESIAN_POINT('Ctrl Pts',(-1.49778964198804,-1.83899496711279,
11.9920734201814));
#93554=CARTESIAN_POINT('Ctrl Pts',(-1.51342276000333,-1.82616512999928,
11.9907184680965));
#93555=CARTESIAN_POINT('Ctrl Pts',(-1.52216623614718,-1.81888357906503,
11.9899535705416));
#93556=CARTESIAN_POINT('Ctrl Pts',(-1.54048618929852,-1.80340214702337,
11.988335715211));
#93557=CARTESIAN_POINT('Ctrl Pts',(-1.55005032989432,-1.79518828187048,
11.9874821960715));
#93558=CARTESIAN_POINT('Ctrl Pts',(-1.57513333713836,-1.7732966305736,11.9852198552338));
#93559=CARTESIAN_POINT('Ctrl Pts',(-1.59053923865441,-1.75949164615021,
11.9838057957537));
#93560=CARTESIAN_POINT('Ctrl Pts',(-1.63672087828426,-1.71700681629142,
11.9794908104552));
#93561=CARTESIAN_POINT('Ctrl Pts',(-1.66691460379,-1.68770938383527,11.976564478804));
#93562=CARTESIAN_POINT('Ctrl Pts',(-1.78195078869128,-1.56998848409578,
11.964991870471));
#93563=CARTESIAN_POINT('Ctrl Pts',(-1.86065982669846,-1.47585600260169,
11.9561175708611));
#93564=CARTESIAN_POINT('Ctrl Pts',(-2.01750629648703,-1.25567487222783,
11.9363815122469));
#93565=CARTESIAN_POINT('Ctrl Pts',(-2.09183833882191,-1.12750675773355,
11.9255257575701));
#93566=CARTESIAN_POINT('Ctrl Pts',(-2.16160415564647,-0.976225718645316,
11.9139406478406));
#93567=CARTESIAN_POINT('Ctrl Pts',(-2.1692496899174,-0.959116790364344,
11.9126475062581));
#93568=CARTESIAN_POINT('Ctrl Pts',(-2.17973939876882,-0.93487598023036,
11.9108410383354));
#93569=CARTESIAN_POINT('Ctrl Pts',(-2.18275271289591,-0.927818701829088,
11.9103181619321));
#93570=CARTESIAN_POINT('Ctrl Pts',(-2.18776590014456,-0.915918054796384,
11.90944170194));
#93571=CARTESIAN_POINT('Ctrl Pts',(-2.18978405116351,-0.911082503444913,
11.9090870283239));
#93572=CARTESIAN_POINT('Ctrl Pts',(-2.19387196532615,-0.901195683531819,
11.9083648836178));
#93573=CARTESIAN_POINT('Ctrl Pts',(-2.19594033983021,-0.896143897883778,
11.9079974966213));
#93574=CARTESIAN_POINT('Ctrl Pts',(-2.2011696350024,-0.883245076971879,
11.9070634061276));
#93575=CARTESIAN_POINT('Ctrl Pts',(-2.20430608135312,-0.875388104350973,
11.9064981599046));
#93576=CARTESIAN_POINT('Ctrl Pts',(-2.21690665526246,-0.843325796305487,
11.9042060289159));
#93577=CARTESIAN_POINT('Ctrl Pts',(-2.2260150938633,-0.818981353842017,
11.9024991681499));
#93578=CARTESIAN_POINT('Ctrl Pts',(-2.24901633442402,-0.754284099745273,
11.8980386295231));
#93579=CARTESIAN_POINT('Ctrl Pts',(-2.26222390730116,-0.713696310960525,
11.8953169159556));
#93580=CARTESIAN_POINT('Ctrl Pts',(-2.3388271031152,-0.454736390244581,
11.8783027396771));
#93581=CARTESIAN_POINT('Ctrl Pts',(-2.37163529115258,-0.228570848616063,
11.8648854578643));
#93582=CARTESIAN_POINT('Ctrl Pts',(-2.37174969976493,-0.00119338383973933,
11.8504244921034));
#93583=CARTESIAN_POINT('Ctrl Pts',(-2.36542649454111,0.173076750093539,
11.8369288124873));
#93584=CARTESIAN_POINT('Ctrl Pts',(-2.36967174016765,0.115057307993937,
11.8408158389598));
#93585=CARTESIAN_POINT('Ctrl Pts',(-2.37178177616025,0.0568728735571407,
11.8447028654324));
#93586=CARTESIAN_POINT('Ctrl Pts',(-2.37174963818669,-0.00131006156719779,
11.848589891905));
#93587=CARTESIAN_POINT('Ctrl Pts',(-2.36542649946083,0.173076682856166,
11.6396027579113));
#93588=CARTESIAN_POINT('Ctrl Pts',(-2.36959623365429,0.1160892273876,11.6431085308926));
#93589=CARTESIAN_POINT('Ctrl Pts',(-2.37170628631787,0.0589549541247075,
11.6466259165959));
#93590=CARTESIAN_POINT('Ctrl Pts',(-2.37182455093614,-0.0981284232074804,
11.6563981685599));
#93591=CARTESIAN_POINT('Ctrl Pts',(-2.36558630217958,-0.197935735150465,
11.6627245204279));
#93592=CARTESIAN_POINT('Ctrl Pts',(-2.35081326271615,-0.314962274922296,
11.6704326954118));
#93593=CARTESIAN_POINT('Ctrl Pts',(-2.34834683170767,-0.332853359734494,
11.6716190245502));
#93594=CARTESIAN_POINT('Ctrl Pts',(-2.34396258522252,-0.362176453446736,
11.6735771943546));
#93595=CARTESIAN_POINT('Ctrl Pts',(-2.34216482705472,-0.373625881301496,
11.6743452435663));
#93596=CARTESIAN_POINT('Ctrl Pts',(-2.33877890187598,-0.394204474395164,
11.6757321432583));
#93597=CARTESIAN_POINT('Ctrl Pts',(-2.33722100363748,-0.403338437863,11.6763500223956));
#93598=CARTESIAN_POINT('Ctrl Pts',(-2.33378238593744,-0.422809930002291,
11.6776722053028));
#93599=CARTESIAN_POINT('Ctrl Pts',(-2.33188641944024,-0.433144528398698,
11.678376981936));
#93600=CARTESIAN_POINT('Ctrl Pts',(-2.32656749480987,-0.461089573958851,
11.680291084235));
#93601=CARTESIAN_POINT('Ctrl Pts',(-2.32301335243347,-0.478674040081191,
11.6815045612319));
#93602=CARTESIAN_POINT('Ctrl Pts',(-2.30323052530042,-0.571136828715468,
11.687934324282));
#93603=CARTESIAN_POINT('Ctrl Pts',(-2.28358180661259,-0.645228611194144,
11.6932589213851));
#93604=CARTESIAN_POINT('Ctrl Pts',(-2.20751111334827,-0.884634207657342,
11.7110456201859));
#93605=CARTESIAN_POINT('Ctrl Pts',(-2.1364273626775,-1.04467606348235,11.7239177483709));
#93606=CARTESIAN_POINT('Ctrl Pts',(-2.03686802877451,-1.21527527682117,
11.7382509404802));
#93607=CARTESIAN_POINT('Ctrl Pts',(-2.02500620526152,-1.23493938154839,
11.7399120354391));
#93608=CARTESIAN_POINT('Ctrl Pts',(-2.00184950378918,-1.27209670753443,
11.7430644666016));
#93609=CARTESIAN_POINT('Ctrl Pts',(-1.99060611869413,-1.2896196311958,11.7445570357783));
#93610=CARTESIAN_POINT('Ctrl Pts',(-1.95217770154501,-1.34781043652375,
11.7495284848437));
#93611=CARTESIAN_POINT('Ctrl Pts',(-1.9239635207587,-1.38778814670646,11.7529687934974));
#93612=CARTESIAN_POINT('Ctrl Pts',(-1.88795647903233,-1.43559667391641,
11.7570874539934));
#93613=CARTESIAN_POINT('Ctrl Pts',(-1.88132186638304,-1.44428027874177,
11.7578357159257));
#93614=CARTESIAN_POINT('Ctrl Pts',(-1.87087758208135,-1.45775601626811,
11.7589967919351));
#93615=CARTESIAN_POINT('Ctrl Pts',(-1.8671090815316,-1.46257964224885,11.7594123731986));
#93616=CARTESIAN_POINT('Ctrl Pts',(-1.86011117379989,-1.47146573681321,
11.7601778280249));
#93617=CARTESIAN_POINT('Ctrl Pts',(-1.8568871262365,-1.47553217344705,11.7605280538438));
#93618=CARTESIAN_POINT('Ctrl Pts',(-1.84954328921449,-1.48473263993862,
11.7613203479538));
#93619=CARTESIAN_POINT('Ctrl Pts',(-1.84541546175541,-1.48986011656763,
11.7617618339506));
#93620=CARTESIAN_POINT('Ctrl Pts',(-1.83277473702483,-1.50542894647073,
11.7631023779214));
#93621=CARTESIAN_POINT('Ctrl Pts',(-1.82419399567672,-1.51581523833169,
11.7639967333131));
#93622=CARTESIAN_POINT('Ctrl Pts',(-1.73479520031837,-1.62216655976194,
11.7731618589147));
#93623=CARTESIAN_POINT('Ctrl Pts',(-1.64655942654343,-1.71166299888996,
11.7809415742957));
#93624=CARTESIAN_POINT('Ctrl Pts',(-1.40119912694303,-1.92390444857523,
11.8008780037958));
#93625=CARTESIAN_POINT('Ctrl Pts',(-1.23500072290513,-2.03458386946986,
11.8129164911346));
#93626=CARTESIAN_POINT('Ctrl Pts',(-1.03229502946698,-2.13549133354626,
11.8276128455799));
#93627=CARTESIAN_POINT('Ctrl Pts',(-1.0074340089395,-2.14733157146981,11.8294138310938));
#93628=CARTESIAN_POINT('Ctrl Pts',(-0.971175851169719,-2.16383152693151,
11.8320410710148));
#93629=CARTESIAN_POINT('Ctrl Pts',(-0.959939098430491,-2.16883985773658,
11.8328553571061));
#93630=CARTESIAN_POINT('Ctrl Pts',(-0.940063593668559,-2.17751384803638,
11.8342960449378));
#93631=CARTESIAN_POINT('Ctrl Pts',(-0.931441029128828,-2.18121611112737,
11.8349211823653));
#93632=CARTESIAN_POINT('Ctrl Pts',(-0.913555284592143,-2.18877030450605,
11.8362182739056));
#93633=CARTESIAN_POINT('Ctrl Pts',(-0.904289196384707,-2.19261481976058,
11.8368904646495));
#93634=CARTESIAN_POINT('Ctrl Pts',(-0.880390017669219,-2.20235336472459,
11.8386248621339));
#93635=CARTESIAN_POINT('Ctrl Pts',(-0.865722204170377,-2.20816031359601,
11.8396899778674));
#93636=CARTESIAN_POINT('Ctrl Pts',(-0.80299897555544,-2.23227127284158,
11.8442482423697));
#93637=CARTESIAN_POINT('Ctrl Pts',(-0.754416266272933,-2.24915490192749,
11.8477881597181));
#93638=CARTESIAN_POINT('Ctrl Pts',(-0.622281848918048,-2.2903119527519,
11.8574482534792));
#93639=CARTESIAN_POINT('Ctrl Pts',(-0.537885812885933,-2.31158810627116,
11.8636547190824));
#93640=CARTESIAN_POINT('Ctrl Pts',(-0.327848848092087,-2.35241221418634,
11.8791328044994));
#93641=CARTESIAN_POINT('Ctrl Pts',(-0.201437396552722,-2.36659033516052,
11.8884831905037));
#93642=CARTESIAN_POINT('Ctrl Pts',(-0.0426416812214114,-2.37158085773896,
11.8999769382039));
#93643=CARTESIAN_POINT('Ctrl Pts',(-0.0107643246538707,-2.37193978609064,
11.9022707201288));
#93644=CARTESIAN_POINT('Ctrl Pts',(0.071640998922669,-2.37120624349076,
11.908151461428));
#93645=CARTESIAN_POINT('Ctrl Pts',(0.122147670897993,-2.36914168456474,
11.911708426109));
#93646=CARTESIAN_POINT('Ctrl Pts',(0.182594302802936,-2.3647322741372,11.9158798583456));
#93647=CARTESIAN_POINT('Ctrl Pts',(0.19263012313159,-2.36393592393366,11.9165695873291));
#93648=CARTESIAN_POINT('Ctrl Pts',(0.209090280969267,-2.36252427697597,
11.9176958406146));
#93649=CARTESIAN_POINT('Ctrl Pts',(0.215517592028784,-2.36194662829993,
11.9181343640749));
#93650=CARTESIAN_POINT('Ctrl Pts',(0.227102627741073,-2.36085775100345,
11.9189224341041));
#93651=CARTESIAN_POINT('Ctrl Pts',(0.232261071664863,-2.36035584608223,
11.919272486155));
#93652=CARTESIAN_POINT('Ctrl Pts',(0.243613907791586,-2.35921366228933,
11.9200410179082));
#93653=CARTESIAN_POINT('Ctrl Pts',(0.249807431062139,-2.35856589690526,
11.9204590742562));
#93654=CARTESIAN_POINT('Ctrl Pts',(0.267664225999971,-2.35662717030328,
11.9216610701236));
#93655=CARTESIAN_POINT('Ctrl Pts',(0.279320770099191,-2.35527401361631,
11.9224416204349));
#93656=CARTESIAN_POINT('Ctrl Pts',(0.364929552630402,-2.34469156202545,
11.928147306832));
#93657=CARTESIAN_POINT('Ctrl Pts',(0.438428712567298,-2.33206665864493,
11.9328986979669));
#93658=CARTESIAN_POINT('Ctrl Pts',(0.617695503759055,-2.2924964502961,11.9443907556221));
#93659=CARTESIAN_POINT('Ctrl Pts',(0.722429270633916,-2.26167766636787,
11.9510242136761));
#93660=CARTESIAN_POINT('Ctrl Pts',(0.841401620177135,-2.21755713456954,
11.9588110880807));
#93661=CARTESIAN_POINT('Ctrl Pts',(0.858057935173975,-2.21116550814914,
11.9599070361984));
#93662=CARTESIAN_POINT('Ctrl Pts',(1.0008640482178,-2.15450907927809,11.9693628610977));
#93663=CARTESIAN_POINT('Ctrl Pts',(1.12253593727548,-2.09369138937848,11.9778412394494));
#93664=CARTESIAN_POINT('Ctrl Pts',(1.25449414574158,-2.01290879205647,11.9879421080169));
#93665=CARTESIAN_POINT('Ctrl Pts',(1.27054103798402,-2.00281871455946,11.9891863179932));
#93666=CARTESIAN_POINT('Ctrl Pts',(1.29642903469795,-1.98610435061953,11.9912205263249));
#93667=CARTESIAN_POINT('Ctrl Pts',(1.30634462536221,-1.97959653583522,11.9920062076588));
#93668=CARTESIAN_POINT('Ctrl Pts',(1.32394184032688,-1.96785732032023,11.9934124986577));
#93669=CARTESIAN_POINT('Ctrl Pts',(1.33164236760114,-1.9626545876158,11.994032021487));
#93670=CARTESIAN_POINT('Ctrl Pts',(1.34784685583916,-1.95156702726821,11.9953445770752));
#93671=CARTESIAN_POINT('Ctrl Pts',(1.35634328089878,-1.94567158256411,11.9960380044172));
#93672=CARTESIAN_POINT('Ctrl Pts',(1.37885570983498,-1.92983168460018,11.9978894616934));
#93673=CARTESIAN_POINT('Ctrl Pts',(1.39280242502703,-1.91979029508999,11.9990511901485));
#93674=CARTESIAN_POINT('Ctrl Pts',(1.46016377223315,-1.87017093023593,12.0047356264163));
#93675=CARTESIAN_POINT('Ctrl Pts',(1.51200260238899,-1.82851419447806,12.0093387995779));
#93676=CARTESIAN_POINT('Ctrl Pts',(1.75722529389617,-1.6138930943348,12.0322888624608));
#93677=CARTESIAN_POINT('Ctrl Pts',(1.92303952204303,-1.41222304429458,12.0518396134128));
#93678=CARTESIAN_POINT('Ctrl Pts',(2.05509743430012,-1.18397280798937,12.0702881863535));
#93679=CARTESIAN_POINT('Ctrl Pts',(2.0572706208332,-1.18019264012371,12.0705927341295));
#93680=CARTESIAN_POINT('Ctrl Pts',(2.06992069561689,-1.15804724477495,12.0723710057368));
#93681=CARTESIAN_POINT('Ctrl Pts',(2.08016249855412,-1.13954778968523,12.0738329796942));
#93682=CARTESIAN_POINT('Ctrl Pts',(2.09400056181127,-1.113744083999,12.0758373220238));
#93683=CARTESIAN_POINT('Ctrl Pts',(2.0978083152236,-1.10655524715962,12.0763920251162));
#93684=CARTESIAN_POINT('Ctrl Pts',(2.10385009840324,-1.0950054024846,12.0772771467267));
#93685=CARTESIAN_POINT('Ctrl Pts',(2.10610768911218,-1.09065689884886,12.0776090203251));
#93686=CARTESIAN_POINT('Ctrl Pts',(2.11080590477986,-1.08153835061618,12.078302018622));
#93687=CARTESIAN_POINT('Ctrl Pts',(2.11324386204848,-1.07676699050575,12.078662965112));
#93688=CARTESIAN_POINT('Ctrl Pts',(2.11915984456469,-1.06509125500273,12.0795422396565));
#93689=CARTESIAN_POINT('Ctrl Pts',(2.12262036283622,-1.05817797547843,12.0800594809004));
#93690=CARTESIAN_POINT('Ctrl Pts',(2.13495283817513,-1.03323673545039,12.081913847832));
#93691=CARTESIAN_POINT('Ctrl Pts',(2.143629734571,-1.01511250628012,12.0832394708479));
#93692=CARTESIAN_POINT('Ctrl Pts',(2.16465192985967,-0.969729533079284,
12.0865100515522));
#93693=CARTESIAN_POINT('Ctrl Pts',(2.17671398905196,-0.942342683477747,
12.0884405395596));
#93694=CARTESIAN_POINT('Ctrl Pts',(2.22599369737009,-0.824454177647528,
12.0965980069319));
#93695=CARTESIAN_POINT('Ctrl Pts',(2.25811241954266,-0.731918091040898,
12.1026251091618));
#93696=CARTESIAN_POINT('Ctrl Pts',(2.3043770643698,-0.566173328804962,12.113181562417));
#93697=CARTESIAN_POINT('Ctrl Pts',(2.32096374930366,-0.493794461356115,
12.1177144400559));
#93698=CARTESIAN_POINT('Ctrl Pts',(2.35597017178445,-0.299598544768957,
12.1298964545494));
#93699=CARTESIAN_POINT('Ctrl Pts',(2.36834145458165,-0.176938656559848,
12.1376211682771));
#93700=CARTESIAN_POINT('Ctrl Pts',(2.37156465605216,-0.035101155465809,
12.1468849867973));
#93701=CARTESIAN_POINT('Ctrl Pts',(2.37176828342757,-0.0163151867064924,
12.1481183089271));
#93702=CARTESIAN_POINT('Ctrl Pts',(2.37173641006333,0.0142806083841101,
12.1501382294368));
#93703=CARTESIAN_POINT('Ctrl Pts',(2.37163589921045,0.0260899909288855,
12.150920611989));
#93704=CARTESIAN_POINT('Ctrl Pts',(2.37129878920259,0.0471844971881024,
12.1523232393106));
#93705=CARTESIAN_POINT('Ctrl Pts',(2.37109583571387,0.0564699751180214,
12.1529424188753));
#93706=CARTESIAN_POINT('Ctrl Pts',(2.3705508428335,0.0761203660757453,12.1542566025492));
#93707=CARTESIAN_POINT('Ctrl Pts',(2.37019535117976,0.0864846801857484,
12.1549520151703));
#93708=CARTESIAN_POINT('Ctrl Pts',(2.36906479111327,0.11414885080847,12.1568144126208));
#93709=CARTESIAN_POINT('Ctrl Pts',(2.36816821565367,0.131442836331636,12.1579851734868));
#93710=CARTESIAN_POINT('Ctrl Pts',(2.36281053925323,0.216714687991474,12.163791139602));
#93711=CARTESIAN_POINT('Ctrl Pts',(2.35561186015997,0.284482039724925,12.1685110432529));
#93712=CARTESIAN_POINT('Ctrl Pts',(2.32607193976808,0.481407029463875,12.1825474469187));
#93713=CARTESIAN_POINT('Ctrl Pts',(2.29593568101464,0.60912673094418,12.1920733039751));
#93714=CARTESIAN_POINT('Ctrl Pts',(2.21425895627556,0.860206724232895,12.2113588759056));
#93715=CARTESIAN_POINT('Ctrl Pts',(2.16252631554485,0.98304904004922,12.2210839994846));
#93716=CARTESIAN_POINT('Ctrl Pts',(2.0918434375424,1.11792574540072,12.2316790887953));
#93717=CARTESIAN_POINT('Ctrl Pts',(2.08272168500248,1.13482923011275,12.2330050654514));
#93718=CARTESIAN_POINT('Ctrl Pts',(2.06960026308547,1.15845323550954,12.2348536640962));
#93719=CARTESIAN_POINT('Ctrl Pts',(2.06577146885511,1.16526708984569,12.2353863130099));
#93720=CARTESIAN_POINT('Ctrl Pts',(2.05927930157816,1.17668820744282,12.236278047779));
#93721=CARTESIAN_POINT('Ctrl Pts',(2.05663400446042,1.18130561374802,12.2366382679579));
#93722=CARTESIAN_POINT('Ctrl Pts',(2.05120668336528,1.19070559576255,12.237370928447));
#93723=CARTESIAN_POINT('Ctrl Pts',(2.0484234304241,1.19548740058673,12.2377432864134));
#93724=CARTESIAN_POINT('Ctrl Pts',(2.04129101825791,1.20764329658035,12.238689087837));
#93725=CARTESIAN_POINT('Ctrl Pts',(2.03691857258858,1.21500373962633,12.2392610442586));
#93726=CARTESIAN_POINT('Ctrl Pts',(2.01899799476063,1.24480205475699,12.2415742854662));
#93727=CARTESIAN_POINT('Ctrl Pts',(2.00511759058134,1.26703932402075,12.2432952630239));
#93728=CARTESIAN_POINT('Ctrl Pts',(1.96749549299831,1.32514501049946,12.2477907577836));
#93729=CARTESIAN_POINT('Ctrl Pts',(1.94314113353665,1.36060678087692,12.2505329575978));
#93730=CARTESIAN_POINT('Ctrl Pts',(1.79173811225853,1.56869640990903,12.2667407956411));
#93731=CARTESIAN_POINT('Ctrl Pts',(1.64273217358128,1.72411594418627,12.279431850364));
#93732=CARTESIAN_POINT('Ctrl Pts',(1.42367214432899,1.89805920507518,12.2971177079821));
#93733=CARTESIAN_POINT('Ctrl Pts',(1.37082497087268,1.93657140220284,12.3013142259393));
#93734=CARTESIAN_POINT('Ctrl Pts',(1.301607315422,1.98275949601139,12.3067645800443));
#93735=CARTESIAN_POINT('Ctrl Pts',(1.28664519333607,1.99250117694115,12.3079400237889));
#93736=CARTESIAN_POINT('Ctrl Pts',(1.26272136039388,2.00769590129888,12.3098159814015));
#93737=CARTESIAN_POINT('Ctrl Pts',(1.25383079439422,2.01326014193278,12.310512360691));
#93738=CARTESIAN_POINT('Ctrl Pts',(1.23780365927248,2.02314353045753,12.3117665132733));
#93739=CARTESIAN_POINT('Ctrl Pts',(1.23068061410725,2.02748436904839,12.3123234765885));
#93740=CARTESIAN_POINT('Ctrl Pts',(1.2139560950548,2.03755581241342,12.313630282861));
#93741=CARTESIAN_POINT('Ctrl Pts',(1.20433676778924,2.04325623251864,12.3143812114017));
#93742=CARTESIAN_POINT('Ctrl Pts',(1.17646210309063,2.05950955284682,12.3165554504598));
#93743=CARTESIAN_POINT('Ctrl Pts',(1.15810627582052,2.06988706987253,12.3179850346368));
#93744=CARTESIAN_POINT('Ctrl Pts',(0.984458652182627,2.16502635445306,12.3314924124387));
#93745=CARTESIAN_POINT('Ctrl Pts',(0.820310167817592,2.23238986534783,12.3442011988481));
#93746=CARTESIAN_POINT('Ctrl Pts',(0.506586040439996,2.32182723903128,12.3680112371111));
#93747=CARTESIAN_POINT('Ctrl Pts',(0.359373580767939,2.34912108670558,12.3789848293889));
#93748=CARTESIAN_POINT('Ctrl Pts',(0.191913245509808,2.36404692431366,12.3906763078027));
#93749=CARTESIAN_POINT('Ctrl Pts',(0.17324597908839,2.36548820330306,12.391968309503));
#93750=CARTESIAN_POINT('Ctrl Pts',(0.147609761539131,2.36716243061672,12.3937254366186));
#93751=CARTESIAN_POINT('Ctrl Pts',(0.140654558942902,2.3675858828726,12.3942004156932));
#93752=CARTESIAN_POINT('Ctrl Pts',(0.128761289452412,2.36825738392118,12.3950095395531));
#93753=CARTESIAN_POINT('Ctrl Pts',(0.123824180457617,2.3685206521464,12.3953445140816));
#93754=CARTESIAN_POINT('Ctrl Pts',(0.113571682611726,2.36903521521545,12.3960381953154));
#93755=CARTESIAN_POINT('Ctrl Pts',(0.108256239259344,2.36928406176334,12.3963967512297));
#93756=CARTESIAN_POINT('Ctrl Pts',(0.0954096551299932,2.36984216198566,
12.3972607907708));
#93757=CARTESIAN_POINT('Ctrl Pts',(0.0878777035675075,2.37013341146655,
12.3977652762332));
#93758=CARTESIAN_POINT('Ctrl Pts',(0.0615077822137425,2.3710272203427,12.3995245668751));
#93759=CARTESIAN_POINT('Ctrl Pts',(0.0426635241664532,2.37144115803878,
12.4007693653004));
#93760=CARTESIAN_POINT('Ctrl Pts',(-0.0736162715846883,2.37260882471755,
12.4083850094455));
#93761=CARTESIAN_POINT('Ctrl Pts',(-0.171028244247414,2.3675822971823,12.4144832196951));
#93762=CARTESIAN_POINT('Ctrl Pts',(-0.38699248975838,2.34303426534386,12.4279052284509));
#93763=CARTESIAN_POINT('Ctrl Pts',(-0.504920945193207,2.32048010060413,
12.4351737066231));
#93764=CARTESIAN_POINT('Ctrl Pts',(-0.726984499523905,2.26027262403236,
12.449434223003));
#93765=CARTESIAN_POINT('Ctrl Pts',(-0.831178292872454,2.22406758929908,
12.4563830462601));
#93766=CARTESIAN_POINT('Ctrl Pts',(-0.949403136286887,2.17351579106401,
12.4647821621643));
#93767=CARTESIAN_POINT('Ctrl Pts',(-0.966250752038867,2.16607863705785,
12.4659915030737));
#93768=CARTESIAN_POINT('Ctrl Pts',(-0.993655430551495,2.15359787018783,
12.4679799277809));
#93769=CARTESIAN_POINT('Ctrl Pts',(-1.0042650113724,2.14867091006672,12.4687550148228));
#93770=CARTESIAN_POINT('Ctrl Pts',(-1.02322153107276,2.13969666203909,12.4701495962316));
#93771=CARTESIAN_POINT('Ctrl Pts',(-1.03158204922485,2.13567848205318,12.4707680731842));
#93772=CARTESIAN_POINT('Ctrl Pts',(-1.04009433183799,2.13152571684589,12.4714013268687));
#93773=CARTESIAN_POINT('Ctrl Pts',(-1.04026997319318,2.13144000233868,12.4714143948922));
#93774=CARTESIAN_POINT('Ctrl Pts',(-1.04060645738165,2.13127574363226,12.4714394328693));
#93775=CARTESIAN_POINT('Ctrl Pts',(-1.0407673019214,2.13119720293333,12.4714514027003));
#93776=CARTESIAN_POINT('Ctrl Pts',(-1.04107545160036,2.13104668964666,12.4714743372676));
#93777=CARTESIAN_POINT('Ctrl Pts',(-1.04122275817543,2.13097471998999,12.4714853019015));
#93778=CARTESIAN_POINT('Ctrl Pts',(-1.04150498435649,2.13083679633468,12.4715063112451));
#93779=CARTESIAN_POINT('Ctrl Pts',(-1.04163990517566,2.13077084478807,12.4715163558697));
#93780=CARTESIAN_POINT('Ctrl Pts',(-1.0418984140125,2.13064445093627,12.4715356031645));
#93781=CARTESIAN_POINT('Ctrl Pts',(-1.04202200304191,2.13058401068904,12.4715448057629));
#93782=CARTESIAN_POINT('Ctrl Pts',(-1.0422588121497,2.13046817551535,12.4715624403462));
#93783=CARTESIAN_POINT('Ctrl Pts',(-1.0423720330766,2.13041278231406,12.4715708722709));
#93784=CARTESIAN_POINT('Ctrl Pts',(-1.04258898701066,2.13030661642931,12.4715870307606));
#93785=CARTESIAN_POINT('Ctrl Pts',(-1.04269272073395,2.13025584519016,12.4715947572753));
#93786=CARTESIAN_POINT('Ctrl Pts',(-1.04289150550433,2.13015853434611,12.4716095646214));
#93787=CARTESIAN_POINT('Ctrl Pts',(-1.04298655714295,2.13011199595696,12.4716166454099));
#93788=CARTESIAN_POINT('Ctrl Pts',(-1.04316871362991,2.1300227949041,12.4716302158695));
#93789=CARTESIAN_POINT('Ctrl Pts',(-1.04325581898201,2.12998013325653,12.4716367055054));
#93790=CARTESIAN_POINT('Ctrl Pts',(-1.04342275544403,2.12989835997503,12.4716491435545));
#93791=CARTESIAN_POINT('Ctrl Pts',(-1.04350258697463,2.12985924919465,12.471655091938));
#93792=CARTESIAN_POINT('Ctrl Pts',(-1.04365559050866,2.12978427957857,12.4716664931076));
#93793=CARTESIAN_POINT('Ctrl Pts',(-1.0437287628526,2.12974842146536,12.4716719458679));
#93794=CARTESIAN_POINT('Ctrl Pts',(-1.04386900990307,2.129679684423,12.4716823975132));
#93795=CARTESIAN_POINT('Ctrl Pts',(-1.04393608489663,2.12964680609972,12.4716873963766));
#93796=CARTESIAN_POINT('Ctrl Pts',(-1.04410194566876,2.12956549597682,12.4716997579575));
#93797=CARTESIAN_POINT('Ctrl Pts',(-1.04420072964193,2.12951706046688,12.4717071208057));
#93798=CARTESIAN_POINT('Ctrl Pts',(-1.04439642669855,2.12942108988594,12.4717217080304));
#93799=CARTESIAN_POINT('Ctrl Pts',(-1.04449333991292,2.12937355506949,12.4717289323984));
#93800=CARTESIAN_POINT('Ctrl Pts',(-1.04468533924511,2.12927936534509,12.4717432458725));
#93801=CARTESIAN_POINT('Ctrl Pts',(-1.04478042547185,2.1292327106892,12.4717503349692));
#93802=CARTESIAN_POINT('Ctrl Pts',(-1.04496881345674,2.12914026128041,12.4717643810266));
#93803=CARTESIAN_POINT('Ctrl Pts',(-1.04506211533331,2.12909446676221,12.4717713379793));
#93804=CARTESIAN_POINT('Ctrl Pts',(-1.04524697613467,2.12900371812387,12.471785122794));
#93805=CARTESIAN_POINT('Ctrl Pts',(-1.04533853518691,2.12895876422189,12.4717919506493));
#93806=CARTESIAN_POINT('Ctrl Pts',(-1.05531578320218,2.1240593101988,12.4725360325113));
#93807=CARTESIAN_POINT('Ctrl Pts',(-1.06516739419824,2.11913609066062,12.4732756811296));
#93808=CARTESIAN_POINT('Ctrl Pts',(-1.09334605887655,2.10480801627165,12.4754057344253));
#93809=CARTESIAN_POINT('Ctrl Pts',(-1.11158496277867,2.09523297358137,12.4768020883032));
#93810=CARTESIAN_POINT('Ctrl Pts',(-1.1525208588623,2.07305754060438,12.4799771116146));
#93811=CARTESIAN_POINT('Ctrl Pts',(-1.17514002949346,2.06031980901287,12.4817605032576));
#93812=CARTESIAN_POINT('Ctrl Pts',(-1.24749779103941,2.01799317851041,12.4875614169866));
#93813=CARTESIAN_POINT('Ctrl Pts',(-1.29636070971872,1.98695625979924,12.4916284047477));
#93814=CARTESIAN_POINT('Ctrl Pts',(-1.44229871816888,1.88658298241549,12.5042373231318));
#93815=CARTESIAN_POINT('Ctrl Pts',(-1.53531590764749,1.81169022638074,12.512940913135));
#93816=CARTESIAN_POINT('Ctrl Pts',(-1.71190293098036,1.64610892557766,12.530620566465));
#93817=CARTESIAN_POINT('Ctrl Pts',(-1.79485426386195,1.55524620907425,12.5395695978527));
#93818=CARTESIAN_POINT('Ctrl Pts',(-1.88222654201364,1.44318789416437,12.5494566685689));
#93819=CARTESIAN_POINT('Ctrl Pts',(-1.89386948253923,1.42787481803066,12.5507846769232));
#93820=CARTESIAN_POINT('Ctrl Pts',(-1.90998256562061,1.4061386213042,12.5526356078951));
#93821=CARTESIAN_POINT('Ctrl Pts',(-1.91460882232325,1.39983294902466,12.5531685903577));
#93822=CARTESIAN_POINT('Ctrl Pts',(-1.92233097592744,1.38919761321403,12.5540607230377));
#93823=CARTESIAN_POINT('Ctrl Pts',(-1.9254436107507,1.38488024511726,12.5544210097842));
#93824=CARTESIAN_POINT('Ctrl Pts',(-1.93176148022677,1.37605459290164,12.5551536499277));
#93825=CARTESIAN_POINT('Ctrl Pts',(-1.93496551799876,1.37154551688877,12.5555259218375));
#93826=CARTESIAN_POINT('Ctrl Pts',(-1.94308469893013,1.36003422860753,12.5564712385453));
#93827=CARTESIAN_POINT('Ctrl Pts',(-1.94797783835804,1.35301648072788,12.5570427993218));
#93828=CARTESIAN_POINT('Ctrl Pts',(-1.96767951567693,1.324431875986,12.5593523825381));
#93829=CARTESIAN_POINT('Ctrl Pts',(-1.98216939720738,1.30264618866939,12.5610701785135));
#93830=CARTESIAN_POINT('Ctrl Pts',(-2.01945780458749,1.24451928008548,12.565555326491));
#93831=CARTESIAN_POINT('Ctrl Pts',(-2.041636772729,1.20779046664347,12.568290545376));
#93832=CARTESIAN_POINT('Ctrl Pts',(-2.1596350224321,0.999834582011131,12.5833511462278));
#93833=CARTESIAN_POINT('Ctrl Pts',(-2.23491679923123,0.817831754420744,
12.5950212159477));
#93834=CARTESIAN_POINT('Ctrl Pts',(-2.30329808334263,0.569062273779928,
12.6111996525701));
#93835=CARTESIAN_POINT('Ctrl Pts',(-2.31733639411244,0.508886068116333,
12.6151234148213));
#93836=CARTESIAN_POINT('Ctrl Pts',(-2.33487580045077,0.417751880656847,
12.6211265200322));
#93837=CARTESIAN_POINT('Ctrl Pts',(-2.34014306905024,0.387158762642001,
12.6231516827518));
#93838=CARTESIAN_POINT('Ctrl Pts',(-2.34662453405432,0.344524884550173,
12.6259915670192));
#93839=CARTESIAN_POINT('Ctrl Pts',(-2.34834947241183,0.332564048314625,
12.6267902035345));
#93840=CARTESIAN_POINT('Ctrl Pts',(-2.35116892690733,0.311896982424793,
12.6281736951931));
#93841=CARTESIAN_POINT('Ctrl Pts',(-2.35230668444913,0.303196816041569,
12.6287571777211));
#93842=CARTESIAN_POINT('Ctrl Pts',(-2.35449624798838,0.285699110753148,
12.6299329291525));
#93843=CARTESIAN_POINT('Ctrl Pts',(-2.35554708435261,0.27690159514424,12.6305252185997));
#93844=CARTESIAN_POINT('Ctrl Pts',(-2.35758279689081,0.259007964596773,
12.6317323104543));
#93845=CARTESIAN_POINT('Ctrl Pts',(-2.35856438140266,0.249911633614706,
12.6323472061039));
#93846=CARTESIAN_POINT('Ctrl Pts',(-2.36070927484612,0.228895635389493,
12.6337708608584));
#93847=CARTESIAN_POINT('Ctrl Pts',(-2.36183497138468,0.216972465989632,
12.6345807877068));
#93848=CARTESIAN_POINT('Ctrl Pts',(-2.36379441443448,0.194392108121133,
12.6361190171284));
#93849=CARTESIAN_POINT('Ctrl Pts',(-2.36464649384007,0.183736959088881,
12.6368467111825));
#93850=CARTESIAN_POINT('Ctrl Pts',(-2.36542649456986,0.173076749700613,
12.6375766332401));
#93851=CARTESIAN_POINT('Origin',(0.,0.,-1.84858989190503));
#93852=CARTESIAN_POINT('',(-2.36542648366643,0.173076898716907,13.8355365560746));
#93853=CARTESIAN_POINT('',(-2.3654265016339,0.173076653156924,13.6406850658798));
#93854=CARTESIAN_POINT('',(-2.36542649454111,0.173076750093529,-1.84858989190503));
#93855=CARTESIAN_POINT('Ctrl Pts',(-2.36542648366643,0.173076898716907,
13.8355365560746));
#93856=CARTESIAN_POINT('Ctrl Pts',(-2.36039328004673,0.24186524209487,13.83056564983));
#93857=CARTESIAN_POINT('Ctrl Pts',(-2.35235946872098,0.310433940184986,
13.825661792469));
#93858=CARTESIAN_POINT('Ctrl Pts',(-2.33989547454688,0.387516525628758,
13.8202743280973));
#93859=CARTESIAN_POINT('Ctrl Pts',(-2.33840044556258,0.396438207113654,
13.8196527003806));
#93860=CARTESIAN_POINT('Ctrl Pts',(-2.33583000553576,0.411256820455127,
13.8186236458865));
#93861=CARTESIAN_POINT('Ctrl Pts',(-2.33478323446111,0.417158527634897,
13.8182147228627));
#93862=CARTESIAN_POINT('Ctrl Pts',(-2.33284797204356,0.427834055557162,
13.8174767548542));
#93863=CARTESIAN_POINT('Ctrl Pts',(-2.33196717621284,0.432609211541442,
13.8171472892113));
#93864=CARTESIAN_POINT('Ctrl Pts',(-2.33012887926652,0.442406608578485,
13.8164726446466));
#93865=CARTESIAN_POINT('Ctrl Pts',(-2.32916981436925,0.44742840555511,13.8161275757743));
#93866=CARTESIAN_POINT('Ctrl Pts',(-2.32696445708651,0.458776692019071,
13.815349411315));
#93867=CARTESIAN_POINT('Ctrl Pts',(-2.32570860150079,0.465101215955899,
13.8149168647948));
#93868=CARTESIAN_POINT('Ctrl Pts',(-2.32191238044717,0.483819188576863,
13.8136398517279));
#93869=CARTESIAN_POINT('Ctrl Pts',(-2.31929858034927,0.496197765470347,
13.8127994281688));
#93870=CARTESIAN_POINT('Ctrl Pts',(-2.29357002253575,0.613397264204295,
13.8048760668163));
#93871=CARTESIAN_POINT('Ctrl Pts',(-2.26346006946904,0.716571441766442,
13.7981546891627));
#93872=CARTESIAN_POINT('Ctrl Pts',(-2.19789797818924,0.895159504927388,
13.7864117145909));
#93873=CARTESIAN_POINT('Ctrl Pts',(-2.16527958724309,0.971406573064843,
13.7813605706524));
#93874=CARTESIAN_POINT('Ctrl Pts',(-2.09042789357284,1.12376934530554,13.7709323698037));
#93875=CARTESIAN_POINT('Ctrl Pts',(-2.04786542696937,1.19957989734769,13.765558792318));
#93876=CARTESIAN_POINT('Ctrl Pts',(-1.96600263086737,1.32828585809461,13.7559094906364));
#93877=CARTESIAN_POINT('Ctrl Pts',(-1.92847971265286,1.38219912244799,13.7516910781001));
#93878=CARTESIAN_POINT('Ctrl Pts',(-1.87848018240435,1.44803307300398,13.7462716803244));
#93879=CARTESIAN_POINT('Ctrl Pts',(-1.86804381456948,1.46147181221751,13.7451507323851));
#93880=CARTESIAN_POINT('Ctrl Pts',(-1.85111476396641,1.48279346237557,13.7433479380973));
#93881=CARTESIAN_POINT('Ctrl Pts',(-1.84471406296757,1.49074891975858,13.7426697668066));
#93882=CARTESIAN_POINT('Ctrl Pts',(-1.83247638555565,1.50575967623371,13.7413794960421));
#93883=CARTESIAN_POINT('Ctrl Pts',(-1.82664951626461,1.51282300579344,13.7407678127598));
#93884=CARTESIAN_POINT('Ctrl Pts',(-1.8133114434909,1.5288020070386,13.7393735454297));
#93885=CARTESIAN_POINT('Ctrl Pts',(-1.80577516040635,1.53769633849624,13.7385899438308));
#93886=CARTESIAN_POINT('Ctrl Pts',(-1.78606470464423,1.56061391397602,13.7365510478609));
#93887=CARTESIAN_POINT('Ctrl Pts',(-1.77379105415041,1.57455015149746,13.735291656171));
#93888=CARTESIAN_POINT('Ctrl Pts',(-1.68017385631382,1.67836488813536,13.7257595597905));
#93889=CARTESIAN_POINT('Ctrl Pts',(-1.59222375240875,1.76201811243754,13.7172032883976));
#93890=CARTESIAN_POINT('Ctrl Pts',(-1.47574810763962,1.8569357616957,13.7063596416695));
#93891=CARTESIAN_POINT('Ctrl Pts',(-1.45288097843942,1.87488124862787,13.7042527262708));
#93892=CARTESIAN_POINT('Ctrl Pts',(-1.29374400778341,1.99510762089445,13.6897512397618));
#93893=CARTESIAN_POINT('Ctrl Pts',(-1.14712143387038,2.08286977202426,13.6771410648638));
#93894=CARTESIAN_POINT('Ctrl Pts',(-0.970580455281716,2.16419646848831,
13.6635539405041));
#93895=CARTESIAN_POINT('Ctrl Pts',(-0.948654688567413,2.17389677047183,
13.6618935112987));
#93896=CARTESIAN_POINT('Ctrl Pts',(-0.919180933683756,2.18640553428428,
13.6597008988304));
#93897=CARTESIAN_POINT('Ctrl Pts',(-0.911761231965697,2.18951003876113,
13.6591522333199));
#93898=CARTESIAN_POINT('Ctrl Pts',(-0.899274624711374,2.19466012538113,
13.6582345897609));
#93899=CARTESIAN_POINT('Ctrl Pts',(-0.894216253192675,2.19672602084789,
13.6578644133508));
#93900=CARTESIAN_POINT('Ctrl Pts',(-0.884296465316073,2.2007374311934,13.6571415970444));
#93901=CARTESIAN_POINT('Ctrl Pts',(-0.879435687226764,2.20268435153908,
13.6567888777625));
#93902=CARTESIAN_POINT('Ctrl Pts',(-0.867452894753732,2.20743791237579,
13.6559228677528));
#93903=CARTESIAN_POINT('Ctrl Pts',(-0.860323581052744,2.21022623312512,
13.6554106697709));
#93904=CARTESIAN_POINT('Ctrl Pts',(-0.835800607028149,2.2196806924828,13.653658866025));
#93905=CARTESIAN_POINT('Ctrl Pts',(-0.8183414399862,2.22617662650169,13.6524289190563));
#93906=CARTESIAN_POINT('Ctrl Pts',(-0.659740015757757,2.28306846175177,
13.641395595291));
#93907=CARTESIAN_POINT('Ctrl Pts',(-0.51417260351606,2.32019359606721,13.6322508311655));
#93908=CARTESIAN_POINT('Ctrl Pts',(-0.246378246363884,2.36202629424293,
13.6156442953703));
#93909=CARTESIAN_POINT('Ctrl Pts',(-0.125452686478198,2.37152461733269,
13.6082215094878));
#93910=CARTESIAN_POINT('Ctrl Pts',(0.0374522253702291,2.37182243152562,
13.5979017024351));
#93911=CARTESIAN_POINT('Ctrl Pts',(0.0792330355859025,2.37079440863415,
13.5952278989353));
#93912=CARTESIAN_POINT('Ctrl Pts',(0.151013878122831,2.36712869859553,13.5905727258431));
#93913=CARTESIAN_POINT('Ctrl Pts',(0.1810315572974,2.36502239065536,13.5886074884343));
#93914=CARTESIAN_POINT('Ctrl Pts',(0.223724930469734,2.36120910433829,13.5857824208118));
#93915=CARTESIAN_POINT('Ctrl Pts',(0.236440285312464,2.35996975819975,13.5849372415586));
#93916=CARTESIAN_POINT('Ctrl Pts',(0.258415757523683,2.35764846159353,13.5834697187558));
#93917=CARTESIAN_POINT('Ctrl Pts',(0.267680745052979,2.35661451804419,13.5828488981799));
#93918=CARTESIAN_POINT('Ctrl Pts',(0.285460491560588,2.35452415254588,13.5816533810088));
#93919=CARTESIAN_POINT('Ctrl Pts',(0.293976101758224,2.35347609407967,13.5810789577061));
#93920=CARTESIAN_POINT('Ctrl Pts',(0.314030930789906,2.35089730365247,13.5797217483405));
#93921=CARTESIAN_POINT('Ctrl Pts',(0.325564850883407,2.34932779263571,13.5789377481315));
#93922=CARTESIAN_POINT('Ctrl Pts',(0.365750351163728,2.34355782812522,13.5761939014556));
#93923=CARTESIAN_POINT('Ctrl Pts',(0.394335183571449,2.33891775109844,13.5742202535806));
#93924=CARTESIAN_POINT('Ctrl Pts',(0.58028056685533,2.30522840748879,13.5612328580375));
#93925=CARTESIAN_POINT('Ctrl Pts',(0.734414311209268,2.26084530820466,13.549727132066));
#93926=CARTESIAN_POINT('Ctrl Pts',(0.991601984140914,2.15769446205777,13.5295072282718));
#93927=CARTESIAN_POINT('Ctrl Pts',(1.09694831991385,2.10609276666328,13.5209093982515));
#93928=CARTESIAN_POINT('Ctrl Pts',(1.2265289986424,2.03024955620763,13.5102075939812));
#93929=CARTESIAN_POINT('Ctrl Pts',(1.25465458333209,2.01299000431196,13.5078773429947));
#93930=CARTESIAN_POINT('Ctrl Pts',(1.30054086387953,1.98349589023642,13.5040740432057));
#93931=CARTESIAN_POINT('Ctrl Pts',(1.31851057437324,1.97159641748497,13.5025842252221));
#93932=CARTESIAN_POINT('Ctrl Pts',(1.34282491584763,1.95501441714933,13.5005704948672));
#93933=CARTESIAN_POINT('Ctrl Pts',(1.34931141997606,1.95054321210731,13.5000334865263));
#93934=CARTESIAN_POINT('Ctrl Pts',(1.36015212862049,1.94299065868512,13.4991365127062));
#93935=CARTESIAN_POINT('Ctrl Pts',(1.36451838486048,1.93992682642096,13.49877538396));
#93936=CARTESIAN_POINT('Ctrl Pts',(1.37277613083524,1.93409063528804,13.4980927183124));
#93937=CARTESIAN_POINT('Ctrl Pts',(1.3766696283295,1.93132121263565,13.4977709796384));
#93938=CARTESIAN_POINT('Ctrl Pts',(1.3868488862342,1.9240343412104,13.4969300975687));
#93939=CARTESIAN_POINT('Ctrl Pts',(1.39312101369233,1.91949780537734,13.4964122541083));
#93940=CARTESIAN_POINT('Ctrl Pts',(1.41482491354248,1.90363727911342,13.4946208680794));
#93941=CARTESIAN_POINT('Ctrl Pts',(1.4301422333882,1.89215688475472,13.4933575778346));
#93942=CARTESIAN_POINT('Ctrl Pts',(1.54664703806597,1.80261293735058,13.4837418965744));
#93943=CARTESIAN_POINT('Ctrl Pts',(1.64152889021988,1.716660232144,13.475863433109));
#93944=CARTESIAN_POINT('Ctrl Pts',(1.8072308338674,1.54018384037335,13.461013656878));
#93945=CARTESIAN_POINT('Ctrl Pts',(1.87930914125581,1.45135981633843,13.454053060609));
#93946=CARTESIAN_POINT('Ctrl Pts',(1.97808110277971,1.30988281367792,13.4432604213924));
#93947=CARTESIAN_POINT('Ctrl Pts',(2.00968241662254,1.26086226877601,13.4395706140131));
#93948=CARTESIAN_POINT('Ctrl Pts',(2.05918342507402,1.177479062386,13.4333307939119));
#93949=CARTESIAN_POINT('Ctrl Pts',(2.07810583053971,1.14375224578573,13.4308165191582));
#93950=CARTESIAN_POINT('Ctrl Pts',(2.10278489984987,1.09712905939844,13.4273460676678));
#93951=CARTESIAN_POINT('Ctrl Pts',(2.10926409742982,1.08462042250214,13.4264154909385));
#93952=CARTESIAN_POINT('Ctrl Pts',(2.11996004870427,1.06351265349513,13.4248456889899));
#93953=CARTESIAN_POINT('Ctrl Pts',(2.1242369000706,1.05494424497924,13.4242085884163));
#93954=CARTESIAN_POINT('Ctrl Pts',(2.13257380404312,1.03798550648644,13.4229477842765));
#93955=CARTESIAN_POINT('Ctrl Pts',(2.13663652184993,1.02959667373577,13.4223241878986));
#93956=CARTESIAN_POINT('Ctrl Pts',(2.14547258275653,1.01107414830746,13.4209473451508));
#93957=CARTESIAN_POINT('Ctrl Pts',(2.15022377211647,1.00093019689202,13.4201933473122));
#93958=CARTESIAN_POINT('Ctrl Pts',(2.16667049002365,0.96515833941974,13.4175343046081));
#93959=CARTESIAN_POINT('Ctrl Pts',(2.17798072385046,0.939356949997527,13.4156161355481));
#93960=CARTESIAN_POINT('Ctrl Pts',(2.26258656372062,0.736602921597457,13.4005343066456));
#93961=CARTESIAN_POINT('Ctrl Pts',(2.31464818703371,0.551594475501066,13.3866370705455));
#93962=CARTESIAN_POINT('Ctrl Pts',(2.34800823595653,0.335824232937742,13.3706890154025));
#93963=CARTESIAN_POINT('Ctrl Pts',(2.35166345550595,0.309191857148216,13.3687266205685));
#93964=CARTESIAN_POINT('Ctrl Pts',(2.36648996811652,0.185602206031561,13.3596598783068));
#93965=CARTESIAN_POINT('Ctrl Pts',(2.3721238684653,0.0880651570359345,13.3526140453319));
#93966=CARTESIAN_POINT('Ctrl Pts',(2.37165522313945,-0.0283108917064951,
13.3445241688066));
#93967=CARTESIAN_POINT('Ctrl Pts',(2.37135709480836,-0.0470700397291419,
13.3432300691523));
#93968=CARTESIAN_POINT('Ctrl Pts',(2.37062935403039,-0.0732815094306271,
13.3414375620916));
#93969=CARTESIAN_POINT('Ctrl Pts',(2.37038712809214,-0.0807377273862422,
13.3409294343541));
#93970=CARTESIAN_POINT('Ctrl Pts',(2.36991446201371,-0.0934402427160046,
13.340066947583));
#93971=CARTESIAN_POINT('Ctrl Pts',(2.36970177305517,-0.0986871072482835,
13.339711613109));
#93972=CARTESIAN_POINT('Ctrl Pts',(2.36925853960096,-0.108791941354843,
13.339029107453));
#93973=CARTESIAN_POINT('Ctrl Pts',(2.36903047824806,-0.113649937096084,
13.3387017940419));
#93974=CARTESIAN_POINT('Ctrl Pts',(2.36844624464178,-0.125327916391205,
13.3379168439044));
#93975=CARTESIAN_POINT('Ctrl Pts',(2.36807555327816,-0.132147180282065,
13.3374600107162));
#93976=CARTESIAN_POINT('Ctrl Pts',(2.36661142138493,-0.157092977580794,
13.3357941475678));
#93977=CARTESIAN_POINT('Ctrl Pts',(2.36533923369439,-0.17520896865986,13.3345946076372));
#93978=CARTESIAN_POINT('Ctrl Pts',(2.35084015901665,-0.35250918177748,13.3229393548876));
#93979=CARTESIAN_POINT('Ctrl Pts',(2.3217699103028,-0.510012011121038,13.3132362294613));
#93980=CARTESIAN_POINT('Ctrl Pts',(2.23004281438386,-0.824852486863105,
13.2931391911143));
#93981=CARTESIAN_POINT('Ctrl Pts',(2.16598237862899,-0.980806740607857,
13.282774641262));
#93982=CARTESIAN_POINT('Ctrl Pts',(2.07610837368012,-1.14690988412821,13.2704417206349));
#93983=CARTESIAN_POINT('Ctrl Pts',(2.06599943664818,-1.16502126345027,13.2690791965614));
#93984=CARTESIAN_POINT('Ctrl Pts',(2.05016104543447,-1.19254310258095,13.2669801551541));
#93985=CARTESIAN_POINT('Ctrl Pts',(2.04460122202787,-1.20205041477193,13.2662497508523));
#93986=CARTESIAN_POINT('Ctrl Pts',(2.03477590275371,-1.21858634427434,13.2649699110149));
#93987=CARTESIAN_POINT('Ctrl Pts',(2.03053966992972,-1.22563220371696,13.2644215489439));
#93988=CARTESIAN_POINT('Ctrl Pts',(2.02089170451218,-1.24149174293454,13.2631802962078));
#93989=CARTESIAN_POINT('Ctrl Pts',(2.01545881076356,-1.25029228797385,13.2624866359622));
#93990=CARTESIAN_POINT('Ctrl Pts',(2.0006176350015,-1.27398486087205,13.2606057640455));
#93991=CARTESIAN_POINT('Ctrl Pts',(1.99110087953804,-1.28880782331417,13.2594145553667));
#93992=CARTESIAN_POINT('Ctrl Pts',(1.94600431330749,-1.35735685484944,13.2538367794574));
#93993=CARTESIAN_POINT('Ctrl Pts',(1.90841258660702,-1.40971998305166,13.2493752408948));
#93994=CARTESIAN_POINT('Ctrl Pts',(1.73568300298879,-1.63073338083704,13.2296310212395));
#93995=CARTESIAN_POINT('Ctrl Pts',(1.57998933007677,-1.78199188103808,13.2135630328312));
#93996=CARTESIAN_POINT('Ctrl Pts',(1.37138139678238,-1.93555198726543,13.1949535309795));
#93997=CARTESIAN_POINT('Ctrl Pts',(1.33604961543301,-1.960107222092,13.1918929568441));
#93998=CARTESIAN_POINT('Ctrl Pts',(1.2782053044385,-1.99801714214975,13.1870490232091));
#93999=CARTESIAN_POINT('Ctrl Pts',(1.25610672041074,-2.01198343719811,13.1852361040396));
#94000=CARTESIAN_POINT('Ctrl Pts',(1.2265403199795,-2.02999230950436,13.1828644113082));
#94001=CARTESIAN_POINT('Ctrl Pts',(1.21927628106825,-2.03436360790525,13.1822859562581));
#94002=CARTESIAN_POINT('Ctrl Pts',(1.20729324094542,-2.04148743168327,13.1813388552885));
#94003=CARTESIAN_POINT('Ctrl Pts',(1.20258797026574,-2.04426272251901,13.1809687630233));
#94004=CARTESIAN_POINT('Ctrl Pts',(1.19335313459514,-2.04966674964374,13.1802459753584));
#94005=CARTESIAN_POINT('Ctrl Pts',(1.18882439710042,-2.05229677243919,13.1798932012966));
#94006=CARTESIAN_POINT('Ctrl Pts',(1.1776508183472,-2.05873633032665,13.1790268496123));
#94007=CARTESIAN_POINT('Ctrl Pts',(1.17099608640866,-2.06252876282544,13.1785143667254));
#94008=CARTESIAN_POINT('Ctrl Pts',(1.1480722880759,-2.07544598099605,13.1767605629602));
#94009=CARTESIAN_POINT('Ctrl Pts',(1.13171350431815,-2.08441133093501,13.1755289304902));
#94010=CARTESIAN_POINT('Ctrl Pts',(0.983055214052431,-2.16361661537799,
13.1644995247509));
#94011=CARTESIAN_POINT('Ctrl Pts',(0.844464836077715,-2.22137948812558,
13.1553594494784));
#94012=CARTESIAN_POINT('Ctrl Pts',(0.58558938442156,-2.30151329482222,13.1387558390886));
#94013=CARTESIAN_POINT('Ctrl Pts',(0.467278928116707,-2.32841699627352,
13.1313311560334));
#94014=CARTESIAN_POINT('Ctrl Pts',(0.306092334984067,-2.35228662032879,
13.1210089236276));
#94015=CARTESIAN_POINT('Ctrl Pts',(0.264595884242198,-2.35731490592322,
13.1183347149211));
#94016=CARTESIAN_POINT('Ctrl Pts',(0.193029779732385,-2.36407343133189,
13.1136788983949));
#94017=CARTESIAN_POINT('Ctrl Pts',(0.16301956448586,-2.36633221929618,13.111713428907));
#94018=CARTESIAN_POINT('Ctrl Pts',(0.120219438727262,-2.36873565030719,
13.1088880855567));
#94019=CARTESIAN_POINT('Ctrl Pts',(0.107457943977824,-2.36934887130852,
13.1080428666357));
#94020=CARTESIAN_POINT('Ctrl Pts',(0.0853771146285568,-2.37023115380912,
13.1065752970797));
#94021=CARTESIAN_POINT('Ctrl Pts',(0.0760599064882378,-2.3705484303326,
13.1059544696866));
#94022=CARTESIAN_POINT('Ctrl Pts',(0.0581648179826237,-2.37105219866113,
13.1047589550329));
#94023=CARTESIAN_POINT('Ctrl Pts',(0.049587305344609,-2.37124709185295,
13.1041845411506));
#94024=CARTESIAN_POINT('Ctrl Pts',(0.0293710595065186,-2.37159669547986,
13.1028273782122));
#94025=CARTESIAN_POINT('Ctrl Pts',(0.0177319593183965,-2.37171227477861,
13.1020434152136));
#94026=CARTESIAN_POINT('Ctrl Pts',(-0.0228617688647179,-2.37181655412525,
13.0992998250801));
#94027=CARTESIAN_POINT('Ctrl Pts',(-0.0518139514957971,-2.37136070888297,
13.0973263999324));
#94028=CARTESIAN_POINT('Ctrl Pts',(-0.241040516821711,-2.36491449632116,
13.0843140434364));
#94029=CARTESIAN_POINT('Ctrl Pts',(-0.400334955452189,-2.34321045976057,
13.0727806591625));
#94030=CARTESIAN_POINT('Ctrl Pts',(-0.669784856626021,-2.27820990407324,
13.052554386564));
#94031=CARTESIAN_POINT('Ctrl Pts',(-0.781201358754205,-2.24244933832728,
13.0439784405596));
#94032=CARTESIAN_POINT('Ctrl Pts',(-0.92007656222129,-2.18626230494038,
13.0333008313638));
#94033=CARTESIAN_POINT('Ctrl Pts',(-0.9503619175815,-2.17326855383347,13.030973767359));
#94034=CARTESIAN_POINT('Ctrl Pts',(-0.999972096075376,-2.15074809679995,
13.0271751001228));
#94035=CARTESIAN_POINT('Ctrl Pts',(-1.01945477092564,-2.1415820370905,13.0256867764275));
#94036=CARTESIAN_POINT('Ctrl Pts',(-1.04589023996994,-2.12870234749524,
13.0236747215502));
#94037=CARTESIAN_POINT('Ctrl Pts',(-1.05295260907856,-2.12521784432056,
13.0231379219405));
#94038=CARTESIAN_POINT('Ctrl Pts',(-1.06476858703089,-2.11931459725055,
13.022241199171));
#94039=CARTESIAN_POINT('Ctrl Pts',(-1.069531575646,-2.11691490535367,13.0218801141194));
#94040=CARTESIAN_POINT('Ctrl Pts',(-1.07854663896613,-2.11233473754071,
13.0211974580525));
#94041=CARTESIAN_POINT('Ctrl Pts',(-1.08280027203294,-2.11015745094376,
13.0208756856676));
#94042=CARTESIAN_POINT('Ctrl Pts',(-1.09392957073957,-2.10441823733817,
13.0200345812468));
#94043=CARTESIAN_POINT('Ctrl Pts',(-1.10079449670808,-2.10083542992669,
13.019516550485));
#94044=CARTESIAN_POINT('Ctrl Pts',(-1.12458202122282,-2.08827209810911,
13.0177238526742));
#94045=CARTESIAN_POINT('Ctrl Pts',(-1.14141381595901,-2.07911991884032,
13.0164594578887));
#94046=CARTESIAN_POINT('Ctrl Pts',(-1.26823101907485,-2.00815954686025,
13.0069499990694));
#94047=CARTESIAN_POINT('Ctrl Pts',(-1.37325339274456,-1.93785925955151,
12.9991664562669));
#94048=CARTESIAN_POINT('Ctrl Pts',(-1.56431801403496,-1.78659266026616,
12.9842144659192));
#94049=CARTESIAN_POINT('Ctrl Pts',(-1.65089020684405,-1.70691658922275,
12.9770593143163));
#94050=CARTESIAN_POINT('Ctrl Pts',(-1.77037226865347,-1.57932403804773,
12.9661180872572));
#94051=CARTESIAN_POINT('Ctrl Pts',(-1.8080130880724,-1.53608929902158,12.9624892104753));
#94052=CARTESIAN_POINT('Ctrl Pts',(-1.8680597955052,-1.46185100805962,12.9563429133728));
#94053=CARTESIAN_POINT('Ctrl Pts',(-1.89134874720401,-1.43159191742304,
12.9538598124634));
#94054=CARTESIAN_POINT('Ctrl Pts',(-1.9221760123903,-1.38947255175145,12.9504256706073));
#94055=CARTESIAN_POINT('Ctrl Pts',(-1.9303551883669,-1.37808687216407,12.949499525053));
#94056=CARTESIAN_POINT('Ctrl Pts',(-1.94394282141897,-1.35881411932749,
12.9479350902317));
#94057=CARTESIAN_POINT('Ctrl Pts',(-1.94940545477528,-1.350965533288,12.9472988930998));
#94058=CARTESIAN_POINT('Ctrl Pts',(-1.96010500023052,-1.33539265302934,
12.9460382262195));
#94059=CARTESIAN_POINT('Ctrl Pts',(-1.96534408426394,-1.3276700553339,12.9454138542165));
#94060=CARTESIAN_POINT('Ctrl Pts',(-1.9767954142291,-1.31057407375535,12.944033278357));
#94061=CARTESIAN_POINT('Ctrl Pts',(-1.98298681722395,-1.30118706865472,
12.9432763079086));
#94062=CARTESIAN_POINT('Ctrl Pts',(-2.00460351973117,-1.26790059181442,
12.9405955817588));
#94063=CARTESIAN_POINT('Ctrl Pts',(-2.01966486030204,-1.24376883345289,
12.9386584164834));
#94064=CARTESIAN_POINT('Ctrl Pts',(-2.13099442350199,-1.05803697931263,
12.9237898750362));
#94065=CARTESIAN_POINT('Ctrl Pts',(-2.20814630307436,-0.885800042265752,
12.91015439604));
#94066=CARTESIAN_POINT('Ctrl Pts',(-2.28862930786293,-0.627802748084554,
12.8904118233233));
#94067=CARTESIAN_POINT('Ctrl Pts',(-2.3090201925046,-0.54807610780382,12.8844110439632));
#94068=CARTESIAN_POINT('Ctrl Pts',(-2.33649802229436,-0.411393016004873,
12.8744296156882));
#94069=CARTESIAN_POINT('Ctrl Pts',(-2.34573737410859,-0.354943166158775,
12.8703943731318));
#94070=CARTESIAN_POINT('Ctrl Pts',(-2.35429878281118,-0.287392065166123,
12.8657096037321));
#94071=CARTESIAN_POINT('Ctrl Pts',(-2.35559519422827,-0.276565092461932,
12.8649631253587));
#94072=CARTESIAN_POINT('Ctrl Pts',(-2.35748886198653,-0.259769698963854,
12.86381233909));
#94073=CARTESIAN_POINT('Ctrl Pts',(-2.35813820516683,-0.253807482666157,
12.8634052226132));
#94074=CARTESIAN_POINT('Ctrl Pts',(-2.35929976534582,-0.242752702777633,
12.8626530498243));
#94075=CARTESIAN_POINT('Ctrl Pts',(-2.35981811096488,-0.237660980140859,
12.8623076673249));
#94076=CARTESIAN_POINT('Ctrl Pts',(-2.36096019249512,-0.226070029910925,
12.8615238080385));
#94077=CARTESIAN_POINT('Ctrl Pts',(-2.36157357650475,-0.219569884800047,
12.8610859154861));
#94078=CARTESIAN_POINT('Ctrl Pts',(-2.36310107688707,-0.202635318454724,
12.8599493010245));
#94079=CARTESIAN_POINT('Ctrl Pts',(-2.36397294002247,-0.192197088300605,
12.8592528659236));
#94080=CARTESIAN_POINT('Ctrl Pts',(-2.36938498223819,-0.121781455892595,
12.8545806993733));
#94081=CARTESIAN_POINT('Ctrl Pts',(-2.37171174752863,-0.0616500417224155,
12.8507175434041));
#94082=CARTESIAN_POINT('Ctrl Pts',(-2.37178614178588,0.056799813610108,
12.8432429961234));
#94083=CARTESIAN_POINT('Ctrl Pts',(-2.36967389599326,0.115027955686387,
12.8396328989325));
#94084=CARTESIAN_POINT('Ctrl Pts',(-2.36542647041237,0.173077079858942,
12.8360489723835));
#94085=CARTESIAN_POINT('',(-2.37174897232385,-0.00158322021055804,12.6497084150621));
#94086=CARTESIAN_POINT('Ctrl Pts',(-2.36542649456986,0.173076749700613,
12.6375766332401));
#94087=CARTESIAN_POINT('Ctrl Pts',(-2.36658602748831,0.157229503369983,
12.6386617202425));
#94088=CARTESIAN_POINT('Ctrl Pts',(-2.36758627251794,0.141371074232541,
12.6397517332812));
#94089=CARTESIAN_POINT('Ctrl Pts',(-2.37067010211813,0.083175043826123,
12.6437674062594));
#94090=CARTESIAN_POINT('Ctrl Pts',(-2.37177781513596,0.0407965685027263,
12.6467221209576));
#94091=CARTESIAN_POINT('Ctrl Pts',(-2.37174946956768,-0.00158622363318729,
12.6497077602747));
#94092=CARTESIAN_POINT('Ctrl Pts',(-2.37174947153371,-0.00158328125955357,
12.6497075530004));
#94093=CARTESIAN_POINT('Ctrl Pts',(-2.37160653311771,-0.215704499816572,
12.6647912319001));
#94094=CARTESIAN_POINT('Ctrl Pts',(-2.34246509598743,-0.428823103194869,
12.6807104451231));
#94095=CARTESIAN_POINT('Ctrl Pts',(-2.2736546331288,-0.676410862535811,
12.6991701563721));
#94096=CARTESIAN_POINT('Ctrl Pts',(-2.26105235453986,-0.717411845906221,
12.7022211463399));
#94097=CARTESIAN_POINT('Ctrl Pts',(-2.23898449953131,-0.782834982600065,
12.7070571680125));
#94098=CARTESIAN_POINT('Ctrl Pts',(-2.23021474331369,-0.807480366208175,
12.7088713744339));
#94099=CARTESIAN_POINT('Ctrl Pts',(-2.21803786776668,-0.839987652639569,
12.7112496634414));
#94100=CARTESIAN_POINT('Ctrl Pts',(-2.21499374392475,-0.84798228726436,
12.7118333755295));
#94101=CARTESIAN_POINT('Ctrl Pts',(-2.20991014190329,-0.861118936225222,
12.7127903557539));
#94102=CARTESIAN_POINT('Ctrl Pts',(-2.20789584492145,-0.866270510409055,
12.7131650872419));
#94103=CARTESIAN_POINT('Ctrl Pts',(-2.20390796817783,-0.87636525428476,
12.7138982417253));
#94104=CARTESIAN_POINT('Ctrl Pts',(-2.20193574563793,-0.881308892588369,
12.7142567383546));
#94105=CARTESIAN_POINT('Ctrl Pts',(-2.19702441069505,-0.893500402927079,
12.7151395732966));
#94106=CARTESIAN_POINT('Ctrl Pts',(-2.1940660232248,-0.900740540506177,
12.7156627626911));
#94107=CARTESIAN_POINT('Ctrl Pts',(-2.18370695453858,-0.925738681962946,
12.7174658277318));
#94108=CARTESIAN_POINT('Ctrl Pts',(-2.17612582538652,-0.943421762126264,
12.7187353858324));
#94109=CARTESIAN_POINT('Ctrl Pts',(-2.1186300402621,-1.07314951455895,12.7280196492916));
#94110=CARTESIAN_POINT('Ctrl Pts',(-2.06029871015184,-1.1812791592184,12.7355998405026));
#94111=CARTESIAN_POINT('Ctrl Pts',(-1.9376385713577,-1.371688989503,12.7495048894272));
#94112=CARTESIAN_POINT('Ctrl Pts',(-1.87575394168097,-1.4551702141512,12.7558286043168));
#94113=CARTESIAN_POINT('Ctrl Pts',(-1.76490856660018,-1.585830236816,12.766485120645));
#94114=CARTESIAN_POINT('Ctrl Pts',(-1.7190383557578,-1.63544056213426,12.7707353018693));
#94115=CARTESIAN_POINT('Ctrl Pts',(-1.6506335766004,-1.70336139418507,12.7769186595485));
#94116=CARTESIAN_POINT('Ctrl Pts',(-1.62978185650955,-1.72332302019158,
12.778784371085));
#94117=CARTESIAN_POINT('Ctrl Pts',(-1.59212183531959,-1.75808054917181,
12.7821251325903));
#94118=CARTESIAN_POINT('Ctrl Pts',(-1.57545833218542,-1.77302852294085,
12.7835936985877));
#94119=CARTESIAN_POINT('Ctrl Pts',(-1.5499884698018,-1.79523366506084,12.7858254879866));
#94120=CARTESIAN_POINT('Ctrl Pts',(-1.54133690593353,-1.80266710831129,
12.7865813862619));
#94121=CARTESIAN_POINT('Ctrl Pts',(-1.52583649139523,-1.81579193636671,
12.7879319902799));
#94122=CARTESIAN_POINT('Ctrl Pts',(-1.5190085266129,-1.82150774003464,12.7885256795905));
#94123=CARTESIAN_POINT('Ctrl Pts',(-1.50417176808201,-1.83378640103706,
12.7898131294515));
#94124=CARTESIAN_POINT('Ctrl Pts',(-1.49615188833904,-1.84033551116142,
12.7905074305846));
#94125=CARTESIAN_POINT('Ctrl Pts',(-1.47466246398457,-1.8576506702423,12.7923637023425));
#94126=CARTESIAN_POINT('Ctrl Pts',(-1.46111817089196,-1.86832252531532,
12.7935294055202));
#94127=CARTESIAN_POINT('Ctrl Pts',(-1.40034548057679,-1.91514169098847,
12.7987421215399));
#94128=CARTESIAN_POINT('Ctrl Pts',(-1.35188740520355,-1.94964984294688,
12.8028522795967));
#94129=CARTESIAN_POINT('Ctrl Pts',(-1.11759999595871,-2.10355510124951,
12.8225273307876));
#94130=CARTESIAN_POINT('Ctrl Pts',(-0.916988769309791,-2.19842589424856,
12.8389486691159));
#94131=CARTESIAN_POINT('Ctrl Pts',(-0.66479954454223,-2.2770862780313,12.8579320995649));
#94132=CARTESIAN_POINT('Ctrl Pts',(-0.623032761525838,-2.28886675115751,
12.8610198450748));
#94133=CARTESIAN_POINT('Ctrl Pts',(-0.555393178803588,-2.30595578311835,
12.8659073020546));
#94134=CARTESIAN_POINT('Ctrl Pts',(-0.529715174909093,-2.31198954099091,
12.8677369074191));
#94135=CARTESIAN_POINT('Ctrl Pts',(-0.495555684710337,-2.3194172233172,
12.8701320799261));
#94136=CARTESIAN_POINT('Ctrl Pts',(-0.487160828402515,-2.32119495637415,
12.8707176205607));
#94137=CARTESIAN_POINT('Ctrl Pts',(-0.473333259457575,-2.32404482467859,
12.8716768182493));
#94138=CARTESIAN_POINT('Ctrl Pts',(-0.467906203561732,-2.325143545657,12.8720519517167));
#94139=CARTESIAN_POINT('Ctrl Pts',(-0.457259059871297,-2.32726029894397,
12.8727852340639));
#94140=CARTESIAN_POINT('Ctrl Pts',(-0.452039328622863,-2.32827979271884,
12.8731434601125));
#94141=CARTESIAN_POINT('Ctrl Pts',(-0.439155929227791,-2.33075116020108,
12.8740246205334));
#94142=CARTESIAN_POINT('Ctrl Pts',(-0.431488354137501,-2.33218281991877,
12.874546415896));
#94143=CARTESIAN_POINT('Ctrl Pts',(-0.405010085574822,-2.33699168423568,
12.876339698901));
#94144=CARTESIAN_POINT('Ctrl Pts',(-0.386165119596994,-2.34017945027589,
12.8776010176428));
#94145=CARTESIAN_POINT('Ctrl Pts',(-0.232265581378858,-2.36430293206934,
12.8877950788121));
#94146=CARTESIAN_POINT('Ctrl Pts',(-0.0956515269750207,-2.3737600966249,
12.896185326393));
#94147=CARTESIAN_POINT('Ctrl Pts',(0.169420606660706,-2.36917351240096,
12.9124373076921));
#94148=CARTESIAN_POINT('Ctrl Pts',(0.297407414053778,-2.35652973621305,
12.9202765722158));
#94149=CARTESIAN_POINT('Ctrl Pts',(0.489999451807937,-2.32155853063592,
12.9326476911491));
#94150=CARTESIAN_POINT('Ctrl Pts',(0.555713278921655,-2.30671083762182,
12.9369710547778));
#94151=CARTESIAN_POINT('Ctrl Pts',(0.637355911334626,-2.28457288130548,
12.9425152962927));
#94152=CARTESIAN_POINT('Ctrl Pts',(0.653959662099677,-2.27987555403383,
12.9436518941431));
#94153=CARTESIAN_POINT('Ctrl Pts',(0.680444685230702,-2.27206961982427,
12.9454801107687));
#94154=CARTESIAN_POINT('Ctrl Pts',(0.690359625870287,-2.26907666423019,
12.9461679550795));
#94155=CARTESIAN_POINT('Ctrl Pts',(0.709130695247628,-2.26327595090908,
12.9474768605706));
#94156=CARTESIAN_POINT('Ctrl Pts',(0.717990573207929,-2.26048090136846,
12.9480974948316));
#94157=CARTESIAN_POINT('Ctrl Pts',(0.738097734960632,-2.25400750343949,
12.9495125730766));
#94158=CARTESIAN_POINT('Ctrl Pts',(0.749334297451787,-2.25029691235278,
12.9503080656128));
#94159=CARTESIAN_POINT('Ctrl Pts',(0.778411428116668,-2.24045299157937,
12.9523790312647));
#94160=CARTESIAN_POINT('Ctrl Pts',(0.796207129189219,-2.23419071039242,
12.9536587315121));
#94161=CARTESIAN_POINT('Ctrl Pts',(0.960320668021123,-2.17422966302381,
12.9655765794031));
#94162=CARTESIAN_POINT('Ctrl Pts',(1.10105794426764,-2.10645305080535,12.9766966511729));
#94163=CARTESIAN_POINT('Ctrl Pts',(1.33046335943887,-1.96667142281494,12.9962491212371));
#94164=CARTESIAN_POINT('Ctrl Pts',(1.4225061700333,-1.90115915901359,13.0045418739486));
#94165=CARTESIAN_POINT('Ctrl Pts',(1.56281094009702,-1.78538250479204,13.017640331429));
#94166=CARTESIAN_POINT('Ctrl Pts',(1.61414520362341,-1.73911070267697,13.0225427884958));
#94167=CARTESIAN_POINT('Ctrl Pts',(1.67161564073098,-1.68256718587607,13.0280949961018));
#94168=CARTESIAN_POINT('Ctrl Pts',(1.6797812696329,-1.67441514718958,13.0288854421533));
#94169=CARTESIAN_POINT('Ctrl Pts',(1.69223278752939,-1.66180158764746,13.030092729751));
#94170=CARTESIAN_POINT('Ctrl Pts',(1.69656111158187,-1.65738249079377,13.0305127694367));
#94171=CARTESIAN_POINT('Ctrl Pts',(1.70448564918962,-1.64922818826259,13.0312823969629));
#94172=CARTESIAN_POINT('Ctrl Pts',(1.70808689163478,-1.64549813641519,13.0316323674027));
#94173=CARTESIAN_POINT('Ctrl Pts',(1.71617657479548,-1.63706392642015,13.0324190478163));
#94174=CARTESIAN_POINT('Ctrl Pts',(1.72065791500058,-1.63235311044019,13.0328552110986));
#94175=CARTESIAN_POINT('Ctrl Pts',(1.73380283699778,-1.61842079654651,13.0341359195323));
#94176=CARTESIAN_POINT('Ctrl Pts',(1.74241223492008,-1.60914815148283,13.0349764487167));
#94177=CARTESIAN_POINT('Ctrl Pts',(1.81512604620786,-1.52956476187093,13.0420948306693));
#94178=CARTESIAN_POINT('Ctrl Pts',(1.87502864835406,-1.45551476617364,13.0480902466388));
#94179=CARTESIAN_POINT('Ctrl Pts',(1.99556106951763,-1.28667778983721,13.0609487725575));
#94180=CARTESIAN_POINT('Ctrl Pts',(2.05422611566453,-1.19078116991798,13.0677614080987));
#94181=CARTESIAN_POINT('Ctrl Pts',(2.1456581979111,-1.01431068431526,13.080015267604));
#94182=CARTESIAN_POINT('Ctrl Pts',(2.18120626342059,-0.935421090181152,
13.0854009400213));
#94183=CARTESIAN_POINT('Ctrl Pts',(2.23082609414845,-0.806992321232268,
13.0941855389465));
#94184=CARTESIAN_POINT('Ctrl Pts',(2.24773222211429,-0.758630941669378,
13.0974964167411));
#94185=CARTESIAN_POINT('Ctrl Pts',(2.26777309820446,-0.694731182493242,
13.1018932967783));
#94186=CARTESIAN_POINT('Ctrl Pts',(2.27233751666291,-0.679653169803669,
13.1029323539921));
#94187=CARTESIAN_POINT('Ctrl Pts',(2.2795608014815,-0.654905459723067,13.1046408108678));
#94188=CARTESIAN_POINT('Ctrl Pts',(2.28230919584446,-0.645262224305075,
13.1053072807735));
#94189=CARTESIAN_POINT('Ctrl Pts',(2.28751159021908,-0.626559557436064,
13.1066014554102));
#94190=CARTESIAN_POINT('Ctrl Pts',(2.28997312925566,-0.617502402677312,
13.1072289014604));
#94191=CARTESIAN_POINT('Ctrl Pts',(2.29553977270727,-0.59652900238041,13.1086836282938));
#94192=CARTESIAN_POINT('Ctrl Pts',(2.2986059382747,-0.584602796202754,13.1095121512591));
#94193=CARTESIAN_POINT('Ctrl Pts',(2.30824328893264,-0.545868856115087,
13.1122075989894));
#94194=CARTESIAN_POINT('Ctrl Pts',(2.31443921213001,-0.518971010775866,
13.1140864887592));
#94195=CARTESIAN_POINT('Ctrl Pts',(2.36130122268905,-0.297967524982086,
13.1295883644198));
#94196=CARTESIAN_POINT('Ctrl Pts',(2.37793496214227,-0.0996058784028845,
13.1440044303405));
#94197=CARTESIAN_POINT('Ctrl Pts',(2.36884002499085,0.119287552253391,13.1600001153947));
#94198=CARTESIAN_POINT('Ctrl Pts',(2.36770012031077,0.140102590333102,13.1615209745401));
#94199=CARTESIAN_POINT('Ctrl Pts',(2.35968690899317,0.257949369536178,13.1701234460742));
#94200=CARTESIAN_POINT('Ctrl Pts',(2.34712282899186,0.354511968694002,13.1771450855675));
#94201=CARTESIAN_POINT('Ctrl Pts',(2.32508783213836,0.468528844570008,13.1852182507133));
#94202=CARTESIAN_POINT('Ctrl Pts',(2.32129423747973,0.486976205396619,13.1865174074998));
#94203=CARTESIAN_POINT('Ctrl Pts',(2.31567560534015,0.512739045552493,13.1883200600941));
#94204=CARTESIAN_POINT('Ctrl Pts',(2.31403494138933,0.520093387744145,13.188833309881));
#94205=CARTESIAN_POINT('Ctrl Pts',(2.31117598739048,0.532627381666701,13.1897056055392));
#94206=CARTESIAN_POINT('Ctrl Pts',(2.30997527318363,0.53781094440367,13.1900656389182));
#94207=CARTESIAN_POINT('Ctrl Pts',(2.30762506290797,0.547803871124166,13.1907582859238));
#94208=CARTESIAN_POINT('Ctrl Pts',(2.30647796480332,0.55261370884598,13.1910910395974));
#94209=CARTESIAN_POINT('Ctrl Pts',(2.30367764894772,0.564194945021064,13.1918908004721));
#94210=CARTESIAN_POINT('Ctrl Pts',(2.30200959446868,0.57096276262445,13.1923569656265));
#94211=CARTESIAN_POINT('Ctrl Pts',(2.29574764300367,0.59589587826222,13.1940702653053));
#94212=CARTESIAN_POINT('Ctrl Pts',(2.29096821941692,0.614014503102291,13.1953072888866));
#94213=CARTESIAN_POINT('Ctrl Pts',(2.24637990683325,0.775273366269205,13.2062610024248));
#94214=CARTESIAN_POINT('Ctrl Pts',(2.19341154052799,0.914456268135927,13.2153324695488));
#94215=CARTESIAN_POINT('Ctrl Pts',(2.04922777007196,1.20725371510017,13.2353321239612));
#94216=CARTESIAN_POINT('Ctrl Pts',(1.95303291388866,1.35736762112661,13.2462423194179));
#94217=CARTESIAN_POINT('Ctrl Pts',(1.82771824553745,1.51165031431606,13.2592186109098));
#94218=CARTESIAN_POINT('Ctrl Pts',(1.8142380990348,1.52780258244728,13.2606003600199));
#94219=CARTESIAN_POINT('Ctrl Pts',(1.79327365962642,1.55225398931975,13.2627292126041));
#94220=CARTESIAN_POINT('Ctrl Pts',(1.78594238108493,1.56068339834222,13.2634700344818));
#94221=CARTESIAN_POINT('Ctrl Pts',(1.77303409324476,1.57531512165759,13.2647682813023));
#94222=CARTESIAN_POINT('Ctrl Pts',(1.7674833646384,1.58154044557804,13.2653246033569));
#94223=CARTESIAN_POINT('Ctrl Pts',(1.75487377164345,1.59553322364326,13.2665841280606));
#94224=CARTESIAN_POINT('Ctrl Pts',(1.74779598968229,1.60328331696349,13.2672881230355));
#94225=CARTESIAN_POINT('Ctrl Pts',(1.72851699179423,1.62411423408215,13.2691979010369));
#94226=CARTESIAN_POINT('Ctrl Pts',(1.71621905558487,1.63710419915523,13.2704078034361));
#94227=CARTESIAN_POINT('Ctrl Pts',(1.65802551091313,1.69719604038684,13.2760957583057));
#94228=CARTESIAN_POINT('Ctrl Pts',(1.6103345845051,1.74251084646752,13.2806518487746));
#94229=CARTESIAN_POINT('Ctrl Pts',(1.416811230463,1.91165598472959,13.2987581489705));
#94230=CARTESIAN_POINT('Ctrl Pts',(1.25810836555815,2.01963541740983,13.3128840143935));
#94231=CARTESIAN_POINT('Ctrl Pts',(1.01894128090298,2.14313622572454,13.3323844957816));
#94232=CARTESIAN_POINT('Ctrl Pts',(0.947951928265619,2.17546866316755,13.337963725656));
#94233=CARTESIAN_POINT('Ctrl Pts',(0.859802384673073,2.2104802475581,13.3445426836938));
#94234=CARTESIAN_POINT('Ctrl Pts',(0.844045961541004,2.21654450020161,13.3457054101287));
#94235=CARTESIAN_POINT('Ctrl Pts',(0.821467496859058,2.22495870265292,13.34735140577));
#94236=CARTESIAN_POINT('Ctrl Pts',(0.814697856314741,2.22744640413542,13.347842353289));
#94237=CARTESIAN_POINT('Ctrl Pts',(0.802966870101622,2.23169666102543,13.3486885451363));
#94238=CARTESIAN_POINT('Ctrl Pts',(0.798010847093563,2.23347363349604,13.3490446328898));
#94239=CARTESIAN_POINT('Ctrl Pts',(0.78762372501528,2.23715892746806,13.3497879594987));
#94240=CARTESIAN_POINT('Ctrl Pts',(0.782191569376079,2.23906398960705,13.3501750066713));
#94241=CARTESIAN_POINT('Ctrl Pts',(0.767708607622437,2.24408403902726,13.3512025743881));
#94242=CARTESIAN_POINT('Ctrl Pts',(0.758645670351082,2.24716408727175,13.3518410700863));
#94243=CARTESIAN_POINT('Ctrl Pts',(0.719161164335299,2.26031683425736,13.3546042131311));
#94244=CARTESIAN_POINT('Ctrl Pts',(0.688554189797122,2.2698278236675,13.3566982821296));
#94245=CARTESIAN_POINT('Ctrl Pts',(0.417116847700562,2.34817947780277,13.3749282247614));
#94246=CARTESIAN_POINT('Ctrl Pts',(0.166965150983491,2.37909465177184,13.3895358083447));
#94247=CARTESIAN_POINT('Ctrl Pts',(-0.149283218388116,2.3679644941074,13.409551387553));
#94248=CARTESIAN_POINT('Ctrl Pts',(-0.215015205268351,2.36290256392582,
13.4137846972655));
#94249=CARTESIAN_POINT('Ctrl Pts',(-0.297464937205378,2.35308444332483,
13.419227497168));
#94250=CARTESIAN_POINT('Ctrl Pts',(-0.314460225316486,2.35087356685176,
13.4203565044592));
#94251=CARTESIAN_POINT('Ctrl Pts',(-0.341659475637941,2.34703506531036,
13.4221753924901));
#94252=CARTESIAN_POINT('Ctrl Pts',(-0.351879571878366,2.34552458017929,
13.4228615675343));
#94253=CARTESIAN_POINT('Ctrl Pts',(-0.371275884753336,2.34252826801927,
13.4241691677416));
#94254=CARTESIAN_POINT('Ctrl Pts',(-0.380453895290972,2.34105516773536,
13.4247901784174));
#94255=CARTESIAN_POINT('Ctrl Pts',(-0.401340443466845,2.33757674096446,
13.4262087255005));
#94256=CARTESIAN_POINT('Ctrl Pts',(-0.413042973831832,2.33553733951994,
13.4270073298483));
#94257=CARTESIAN_POINT('Ctrl Pts',(-0.443438897598897,2.33000464491128,
13.4290917544037));
#94258=CARTESIAN_POINT('Ctrl Pts',(-0.46210616025162,2.32637433812214,13.4303818929892));
#94259=CARTESIAN_POINT('Ctrl Pts',(-0.622927142581399,2.29308677420926,
13.4415857490044));
#94260=CARTESIAN_POINT('Ctrl Pts',(-0.762096568076674,2.25066207411848,
13.4519136922315));
#94261=CARTESIAN_POINT('Ctrl Pts',(-0.988181772134961,2.15835660844579,
13.4696516152788));
#94262=CARTESIAN_POINT('Ctrl Pts',(-1.07743547803684,2.11521605504404,13.4769212064894));
#94263=CARTESIAN_POINT('Ctrl Pts',(-1.23694037536483,2.02539768702431,13.4902090297533));
#94264=CARTESIAN_POINT('Ctrl Pts',(-1.30791634917458,1.98030682670697,13.4962393583677));
#94265=CARTESIAN_POINT('Ctrl Pts',(-1.39062866117043,1.92136856050259,13.5032894703318));
#94266=CARTESIAN_POINT('Ctrl Pts',(-1.40478899155932,1.91103980949199,13.5044972099905));
#94267=CARTESIAN_POINT('Ctrl Pts',(-1.424700977243,1.89617477892827,13.5061951158166));
#94268=CARTESIAN_POINT('Ctrl Pts',(-1.43054769967514,1.89176767849098,13.5066936196878));
#94269=CARTESIAN_POINT('Ctrl Pts',(-1.44057788464989,1.8841341059943,13.5075485954226));
#94270=CARTESIAN_POINT('Ctrl Pts',(-1.44477111738726,1.88092062346485,13.507905959358));
#94271=CARTESIAN_POINT('Ctrl Pts',(-1.45347490386056,1.87420419913461,13.5086475395512));
#94272=CARTESIAN_POINT('Ctrl Pts',(-1.45798357040366,1.87069895664694,13.5090315893851));
#94273=CARTESIAN_POINT('Ctrl Pts',(-1.4698535142068,1.86140174127125,13.51004254892));
#94274=CARTESIAN_POINT('Ctrl Pts',(-1.47719331110825,1.85558231415524,13.510667547924));
#94275=CARTESIAN_POINT('Ctrl Pts',(-1.50809006935702,1.83078601625937,13.5132988556975));
#94276=CARTESIAN_POINT('Ctrl Pts',(-1.53131854773121,1.81140189146337,13.5152780554275));
#94277=CARTESIAN_POINT('Ctrl Pts',(-1.74491179341248,1.62611242206457,13.53355577674));
#94278=CARTESIAN_POINT('Ctrl Pts',(-1.90802639374918,1.43123425867429,13.5482687024767));
#94279=CARTESIAN_POINT('Ctrl Pts',(-2.05967506020098,1.17679212077054,13.5670027289252));
#94280=CARTESIAN_POINT('Ctrl Pts',(-2.08096963471221,1.13871246435083,13.5697901062475));
#94281=CARTESIAN_POINT('Ctrl Pts',(-2.11566382405464,1.07244437286819,13.5746305118822));
#94282=CARTESIAN_POINT('Ctrl Pts',(-2.12957972161713,1.04453837175365,13.5766657565784));
#94283=CARTESIAN_POINT('Ctrl Pts',(-2.14854084804998,1.00456012869067,13.5795811064392));
#94284=CARTESIAN_POINT('Ctrl Pts',(-2.15404299289103,0.992707208167887,
13.5804454101347));
#94285=CARTESIAN_POINT('Ctrl Pts',(-2.16336581961056,0.972181157002413,
13.5819423516776));
#94286=CARTESIAN_POINT('Ctrl Pts',(-2.16723302394512,0.963529390802686,
13.5825733758317));
#94287=CARTESIAN_POINT('Ctrl Pts',(-2.17454358820276,0.946907399920196,
13.5837859397255));
#94288=CARTESIAN_POINT('Ctrl Pts',(-2.17799524484547,0.938940973105493,
13.5843671835787));
#94289=CARTESIAN_POINT('Ctrl Pts',(-2.1860033222167,0.920176555789852,13.5857365877449));
#94290=CARTESIAN_POINT('Ctrl Pts',(-2.19052356560152,0.909363468870273,
13.5865259623491));
#94291=CARTESIAN_POINT('Ctrl Pts',(-2.20589849194404,0.871804488526548,
13.5892689786342));
#94292=CARTESIAN_POINT('Ctrl Pts',(-2.21634456726761,0.844895173250619,
13.5912362625293));
#94293=CARTESIAN_POINT('Ctrl Pts',(-2.28496930534364,0.658078748583226,
13.6049137389491));
#94294=CARTESIAN_POINT('Ctrl Pts',(-2.32627207435697,0.492534002123081,
13.6171861893278));
#94295=CARTESIAN_POINT('Ctrl Pts',(-2.3564272854985,0.273881811246033,13.633303083632));
#94296=CARTESIAN_POINT('Ctrl Pts',(-2.3617342843641,0.22353792809192,13.6370032909136));
#94297=CARTESIAN_POINT('Ctrl Pts',(-2.3654265016339,0.173076653156924,13.6406850658798));
#94298=CARTESIAN_POINT('Origin',(0.,0.,-1.84858989190503));
#94299=CARTESIAN_POINT('',(-2.36542649432832,0.173076753001719,14.8389825814723));
#94300=CARTESIAN_POINT('',(-2.3654265029177,0.173076635611311,14.6411792785331));
#94301=CARTESIAN_POINT('',(-2.36542649454111,0.173076750093529,-1.84858989190503));
#94302=CARTESIAN_POINT('',(-2.37174914129228,0.00201823668619566,13.8479759907678));
#94303=CARTESIAN_POINT('Ctrl Pts',(-2.36542649432832,0.173076753001719,
14.8389825814723));
#94304=CARTESIAN_POINT('Ctrl Pts',(-2.3614020125275,0.228079032120752,14.8351425342295));
#94305=CARTESIAN_POINT('Ctrl Pts',(-2.35546045181701,0.282922847275077,
14.8312473450475));
#94306=CARTESIAN_POINT('Ctrl Pts',(-2.32776585976983,0.475558337415043,
14.8173422565782));
#94307=CARTESIAN_POINT('Ctrl Pts',(-2.29578163802699,0.61158049665499,14.8070970944981));
#94308=CARTESIAN_POINT('Ctrl Pts',(-2.21939821692657,0.842790865555311,
14.7893681751657));
#94309=CARTESIAN_POINT('Ctrl Pts',(-2.18028755787251,0.939348953397733,
14.7818688675747));
#94310=CARTESIAN_POINT('Ctrl Pts',(-2.12945263491179,1.04440852039878,14.7738162003158));
#94311=CARTESIAN_POINT('Ctrl Pts',(-2.12385882784374,1.0557373626657,14.7729493760261));
#94312=CARTESIAN_POINT('Ctrl Pts',(-2.11527540425551,1.07277656358541,14.7716485190868));
#94313=CARTESIAN_POINT('Ctrl Pts',(-2.11235271387947,1.07852009990428,14.7712105298397));
#94314=CARTESIAN_POINT('Ctrl Pts',(-2.10706947699421,1.08879861216497,14.7704277086525));
#94315=CARTESIAN_POINT('Ctrl Pts',(-2.10471765450586,1.09333791444461,14.7700823474971));
#94316=CARTESIAN_POINT('Ctrl Pts',(-2.0995449760829,1.10324326656844,14.7693295106624));
#94317=CARTESIAN_POINT('Ctrl Pts',(-2.09671822246143,1.10860611107363,14.7689224125096));
#94318=CARTESIAN_POINT('Ctrl Pts',(-2.0886079695387,1.12385068988137,14.7677664238005));
#94319=CARTESIAN_POINT('Ctrl Pts',(-2.08327487097476,1.13370606768764,14.767020586303));
#94320=CARTESIAN_POINT('Ctrl Pts',(-2.04717315776957,1.19930571430767,14.7620635953376));
#94321=CARTESIAN_POINT('Ctrl Pts',(-2.01423723317738,1.25383498793287,14.7579791816982));
#94322=CARTESIAN_POINT('Ctrl Pts',(-1.86232455973589,1.48387481152358,14.7406124006808));
#94323=CARTESIAN_POINT('Ctrl Pts',(-1.72231641754659,1.64431575023663,14.7280561531223));
#94324=CARTESIAN_POINT('Ctrl Pts',(-1.51146028422509,1.82903024844436,14.7103594773067));
#94325=CARTESIAN_POINT('Ctrl Pts',(-1.45816436874979,1.8717956963686,14.7059791279234));
#94326=CARTESIAN_POINT('Ctrl Pts',(-1.38882917100014,1.9226713065059,14.7003469749911));
#94327=CARTESIAN_POINT('Ctrl Pts',(-1.37444074962452,1.932983190984,14.6991817101431));
#94328=CARTESIAN_POINT('Ctrl Pts',(-1.35136637512529,1.94913223205842,14.6973178332736));
#94329=CARTESIAN_POINT('Ctrl Pts',(-1.34275469855957,1.95507476874487,14.696623262589));
#94330=CARTESIAN_POINT('Ctrl Pts',(-1.32656291567021,1.96609055866013,14.6953191344407));
#94331=CARTESIAN_POINT('Ctrl Pts',(-1.3189922916831,1.97117746145599,14.6947101094603));
#94332=CARTESIAN_POINT('Ctrl Pts',(-1.30200267756705,1.98245153446869,14.6933448911927));
#94333=CARTESIAN_POINT('Ctrl Pts',(-1.29256860427577,1.9886154617011,14.6925878433771));
#94334=CARTESIAN_POINT('Ctrl Pts',(-1.26460542229226,2.00660267640408,14.6903467207935));
#94335=CARTESIAN_POINT('Ctrl Pts',(-1.24595590779675,2.01823561409474,14.6888556472716));
#94336=CARTESIAN_POINT('Ctrl Pts',(-1.09905939912294,2.10705266996693,14.6771353604057));
#94337=CARTESIAN_POINT('Ctrl Pts',(-0.963951845381477,2.17218413718589,
14.6664668985994));
#94338=CARTESIAN_POINT('Ctrl Pts',(-0.667864472189908,2.28182970133326,
14.6435029238538));
#94339=CARTESIAN_POINT('Ctrl Pts',(-0.506459933749803,2.32299241982373,
14.6312182235382));
#94340=CARTESIAN_POINT('Ctrl Pts',(-0.336837498890614,2.34771517576119,
14.6192116560624));
#94341=CARTESIAN_POINT('Ctrl Pts',(-0.331600166535559,2.34846064003882,
14.618841846049));
#94342=CARTESIAN_POINT('Ctrl Pts',(-0.304918044152087,2.35216744604212,
14.6169625838682));
#94343=CARTESIAN_POINT('Ctrl Pts',(-0.283435003853626,2.35485273216162,
14.6154651823659));
#94344=CARTESIAN_POINT('Ctrl Pts',(-0.25382435813423,2.35814282043155,14.6134255161708));
#94345=CARTESIAN_POINT('Ctrl Pts',(-0.245726716122556,2.35900037139999,
14.6128702160168));
#94346=CARTESIAN_POINT('Ctrl Pts',(-0.232795285031159,2.36030251815304,
14.6119875767147));
#94347=CARTESIAN_POINT('Ctrl Pts',(-0.227964364108627,2.36077399844215,
14.6116587617775));
#94348=CARTESIAN_POINT('Ctrl Pts',(-0.217896631833942,2.36172538071267,
14.6109754714222));
#94349=CARTESIAN_POINT('Ctrl Pts',(-0.212659636586564,2.36220269996234,
14.610621153585));
#94350=CARTESIAN_POINT('Ctrl Pts',(-0.199949823355986,2.36331851009633,
14.6097638618266));
#94351=CARTESIAN_POINT('Ctrl Pts',(-0.192475393937949,2.36393898792157,
14.6092618906104));
#94352=CARTESIAN_POINT('Ctrl Pts',(-0.166041669104612,2.36600713639777,
14.6074939730283));
#94353=CARTESIAN_POINT('Ctrl Pts',(-0.147067420757558,2.36726230825546,
14.6062382757939));
#94354=CARTESIAN_POINT('Ctrl Pts',(-0.100211970523747,2.36979629669898,
14.6031657232352));
#94355=CARTESIAN_POINT('Ctrl Pts',(-0.0723187815931293,2.3708114790126,
14.6013612984657));
#94356=CARTESIAN_POINT('Ctrl Pts',(0.164682695112942,2.37525029564411,14.5861898389889));
#94357=CARTESIAN_POINT('Ctrl Pts',(0.373395163448005,2.35149516409628,14.5738139188356));
#94358=CARTESIAN_POINT('Ctrl Pts',(0.66579311152404,2.27825117407371,14.5550034499326));
#94359=CARTESIAN_POINT('Ctrl Pts',(0.753888379076735,2.25063504354883,14.5491441322446));
#94360=CARTESIAN_POINT('Ctrl Pts',(0.856599263480938,2.21172904269297,14.5419632546389));
#94361=CARTESIAN_POINT('Ctrl Pts',(0.872983393215745,2.20531349792047,14.5408070339504));
#94362=CARTESIAN_POINT('Ctrl Pts',(0.899827365795049,2.19445616723867,14.5388941507435));
#94363=CARTESIAN_POINT('Ctrl Pts',(0.910329555800329,2.19012037348924,14.5381410604948));
#94364=CARTESIAN_POINT('Ctrl Pts',(0.929211988542956,2.18216554422235,14.5367783278065));
#94365=CARTESIAN_POINT('Ctrl Pts',(0.93760331234588,2.17857325025094,14.5361696040151));
#94366=CARTESIAN_POINT('Ctrl Pts',(0.955507824629391,2.17078579265972,14.5348639633414));
#94367=CARTESIAN_POINT('Ctrl Pts',(0.965014553459373,2.16657634672054,14.5341665678627));
#94368=CARTESIAN_POINT('Ctrl Pts',(0.990779656584828,2.15496470000367,14.5322650262955));
#94369=CARTESIAN_POINT('Ctrl Pts',(1.00698229716312,2.14744122360354,14.5310567316241));
#94370=CARTESIAN_POINT('Ctrl Pts',(1.09344492277928,2.10609978824017,14.5245401301736));
#94371=CARTESIAN_POINT('Ctrl Pts',(1.16208241806356,2.06901912609388,14.5191191829032));
#94372=CARTESIAN_POINT('Ctrl Pts',(1.38520005734614,1.93387433498121,14.5006373631487));
#94373=CARTESIAN_POINT('Ctrl Pts',(1.53014170349035,1.82134602101831,14.4871187880885));
#94374=CARTESIAN_POINT('Ctrl Pts',(1.68503945359044,1.66943194150703,14.4714173817469));
#94375=CARTESIAN_POINT('Ctrl Pts',(1.70886925854408,1.64503100251655,14.4689632777369));
#94376=CARTESIAN_POINT('Ctrl Pts',(1.76589338603999,1.58406330280113,14.4630103526347));
#94377=CARTESIAN_POINT('Ctrl Pts',(1.79849009039522,1.54695514945682,14.45953704692));
#94378=CARTESIAN_POINT('Ctrl Pts',(1.83620691712339,1.50121293735987,14.4554575092086));
#94379=CARTESIAN_POINT('Ctrl Pts',(1.84245901027645,1.49353303608209,14.4547791679922));
#94380=CARTESIAN_POINT('Ctrl Pts',(1.85264435230421,1.48086034350073,14.4536709138133));
#94381=CARTESIAN_POINT('Ctrl Pts',(1.85660588268961,1.47589059616435,14.4532390653167));
#94382=CARTESIAN_POINT('Ctrl Pts',(1.86371546914683,1.46689768110117,14.4524626882875));
#94383=CARTESIAN_POINT('Ctrl Pts',(1.8668705254502,1.46288024097705,14.4521176701031));
#94384=CARTESIAN_POINT('Ctrl Pts',(1.87378732991716,1.45401401772847,14.4513602243834));
#94385=CARTESIAN_POINT('Ctrl Pts',(1.87754324314238,1.44916082399513,14.4509482083382));
#94386=CARTESIAN_POINT('Ctrl Pts',(1.88831762339303,1.43512653239419,14.4497640346406));
#94387=CARTESIAN_POINT('Ctrl Pts',(1.89528800461799,1.42590848369943,14.4489951684103));
#94388=CARTESIAN_POINT('Ctrl Pts',(1.94564823884009,1.35828734841707,14.4434167151619));
#94389=CARTESIAN_POINT('Ctrl Pts',(1.98640255118573,1.29795950757444,14.4387731377725));
#94390=CARTESIAN_POINT('Ctrl Pts',(2.08193205575991,1.14148175315283,14.4272853826972));
#94391=CARTESIAN_POINT('Ctrl Pts',(2.13287567818831,1.04319960590128,14.4205608433446));
#94392=CARTESIAN_POINT('Ctrl Pts',(2.23828765215156,0.799540074808669,14.4042725433401));
#94393=CARTESIAN_POINT('Ctrl Pts',(2.28571067915955,0.651699933567038,14.3946716787535));
#94394=CARTESIAN_POINT('Ctrl Pts',(2.32232527186871,0.482029973092071,14.3833370262321));
#94395=CARTESIAN_POINT('Ctrl Pts',(2.32605254044154,0.463710156781885,14.3821096695008));
#94396=CARTESIAN_POINT('Ctrl Pts',(2.33175882300326,0.433861308176566,14.3801033048129));
#94397=CARTESIAN_POINT('Ctrl Pts',(2.33386984982371,0.42235809351864,14.3793285022335));
#94398=CARTESIAN_POINT('Ctrl Pts',(2.33748254485082,0.401817541018991,14.3779419550727));
#94399=CARTESIAN_POINT('Ctrl Pts',(2.33901710283989,0.39278616615475,14.3773312694123));
#94400=CARTESIAN_POINT('Ctrl Pts',(2.34214792138358,0.373691051012584,14.3760377881741));
#94401=CARTESIAN_POINT('Ctrl Pts',(2.3437317226846,0.363625485493788,14.3753546103965));
#94402=CARTESIAN_POINT('Ctrl Pts',(2.34777256758438,0.336820819772042,14.3735315604107));
#94403=CARTESIAN_POINT('Ctrl Pts',(2.3501154081109,0.320065362640248,14.3723881025388));
#94404=CARTESIAN_POINT('Ctrl Pts',(2.36060566184537,0.238703386839367,14.3668157760449));
#94405=CARTESIAN_POINT('Ctrl Pts',(2.36626854351113,0.173810654741295,14.3623096528739));
#94406=CARTESIAN_POINT('Ctrl Pts',(2.38032334842894,-0.132327988621367,
14.340744983751));
#94407=CARTESIAN_POINT('Ctrl Pts',(2.35452810697936,-0.37365024381514,14.3226635346676));
#94408=CARTESIAN_POINT('Ctrl Pts',(2.28228604974796,-0.646569493660247,
14.3026407962111));
#94409=CARTESIAN_POINT('Ctrl Pts',(2.27075790852634,-0.685959730104411,
14.299767256913));
#94410=CARTESIAN_POINT('Ctrl Pts',(2.25508161952206,-0.734785582349324,
14.2962421800859));
#94411=CARTESIAN_POINT('Ctrl Pts',(2.25188745200605,-0.744517209917209,
14.2955414405841));
#94412=CARTESIAN_POINT('Ctrl Pts',(2.2467498075832,-0.759834410856349,14.2944417686379));
#94413=CARTESIAN_POINT('Ctrl Pts',(2.24484835788753,-0.765433786711405,
14.2940404625193));
#94414=CARTESIAN_POINT('Ctrl Pts',(2.24142571780832,-0.77539029607059,14.2933281873422));
#94415=CARTESIAN_POINT('Ctrl Pts',(2.23991276206047,-0.779750074491153,
14.2930167486488));
#94416=CARTESIAN_POINT('Ctrl Pts',(2.23627877140925,-0.790124032176763,
14.2922767459517));
#94417=CARTESIAN_POINT('Ctrl Pts',(2.23414619835565,-0.796134094526861,
14.2918488712038));
#94418=CARTESIAN_POINT('Ctrl Pts',(2.22768785060494,-0.81410482678005,14.2905717882783));
#94419=CARTESIAN_POINT('Ctrl Pts',(2.22328999363442,-0.826039618172592,
14.2897267179865));
#94420=CARTESIAN_POINT('Ctrl Pts',(2.21293871573412,-0.853448990776743,
14.2877917561236));
#94421=CARTESIAN_POINT('Ctrl Pts',(2.20691855158682,-0.86889785440863,14.2867054516841));
#94422=CARTESIAN_POINT('Ctrl Pts',(2.18600202948953,-0.920953324840884,
14.2830556117379));
#94423=CARTESIAN_POINT('Ctrl Pts',(2.17035222050802,-0.957252062871989,
14.2805282152508));
#94424=CARTESIAN_POINT('Ctrl Pts',(2.08239057215326,-1.14801170044348,14.2672544360006));
#94425=CARTESIAN_POINT('Ctrl Pts',(1.99448105722603,-1.294733522514,14.2570414815074));
#94426=CARTESIAN_POINT('Ctrl Pts',(1.82491817790297,-1.51890948996825,14.2396220593414));
#94427=CARTESIAN_POINT('Ctrl Pts',(1.75217675144003,-1.60227468719246,14.2326524475735));
#94428=CARTESIAN_POINT('Ctrl Pts',(1.66095843026834,-1.69314755491943,14.2242404474436));
#94429=CARTESIAN_POINT('Ctrl Pts',(1.64787291576171,-1.70588580291266,14.2230411114145));
#94430=CARTESIAN_POINT('Ctrl Pts',(1.62626260432966,-1.72644193256843,14.2210715326259));
#94431=CARTESIAN_POINT('Ctrl Pts',(1.61782524817451,-1.73435096307022,14.2203052403666));
#94432=CARTESIAN_POINT('Ctrl Pts',(1.60261172925364,-1.7484042350013,14.2189281171644));
#94433=CARTESIAN_POINT('Ctrl Pts',(1.595857182125,-1.75457162120467,14.2183182901236));
#94434=CARTESIAN_POINT('Ctrl Pts',(1.58144630540479,-1.7675777298281,14.2170204762423));
#94435=CARTESIAN_POINT('Ctrl Pts',(1.57378093152755,-1.77440610393022,14.2163320711971));
#94436=CARTESIAN_POINT('Ctrl Pts',(1.55310532298312,-1.79258472859395,14.2144802153294));
#94437=CARTESIAN_POINT('Ctrl Pts',(1.54001528509315,-1.80384285556825,14.2133129762345));
#94438=CARTESIAN_POINT('Ctrl Pts',(1.47361671150651,-1.85969960857639,14.2074168990212));
#94439=CARTESIAN_POINT('Ctrl Pts',(1.4184939116039,-1.90207837219248,14.2025994923366));
#94440=CARTESIAN_POINT('Ctrl Pts',(1.25002887732396,-2.02019596502572,14.188086594073));
#94441=CARTESIAN_POINT('Ctrl Pts',(1.13194137124756,-2.08865138613334,14.1781615053262));
#94442=CARTESIAN_POINT('Ctrl Pts',(0.893907777729786,-2.20049967436686,
14.1589489649872));
#94443=CARTESIAN_POINT('Ctrl Pts',(0.775018034314984,-2.24513333449316,
14.1497002682192));
#94444=CARTESIAN_POINT('Ctrl Pts',(0.634684710045782,-2.2853317256098,14.1395438220636));
#94445=CARTESIAN_POINT('Ctrl Pts',(0.616186102927349,-2.29038872746865,
14.1382199980675));
#94446=CARTESIAN_POINT('Ctrl Pts',(0.590130937384832,-2.29717294675024,
14.1363782966847));
#94447=CARTESIAN_POINT('Ctrl Pts',(0.582624754501801,-2.29908818235827,
14.1358503773092));
#94448=CARTESIAN_POINT('Ctrl Pts',(0.570472835117067,-2.30212546259906,
14.1350001504593));
#94449=CARTESIAN_POINT('Ctrl Pts',(0.565832935305995,-2.30327028190814,
14.1346765551882));
#94450=CARTESIAN_POINT('Ctrl Pts',(0.556008371373249,-2.30566285266996,
14.133993621224));
#94451=CARTESIAN_POINT('Ctrl Pts',(0.550822897572116,-2.3069071580499,14.1336344890514));
#94452=CARTESIAN_POINT('Ctrl Pts',(0.537972579863874,-2.30994491941135,
14.1327476887345));
#94453=CARTESIAN_POINT('Ctrl Pts',(0.530302835566549,-2.31171774540812,
14.132221194423));
#94454=CARTESIAN_POINT('Ctrl Pts',(0.501646433458125,-2.31819141710669,
14.1302639873015));
#94455=CARTESIAN_POINT('Ctrl Pts',(0.480604186342854,-2.32264510584657,
14.1288466546656));
#94456=CARTESIAN_POINT('Ctrl Pts',(0.427224006931558,-2.33318672682754,
14.1252944326726));
#94457=CARTESIAN_POINT('Ctrl Pts',(0.39481375911396,-2.33888926214865,14.1231775836762));
#94458=CARTESIAN_POINT('Ctrl Pts',(0.247124019929762,-2.36171732498843,
14.1136690406334));
#94459=CARTESIAN_POINT('Ctrl Pts',(0.130789282120243,-2.37100772415138,
14.1065523347632));
#94460=CARTESIAN_POINT('Ctrl Pts',(-0.146525832010526,-2.3726721650846,
14.089560617621));
#94461=CARTESIAN_POINT('Ctrl Pts',(-0.306946807904424,-2.3572903870215,
14.0796850104309));
#94462=CARTESIAN_POINT('Ctrl Pts',(-0.492959690905339,-2.32013511567851,
14.0673940742713));
#94463=CARTESIAN_POINT('Ctrl Pts',(-0.521242403944802,-2.31394521298482,
14.065502999199));
#94464=CARTESIAN_POINT('Ctrl Pts',(-0.560726259194147,-2.3045432504025,
14.0628285185071));
#94465=CARTESIAN_POINT('Ctrl Pts',(-0.572028589097567,-2.30176384884208,
14.0620589591454));
#94466=CARTESIAN_POINT('Ctrl Pts',(-0.591625920194157,-2.29679133634868,
14.060717464676));
#94467=CARTESIAN_POINT('Ctrl Pts',(-0.599930398558999,-2.29463617720601,
14.0601467614224));
#94468=CARTESIAN_POINT('Ctrl Pts',(-0.617233910138552,-2.29004525646018,
14.0589528590178));
#94469=CARTESIAN_POINT('Ctrl Pts',(-0.62623062424451,-2.28760140265372,
14.0583294063964));
#94470=CARTESIAN_POINT('Ctrl Pts',(-0.647522737391686,-2.2816826284064,
14.0568473824666));
#94471=CARTESIAN_POINT('Ctrl Pts',(-0.659804820587774,-2.27816129801967,
14.0559873146583));
#94472=CARTESIAN_POINT('Ctrl Pts',(-0.699932460915938,-2.2663048012793,
14.0531599676609));
#94473=CARTESIAN_POINT('Ctrl Pts',(-0.727652378417647,-2.25755726109058,
14.051179315727));
#94474=CARTESIAN_POINT('Ctrl Pts',(-0.793600692890124,-2.23540526412616,
14.0463988198523));
#94475=CARTESIAN_POINT('Ctrl Pts',(-0.831659048533409,-2.22152687153939,
14.0435841469416));
#94476=CARTESIAN_POINT('Ctrl Pts',(-1.06563532935693,-2.12934986788801,
14.0259271422914));
#94477=CARTESIAN_POINT('Ctrl Pts',(-1.2507185170132,-2.02617540701597,14.0102831756595));
#94478=CARTESIAN_POINT('Ctrl Pts',(-1.43172899683686,-1.89091949464764,
13.9939812907566));
#94479=CARTESIAN_POINT('Ctrl Pts',(-1.44369633829074,-1.88179843590999,
13.9928988888703));
#94480=CARTESIAN_POINT('Ctrl Pts',(-1.50182145098892,-1.83661678339207,
13.987621698453));
#94481=CARTESIAN_POINT('Ctrl Pts',(-1.54672378788611,-1.79896518351512,
13.9834822457971));
#94482=CARTESIAN_POINT('Ctrl Pts',(-1.59792210108302,-1.75269838740008,
13.9787296496769));
#94483=CARTESIAN_POINT('Ctrl Pts',(-1.60560851278842,-1.74565975837149,
13.9780152454683));
#94484=CARTESIAN_POINT('Ctrl Pts',(-1.61802278778451,-1.73414034654459,
13.9768603116519));
#94485=CARTESIAN_POINT('Ctrl Pts',(-1.6227789263163,-1.72969044692717,13.9764175682375));
#94486=CARTESIAN_POINT('Ctrl Pts',(-1.6312387741586,-1.72170970447448,13.9756296703288));
#94487=CARTESIAN_POINT('Ctrl Pts',(-1.63494943602169,-1.71818642416049,
13.9752839561611));
#94488=CARTESIAN_POINT('Ctrl Pts',(-1.6421509175494,-1.71130414982235,13.9746127737307));
#94489=CARTESIAN_POINT('Ctrl Pts',(-1.64564283062835,-1.70794648753418,
13.9742872080722));
#94490=CARTESIAN_POINT('Ctrl Pts',(-1.65566521381503,-1.6982501543112,13.9733523529318));
#94491=CARTESIAN_POINT('Ctrl Pts',(-1.66216961300225,-1.69188447336643,
13.9727451194643));
#94492=CARTESIAN_POINT('Ctrl Pts',(-1.69213134149449,-1.66222217062738,
13.9699445903256));
#94493=CARTESIAN_POINT('Ctrl Pts',(-1.71513794421006,-1.63847280366575,
13.9677844641144));
#94494=CARTESIAN_POINT('Ctrl Pts',(-1.7789945197234,-1.56973503185522,13.961733322715));
#94495=CARTESIAN_POINT('Ctrl Pts',(-1.81862460942257,-1.52364536535424,
13.9579100832205));
#94496=CARTESIAN_POINT('Ctrl Pts',(-1.91222348598784,-1.40592757866267,
13.9485616066458));
#94497=CARTESIAN_POINT('Ctrl Pts',(-1.96398375717597,-1.33266642323371,
13.9430964747904));
#94498=CARTESIAN_POINT('Ctrl Pts',(-2.09559796324398,-1.12199622193867,
13.9278625780495));
#94499=CARTESIAN_POINT('Ctrl Pts',(-2.16597593315566,-0.979257059794558,
13.9180382995999));
#94500=CARTESIAN_POINT('Ctrl Pts',(-2.2281211920225,-0.813034130090632,
13.906450319185));
#94501=CARTESIAN_POINT('Ctrl Pts',(-2.23446918232746,-0.79542189007037,
13.9052212695859));
#94502=CARTESIAN_POINT('Ctrl Pts',(-2.24444554133774,-0.766680663226114,
13.9032126840807));
#94503=CARTESIAN_POINT('Ctrl Pts',(-2.2482012725681,-0.755596490921561,
13.9024373691801));
#94504=CARTESIAN_POINT('Ctrl Pts',(-2.25475060810512,-0.735786446979471,
13.9010502513684));
#94505=CARTESIAN_POINT('Ctrl Pts',(-2.25757599386896,-0.727071267594697,
13.9004395106939));
#94506=CARTESIAN_POINT('Ctrl Pts',(-2.26343555747647,-0.70863338523543,
13.8991462741429));
#94507=CARTESIAN_POINT('Ctrl Pts',(-2.26645773538514,-0.698907093689615,
13.8984633981684));
#94508=CARTESIAN_POINT('Ctrl Pts',(-2.2743273041869,-0.672992518790541,
13.8966420101112));
#94509=CARTESIAN_POINT('Ctrl Pts',(-2.27906441647683,-0.656771632021285,
13.8954999239152));
#94510=CARTESIAN_POINT('Ctrl Pts',(-2.28905978403994,-0.621134424448397,
13.8929858820058));
#94511=CARTESIAN_POINT('Ctrl Pts',(-2.29424512680767,-0.601699196310096,
13.8916116620672));
#94512=CARTESIAN_POINT('Ctrl Pts',(-2.34755169363489,-0.391185040414472,
13.8766899946634));
#94513=CARTESIAN_POINT('Ctrl Pts',(-2.37191673355796,-0.194929333901108,
13.8623564033571));
#94514=CARTESIAN_POINT('Ctrl Pts',(-2.37174914129228,0.00201823668619566,
13.8479759907678));
#94515=CARTESIAN_POINT('Ctrl Pts',(-2.3717491398467,0.00201993475696598,
13.8479758667807));
#94516=CARTESIAN_POINT('Ctrl Pts',(-2.37170051413794,0.0591148396921598,
13.8438069996322));
#94517=CARTESIAN_POINT('Ctrl Pts',(-2.36959025382119,0.116171024686506,
13.8396487900764));
#94518=CARTESIAN_POINT('Ctrl Pts',(-2.36542648366643,0.173076898716907,
13.8355365560746));
#94519=CARTESIAN_POINT('Ctrl Pts',(-2.3654265016339,0.173076653156924,13.6406850658798));
#94520=CARTESIAN_POINT('Ctrl Pts',(-2.36966457379971,0.115155217573458,
13.644911151959));
#94521=CARTESIAN_POINT('Ctrl Pts',(-2.37177512500354,0.0570791205575195,
13.6491130294797));
#94522=CARTESIAN_POINT('Ctrl Pts',(-2.37172935718148,-0.0478396125883249,
13.6565829838009));
#94523=CARTESIAN_POINT('Ctrl Pts',(-2.37032343645748,-0.0946377349083146,
13.6598712536482));
#94524=CARTESIAN_POINT('Ctrl Pts',(-2.36689050219465,-0.152130446883851,
13.6638337330577));
#94525=CARTESIAN_POINT('Ctrl Pts',(-2.36617441736504,-0.162889410416478,
13.6645719125626));
#94526=CARTESIAN_POINT('Ctrl Pts',(-2.36493924025131,-0.179715099442791,
13.6657207145778));
#94527=CARTESIAN_POINT('Ctrl Pts',(-2.3644701304286,-0.185785175629894,
13.6661340136292));
#94528=CARTESIAN_POINT('Ctrl Pts',(-2.36355760519669,-0.197029117735796,
13.6668973842094));
#94529=CARTESIAN_POINT('Ctrl Pts',(-2.36312057520462,-0.202203299316896,
13.6672477923236));
#94530=CARTESIAN_POINT('Ctrl Pts',(-2.36208715259719,-0.213977231921002,
13.6680431921905));
#94531=CARTESIAN_POINT('Ctrl Pts',(-2.3614800929295,-0.220575940759209,
13.6684875822957));
#94532=CARTESIAN_POINT('Ctrl Pts',(-2.35953359855696,-0.240804533255232,
13.6698458449916));
#94533=CARTESIAN_POINT('Ctrl Pts',(-2.35810372875169,-0.254425730819577,
13.6707548317141));
#94534=CARTESIAN_POINT('Ctrl Pts',(-2.34195580645491,-0.396398228956341,
13.6801776474902));
#94535=CARTESIAN_POINT('Ctrl Pts',(-2.31688950310181,-0.523375281919996,
13.6881719460958));
#94536=CARTESIAN_POINT('Ctrl Pts',(-2.2285869977464,-0.834434008675452,
13.7080289441977));
#94537=CARTESIAN_POINT('Ctrl Pts',(-2.15285929837325,-1.01393675689906,
13.7197985919894));
#94538=CARTESIAN_POINT('Ctrl Pts',(-2.04214817680727,-1.20648818887445,
13.7342085859765));
#94539=CARTESIAN_POINT('Ctrl Pts',(-2.02775514984024,-1.23052503816858,
13.7360404491905));
#94540=CARTESIAN_POINT('Ctrl Pts',(-2.00638914573541,-1.264813862083,13.7387045862844));
#94541=CARTESIAN_POINT('Ctrl Pts',(-1.99975591654114,-1.27527556797241,
13.739524408507));
#94542=CARTESIAN_POINT('Ctrl Pts',(-1.98794671867997,-1.29358193641776,
13.7409715542617));
#94543=CARTESIAN_POINT('Ctrl Pts',(-1.98280546421823,-1.30144875782308,
13.7415975772099));
#94544=CARTESIAN_POINT('Ctrl Pts',(-1.97209829610196,-1.3176214698184,13.7428932510633));
#94545=CARTESIAN_POINT('Ctrl Pts',(-1.96652635202759,-1.32592312321959,
13.7435631200061));
#94546=CARTESIAN_POINT('Ctrl Pts',(-1.95211521315318,-1.3471036525959,13.7452846556922));
#94547=CARTESIAN_POINT('Ctrl Pts',(-1.9432010906199,-1.35993071783013,13.7463391489692));
#94548=CARTESIAN_POINT('Ctrl Pts',(-1.90522215232671,-1.41344501007247,
13.750789659394));
#94549=CARTESIAN_POINT('Ctrl Pts',(-1.87500303290319,-1.45329323090714,
13.7542297327448));
#94550=CARTESIAN_POINT('Ctrl Pts',(-1.79105035094229,-1.55701635136388,
13.7635355813404));
#94551=CARTESIAN_POINT('Ctrl Pts',(-1.73517031334781,-1.61905612310837,
13.769479917436));
#94552=CARTESIAN_POINT('Ctrl Pts',(-1.57640700866631,-1.77764206181256,
13.785688000691));
#94553=CARTESIAN_POINT('Ctrl Pts',(-1.46799220459803,-1.86817222551871,
13.7960863576813));
#94554=CARTESIAN_POINT('Ctrl Pts',(-1.34017759356799,-1.95686882643037,
13.8073067641497));
#94555=CARTESIAN_POINT('Ctrl Pts',(-1.32809564159908,-1.96508869180668,
13.8083576929742));
#94556=CARTESIAN_POINT('Ctrl Pts',(-1.26740415344156,-2.00556426229297,
13.8135861126565));
#94557=CARTESIAN_POINT('Ctrl Pts',(-1.21768743619563,-2.03613357035258,
13.8177085258715));
#94558=CARTESIAN_POINT('Ctrl Pts',(-1.15776327057873,-2.06999810524921,
13.8224493601109));
#94559=CARTESIAN_POINT('Ctrl Pts',(-1.14860287686701,-2.0750950310417,13.8231679579305));
#94560=CARTESIAN_POINT('Ctrl Pts',(-1.13363832825468,-2.08329198435553,
13.8243315822279));
#94561=CARTESIAN_POINT('Ctrl Pts',(-1.12785465845747,-2.08642882059846,
13.8247788324008));
#94562=CARTESIAN_POINT('Ctrl Pts',(-1.11748611907309,-2.09199659765284,
13.8255761013129));
#94563=CARTESIAN_POINT('Ctrl Pts',(-1.11290626928374,-2.09443658974088,
13.825926682421));
#94564=CARTESIAN_POINT('Ctrl Pts',(-1.10290463074564,-2.09972306119919,
13.8266888512001));
#94565=CARTESIAN_POINT('Ctrl Pts',(-1.0974798205337,-2.10256357904415,13.8271000636115));
#94566=CARTESIAN_POINT('Ctrl Pts',(-1.08206051738724,-2.11056143815232,
13.8282628780939));
#94567=CARTESIAN_POINT('Ctrl Pts',(-1.07204008918079,-2.11566883211694,
13.8290114247087));
#94568=CARTESIAN_POINT('Ctrl Pts',(-1.00647277428633,-2.14850291705219,
13.8338656536168));
#94569=CARTESIAN_POINT('Ctrl Pts',(-0.949886281574112,-2.17411357609958,
13.8378512926677));
#94570=CARTESIAN_POINT('Ctrl Pts',(-0.712166110121094,-2.27064733874149,
13.8540305809719));
#94571=CARTESIAN_POINT('Ctrl Pts',(-0.523656570790738,-2.32138177587498,
13.8656016084419));
#94572=CARTESIAN_POINT('Ctrl Pts',(-0.247210885606719,-2.36035056584702,
13.8830816645218));
#94573=CARTESIAN_POINT('Ctrl Pts',(-0.162800041479565,-2.36767009865302,
13.8884753678646));
#94574=CARTESIAN_POINT('Ctrl Pts',(-0.059160299622568,-2.37108845385537,
13.8952572092189));
#94575=CARTESIAN_POINT('Ctrl Pts',(-0.040129167633956,-2.37148687790052,
13.8965089538415));
#94576=CARTESIAN_POINT('Ctrl Pts',(-0.0102364215921659,-2.37175277221655,
13.898486066871));
#94577=CARTESIAN_POINT('Ctrl Pts',(0.000623285463821417,-2.37177477887079,
13.8992066001961));
#94578=CARTESIAN_POINT('Ctrl Pts',(0.0197974813912066,-2.3716819476805,
13.9004829619631));
#94579=CARTESIAN_POINT('Ctrl Pts',(0.0281119919635066,-2.37159796637159,
13.9010378148921));
#94580=CARTESIAN_POINT('Ctrl Pts',(0.047180535766741,-2.37130507341475,
13.9023135755977));
#94581=CARTESIAN_POINT('Ctrl Pts',(0.0579338676865814,-2.37106672502296,
13.9030353934356));
#94582=CARTESIAN_POINT('Ctrl Pts',(0.0877606907639155,-2.37020258817421,
13.9050443099736));
#94583=CARTESIAN_POINT('Ctrl Pts',(0.106828458096183,-2.36941973723284,
13.9063362875109));
#94584=CARTESIAN_POINT('Ctrl Pts',(0.222176638545932,-2.36328881586511,
13.9142005031177));
#94585=CARTESIAN_POINT('Ctrl Pts',(0.318054111611235,-2.35230389036165,
13.9209477537216));
#94586=CARTESIAN_POINT('Ctrl Pts',(0.531147861862907,-2.31462279841012,
13.9364134428607));
#94587=CARTESIAN_POINT('Ctrl Pts',(0.647545781603016,-2.28479260502635,
13.945192635216));
#94588=CARTESIAN_POINT('Ctrl Pts',(0.802775677621637,-2.23219139276793,
13.9571550318187));
#94589=CARTESIAN_POINT('Ctrl Pts',(0.84397564744979,-2.21694214842574,13.9603540510164));
#94590=CARTESIAN_POINT('Ctrl Pts',(0.910913774851806,-2.19002982029117,
13.9655713055385));
#94591=CARTESIAN_POINT('Ctrl Pts',(0.936909144820054,-2.17903553689865,
13.9676023942615));
#94592=CARTESIAN_POINT('Ctrl Pts',(1.01089740585605,-2.14617459354204,13.9733869774753));
#94593=CARTESIAN_POINT('Ctrl Pts',(1.05836916996301,-2.12316618589423,13.9771031277693));
#94594=CARTESIAN_POINT('Ctrl Pts',(1.11405345074896,-2.09384497518342,13.9814355002175));
#94595=CARTESIAN_POINT('Ctrl Pts',(1.12303818682076,-2.08903975824558,13.9821336770231));
#94596=CARTESIAN_POINT('Ctrl Pts',(1.13769516450775,-2.08107902255819,13.9832708783125));
#94597=CARTESIAN_POINT('Ctrl Pts',(1.14338579832841,-2.07795791685341,13.9837119666306));
#94598=CARTESIAN_POINT('Ctrl Pts',(1.15359886543818,-2.07230176302125,13.9845027128586));
#94599=CARTESIAN_POINT('Ctrl Pts',(1.15812583862474,-2.06977522520621,13.9848528930264));
#94600=CARTESIAN_POINT('Ctrl Pts',(1.16804444653797,-2.06419684486427,13.9856194312944));
#94601=CARTESIAN_POINT('Ctrl Pts',(1.17343241463426,-2.06113871778308,13.9860353807317));
#94602=CARTESIAN_POINT('Ctrl Pts',(1.18885974669095,-2.0523023021538,13.9872252603883));
#94603=CARTESIAN_POINT('Ctrl Pts',(1.19886902156877,-2.04647143138223,13.9879959063456));
#94604=CARTESIAN_POINT('Ctrl Pts',(1.26929495451525,-2.00475099307711,13.9934115952644));
#94605=CARTESIAN_POINT('Ctrl Pts',(1.32813966426015,-1.96626128218342,13.9979023549912));
#94606=CARTESIAN_POINT('Ctrl Pts',(1.47607317349681,-1.85982275403718,14.0093377579817));
#94607=CARTESIAN_POINT('Ctrl Pts',(1.56221309223093,-1.78807873119548,14.0161484865857));
#94608=CARTESIAN_POINT('Ctrl Pts',(1.75498516215986,-1.60291926916756,14.0325483822515));
#94609=CARTESIAN_POINT('Ctrl Pts',(1.85614783840731,-1.48459708184752,14.0421717709329));
#94610=CARTESIAN_POINT('Ctrl Pts',(1.95584498697376,-1.34172526429564,14.0535457806605));
#94611=CARTESIAN_POINT('Ctrl Pts',(1.96648967377802,-1.32607489484814,14.0547881670264));
#94612=CARTESIAN_POINT('Ctrl Pts',(1.98349343488059,-1.30042005766958,14.0568199828052));
#94613=CARTESIAN_POINT('Ctrl Pts',(1.98996696023742,-1.29049216236725,14.0576051122212));
#94614=CARTESIAN_POINT('Ctrl Pts',(2.00138272293743,-1.2726946248536,14.0590107891905));
#94615=CARTESIAN_POINT('Ctrl Pts',(2.00635366715774,-1.26484361478456,14.0596302535283));
#94616=CARTESIAN_POINT('Ctrl Pts',(2.01676152848103,-1.24818990740811,14.060943076362));
#94617=CARTESIAN_POINT('Ctrl Pts',(2.02218722478593,-1.23938046206231,14.0616368317503));
#94618=CARTESIAN_POINT('Ctrl Pts',(2.03648261687629,-1.21582593288236,14.0634900964053));
#94619=CARTESIAN_POINT('Ctrl Pts',(2.04524964132078,-1.20101957741495,14.064653316954));
#94620=CARTESIAN_POINT('Ctrl Pts',(2.08723526069181,-1.12831833712147,14.0703576034991));
#94621=CARTESIAN_POINT('Ctrl Pts',(2.11815785997799,-1.06913939433806,14.0749798181684));
#94622=CARTESIAN_POINT('Ctrl Pts',(2.25892586895362,-0.769593095637562,
14.0982922301832));
#94623=CARTESIAN_POINT('Ctrl Pts',(2.33053601419852,-0.513404003847887,
14.118239039586));
#94624=CARTESIAN_POINT('Ctrl Pts',(2.36063813866413,-0.230238550375794,
14.1380825608457));
#94625=CARTESIAN_POINT('Ctrl Pts',(2.36254848089642,-0.209730683584838,
14.139505995642));
#94626=CARTESIAN_POINT('Ctrl Pts',(2.36483339902296,-0.181178922373827,
14.1414663644167));
#94627=CARTESIAN_POINT('Ctrl Pts',(2.3654344688001,-0.173154802515619,14.1420149567927));
#94628=CARTESIAN_POINT('Ctrl Pts',(2.3663346520844,-0.16025672573131,14.1428928391608));
#94629=CARTESIAN_POINT('Ctrl Pts',(2.36665956412127,-0.155384724031287,
14.1432235416347));
#94630=CARTESIAN_POINT('Ctrl Pts',(2.36731047923859,-0.145148335667127,
14.1439164281146));
#94631=CARTESIAN_POINT('Ctrl Pts',(2.36763329863732,-0.139783792202878,
14.14427842293));
#94632=CARTESIAN_POINT('Ctrl Pts',(2.36838064539985,-0.126618377415897,
14.1451641573322));
#94633=CARTESIAN_POINT('Ctrl Pts',(2.36878487420083,-0.118816325087629,
14.1456867722255));
#94634=CARTESIAN_POINT('Ctrl Pts',(2.37011642340545,-0.0903992837354115,
14.1475824090917));
#94635=CARTESIAN_POINT('Ctrl Pts',(2.37081327721885,-0.0697736875681348,
14.1489432445272));
#94636=CARTESIAN_POINT('Ctrl Pts',(2.37188331454646,-0.0181400520376521,
14.1523181759893));
#94637=CARTESIAN_POINT('Ctrl Pts',(2.37191779587942,0.0128718786578912,
14.1543165864761));
#94638=CARTESIAN_POINT('Ctrl Pts',(2.36941773202961,0.147988169915104,14.162933242687));
#94639=CARTESIAN_POINT('Ctrl Pts',(2.36063695498753,0.251868279889686,14.1693278314723));
#94640=CARTESIAN_POINT('Ctrl Pts',(2.31866693835288,0.52923672758063,14.1865246601909));
#94641=CARTESIAN_POINT('Ctrl Pts',(2.2729120859637,0.70012086871169,14.1972930113968));
#94642=CARTESIAN_POINT('Ctrl Pts',(2.19821194557041,0.891000306396194,14.2105780377398));
#94643=CARTESIAN_POINT('Ctrl Pts',(2.18729972532151,0.917462315212398,14.212447972789));
#94644=CARTESIAN_POINT('Ctrl Pts',(2.17126484298643,0.954433564496448,14.2151035558771));
#94645=CARTESIAN_POINT('Ctrl Pts',(2.16653900995932,0.965113028371262,14.2158757639341));
#94646=CARTESIAN_POINT('Ctrl Pts',(2.15816690414544,0.983660956411467,14.2172260833561));
#94647=CARTESIAN_POINT('Ctrl Pts',(2.15455595845984,0.991545199052107,14.2178029771567));
#94648=CARTESIAN_POINT('Ctrl Pts',(2.14690485117357,1.00801170579069,14.2190140357177));
#94649=CARTESIAN_POINT('Ctrl Pts',(2.14285628664316,1.01658987270027,14.2196484823327));
#94650=CARTESIAN_POINT('Ctrl Pts',(2.1330869789981,1.03697157651888,14.2211645314235));
#94651=CARTESIAN_POINT('Ctrl Pts',(2.12731961226386,1.04875228996633,14.2220477411484));
#94652=CARTESIAN_POINT('Ctrl Pts',(2.10738008880033,1.08864047880309,14.2250622293253));
#94653=CARTESIAN_POINT('Ctrl Pts',(2.09274673920698,1.11651235998425,14.2272095485095));
#94654=CARTESIAN_POINT('Ctrl Pts',(2.05625844217895,1.18277216527265,14.2324162665376));
#94655=CARTESIAN_POINT('Ctrl Pts',(2.03387799618965,1.22085569833873,14.2354934070591));
#94656=CARTESIAN_POINT('Ctrl Pts',(1.87647056231414,1.47235536034209,14.2563930289056));
#94657=CARTESIAN_POINT('Ctrl Pts',(1.70919853806817,1.66360390189591,14.2753854692238));
#94658=CARTESIAN_POINT('Ctrl Pts',(1.49224228499878,1.8437141140417,14.2952045663636));
#94659=CARTESIAN_POINT('Ctrl Pts',(1.46918737457923,1.86213786585103,14.2972569078472));
#94660=CARTESIAN_POINT('Ctrl Pts',(1.43843797136571,1.88578375186439,14.2999181776973));
#94661=CARTESIAN_POINT('Ctrl Pts',(1.43104932214785,1.8913968386014,14.3005520059972));
#94662=CARTESIAN_POINT('Ctrl Pts',(1.41907576647131,1.90038270420443,14.3015698368535));
#94663=CARTESIAN_POINT('Ctrl Pts',(1.41451142132369,1.90378252280043,14.3019556750205));
#94664=CARTESIAN_POINT('Ctrl Pts',(1.40567983835459,1.91031155952172,14.30269800569));
#94665=CARTESIAN_POINT('Ctrl Pts',(1.40141433651535,1.91344294933466,14.3030546405708));
#94666=CARTESIAN_POINT('Ctrl Pts',(1.39118165717928,1.92090239138944,14.3039057371428));
#94667=CARTESIAN_POINT('Ctrl Pts',(1.38520464911514,1.92521699666826,14.3043992754068));
#94668=CARTESIAN_POINT('Ctrl Pts',(1.36470591753941,1.93986947140268,14.3060800313433));
#94669=CARTESIAN_POINT('Ctrl Pts',(1.35008737526894,1.95007177658532,14.3072583950441));
#94670=CARTESIAN_POINT('Ctrl Pts',(1.26350144619314,2.00905979365591,14.3141286784368));
#94671=CARTESIAN_POINT('Ctrl Pts',(1.18900227582438,2.0540287801548,14.319602481301));
#94672=CARTESIAN_POINT('Ctrl Pts',(0.995076054717052,2.15698973129651,14.3332156831375));
#94673=CARTESIAN_POINT('Ctrl Pts',(0.872949852459632,2.20923986455133,14.3412319294453));
#94674=CARTESIAN_POINT('Ctrl Pts',(0.643215935716809,2.28548700906873,14.3562384353388));
#94675=CARTESIAN_POINT('Ctrl Pts',(0.537087793350325,2.31272773709725,14.36314295956));
#94676=CARTESIAN_POINT('Ctrl Pts',(0.411379412146523,2.33587313487773,14.3714927976255));
#94677=CARTESIAN_POINT('Ctrl Pts',(0.393253895013062,2.33899287422973,14.3727005816301));
#94678=CARTESIAN_POINT('Ctrl Pts',(0.363550954485634,2.34375029259329,14.3746869603661));
#94679=CARTESIAN_POINT('Ctrl Pts',(0.351994236397848,2.34551375604328,14.3754615723831));
#94680=CARTESIAN_POINT('Ctrl Pts',(0.331245860438416,2.34852299834729,14.3768556327467));
#94681=CARTESIAN_POINT('Ctrl Pts',(0.322058977913698,2.34980043926408,14.3774740667892));
#94682=CARTESIAN_POINT('Ctrl Pts',(0.302513957564566,2.35240141311723,14.3787923912539));
#94683=CARTESIAN_POINT('Ctrl Pts',(0.292154127870092,2.35371048824434,14.3794927242597));
#94684=CARTESIAN_POINT('Ctrl Pts',(0.264267093188859,2.35704736420197,14.381382265363));
#94685=CARTESIAN_POINT('Ctrl Pts',(0.246725633312908,2.35894802954989,14.3825754446634));
#94686=CARTESIAN_POINT('Ctrl Pts',(0.15707990474941,2.36765056481396,14.3886980409045));
#94687=CARTESIAN_POINT('Ctrl Pts',(0.0847196167827616,2.37134222044782,
14.3937237446156));
#94688=CARTESIAN_POINT('Ctrl Pts',(-0.134262270104153,2.37247881922378,
14.4091955977359));
#94689=CARTESIAN_POINT('Ctrl Pts',(-0.280575212756807,2.35965048353693,
14.419910802823));
#94690=CARTESIAN_POINT('Ctrl Pts',(-0.468946857367222,2.32536128257686,
14.4338853130459));
#94691=CARTESIAN_POINT('Ctrl Pts',(-0.512908408510258,2.3160616159789,14.4371572283274));
#94692=CARTESIAN_POINT('Ctrl Pts',(-0.581529844257104,2.29949556719929,
14.4422605982404));
#94693=CARTESIAN_POINT('Ctrl Pts',(-0.606380742568676,2.29306765961788,
14.4441078930283));
#94694=CARTESIAN_POINT('Ctrl Pts',(-0.683384407995395,2.27181055486915,
14.4498205558896));
#94695=CARTESIAN_POINT('Ctrl Pts',(-0.735140690732121,2.25559453136196,
14.4536439835678));
#94696=CARTESIAN_POINT('Ctrl Pts',(-0.795990193165919,2.23421197956844,
14.4580847105894));
#94697=CARTESIAN_POINT('Ctrl Pts',(-0.805658383572585,2.23074385258039,
14.4587886124511));
#94698=CARTESIAN_POINT('Ctrl Pts',(-0.821422215508404,2.22497327076715,
14.4599332274704));
#94699=CARTESIAN_POINT('Ctrl Pts',(-0.827531313759111,2.22270835673344,
14.4603760487772));
#94700=CARTESIAN_POINT('Ctrl Pts',(-0.838485721216621,2.21859564751026,
14.4611686165873));
#94701=CARTESIAN_POINT('Ctrl Pts',(-0.843334351121684,2.21675711923979,
14.4615188966555));
#94702=CARTESIAN_POINT('Ctrl Pts',(-0.853943095538841,2.21269459587971,
14.4622841480391));
#94703=CARTESIAN_POINT('Ctrl Pts',(-0.859700562199524,2.21046400798772,
14.4626987203466));
#94704=CARTESIAN_POINT('Ctrl Pts',(-0.875460544566788,2.20428730354226,
14.4638316840239));
#94705=CARTESIAN_POINT('Ctrl Pts',(-0.885445192195174,2.2002955492857,14.4645474170893));
#94706=CARTESIAN_POINT('Ctrl Pts',(-0.947733503854984,2.17490068427505,
14.4690016842843));
#94707=CARTESIAN_POINT('Ctrl Pts',(-0.999290213896659,2.15169980659951,
14.4726409659885));
#94708=CARTESIAN_POINT('Ctrl Pts',(-1.18811724292918,2.05847297487345,14.4859683619522));
#94709=CARTESIAN_POINT('Ctrl Pts',(-1.31929619942623,1.97696690645317,14.4952443636338));
#94710=CARTESIAN_POINT('Ctrl Pts',(-1.54326762172838,1.80551938044957,14.5126353675754));
#94711=CARTESIAN_POINT('Ctrl Pts',(-1.63840951236473,1.71964609756744,14.5206497801449));
#94712=CARTESIAN_POINT('Ctrl Pts',(-1.73910170620789,1.61278633154561,14.5302359856086));
#94713=CARTESIAN_POINT('Ctrl Pts',(-1.75188422874247,1.59889215114501,14.5314752911328));
#94714=CARTESIAN_POINT('Ctrl Pts',(-1.77240937881996,1.57604035072261,14.5335030644104));
#94715=CARTESIAN_POINT('Ctrl Pts',(-1.78025336842764,1.5671745687165,14.5342872608593));
#94716=CARTESIAN_POINT('Ctrl Pts',(-1.79413465132423,1.55124634881878,14.5356919008291));
#94717=CARTESIAN_POINT('Ctrl Pts',(-1.80019747645138,1.54420640568578,14.5363112672532));
#94718=CARTESIAN_POINT('Ctrl Pts',(-1.81292940103184,1.52924565167884,14.5376245465101));
#94719=CARTESIAN_POINT('Ctrl Pts',(-1.81958828912588,1.52131644587139,14.5383188601581));
#94720=CARTESIAN_POINT('Ctrl Pts',(-1.83302885559845,1.505097334645,14.5397357113136));
#94721=CARTESIAN_POINT('Ctrl Pts',(-1.83980672100949,1.49680459478574,14.5404583815303));
#94722=CARTESIAN_POINT('Ctrl Pts',(-1.86937641212722,1.46012169275235,14.543647684254));
#94723=CARTESIAN_POINT('Ctrl Pts',(-1.89156788338949,1.43125616641486,14.5461380332027));
#94724=CARTESIAN_POINT('Ctrl Pts',(-1.97444070443029,1.31816422367882,14.5558275416721));
#94725=CARTESIAN_POINT('Ctrl Pts',(-2.03022535633471,1.23050922521842,14.5632045645012));
#94726=CARTESIAN_POINT('Ctrl Pts',(-2.12246910352673,1.06212311878316,14.5770860797305));
#94727=CARTESIAN_POINT('Ctrl Pts',(-2.16050237637178,0.982450584953549,
14.5835433171297));
#94728=CARTESIAN_POINT('Ctrl Pts',(-2.19603182186104,0.895918909124036,
14.5903691788301));
#94729=CARTESIAN_POINT('Ctrl Pts',(-2.19803906419902,0.890983011506573,
14.5907578938943));
#94730=CARTESIAN_POINT('Ctrl Pts',(-2.24290862879087,0.779572318830626,
14.599516865991));
#94731=CARTESIAN_POINT('Ctrl Pts',(-2.27800801630554,0.670118036919324,
14.6078232415036));
#94732=CARTESIAN_POINT('Ctrl Pts',(-2.30805192076658,0.54612952360223,14.6166270141927));
#94733=CARTESIAN_POINT('Ctrl Pts',(-2.3109589341186,0.533694621089315,14.6175032510949));
#94734=CARTESIAN_POINT('Ctrl Pts',(-2.31519982540412,0.514869332193258,
14.6188190701366));
#94735=CARTESIAN_POINT('Ctrl Pts',(-2.31660793141405,0.50849617057809,14.6192626807328));
#94736=CARTESIAN_POINT('Ctrl Pts',(-2.31908766683348,0.497048641077518,
14.6200560816172));
#94737=CARTESIAN_POINT('Ctrl Pts',(-2.32016897311292,0.491976519688363,
14.6204064106129));
#94738=CARTESIAN_POINT('Ctrl Pts',(-2.32249929460377,0.480867025753907,
14.6211710913307));
#94739=CARTESIAN_POINT('Ctrl Pts',(-2.32374140893419,0.474828323174784,
14.6215850483729));
#94740=CARTESIAN_POINT('Ctrl Pts',(-2.32626218594874,0.462326411442523,
14.622438689942));
#94741=CARTESIAN_POINT('Ctrl Pts',(-2.32753749432764,0.455862570897453,
14.6228781862929));
#94742=CARTESIAN_POINT('Ctrl Pts',(-2.33075883786171,0.439169359076368,
14.624008610313));
#94743=CARTESIAN_POINT('Ctrl Pts',(-2.3326644972697,0.428932207759946,14.6246973978613));
#94744=CARTESIAN_POINT('Ctrl Pts',(-2.3490847332647,0.33737577802246,14.6308206249047));
#94745=CARTESIAN_POINT('Ctrl Pts',(-2.359403337115,0.255394829345939,14.6360441351265));
#94746=CARTESIAN_POINT('Ctrl Pts',(-2.3654265029177,0.173076635611311,14.6411792785331));
#94747=CARTESIAN_POINT('Origin',(0.,0.,-1.84858989190503));
#94748=CARTESIAN_POINT('',(-2.3654264678378,0.1730771150452,15.8377719611872));
#94749=CARTESIAN_POINT('',(-2.36542649459319,0.173076749381846,15.6377659025437));
#94750=CARTESIAN_POINT('',(-2.36542649454111,0.173076750093529,-1.84858989190503));
#94751=CARTESIAN_POINT('Ctrl Pts',(-2.3654264678378,0.173077115045235,15.8377719611872));
#94752=CARTESIAN_POINT('Ctrl Pts',(-2.35693967585688,0.289065195696194,
15.8305839026341));
#94753=CARTESIAN_POINT('Ctrl Pts',(-2.33992823301383,0.404345136771074,
15.8232718114111));
#94754=CARTESIAN_POINT('Ctrl Pts',(-2.31108949090406,0.53320410740175,15.8146601565345));
#94755=CARTESIAN_POINT('Ctrl Pts',(-2.30753370920037,0.548388016895403,
15.8136385787627));
#94756=CARTESIAN_POINT('Ctrl Pts',(-2.30133322390988,0.573736651875055,
15.8119210921138));
#94757=CARTESIAN_POINT('Ctrl Pts',(-2.29877023651474,0.583921010869794,
15.8112277894557));
#94758=CARTESIAN_POINT('Ctrl Pts',(-2.29359273599811,0.603931963977296,
15.8098589241349));
#94759=CARTESIAN_POINT('Ctrl Pts',(-2.29098249745076,0.613759437086357,
15.8091835117595));
#94760=CARTESIAN_POINT('Ctrl Pts',(-2.28589948284066,0.632412538950499,
15.8078953905436));
#94761=CARTESIAN_POINT('Ctrl Pts',(-2.28343857822489,0.641241234226451,
15.8072830775913));
#94762=CARTESIAN_POINT('Ctrl Pts',(-2.27771063661152,0.661339545219483,
15.8058830408649));
#94763=CARTESIAN_POINT('Ctrl Pts',(-2.2744110386623,0.672599551586081,15.8050942677294));
#94764=CARTESIAN_POINT('Ctrl Pts',(-2.26560116083366,0.701857335075098,
15.8030330069283));
#94765=CARTESIAN_POINT('Ctrl Pts',(-2.25996003422465,0.719814522468014,
15.8017562720134));
#94766=CARTESIAN_POINT('Ctrl Pts',(-2.21024647093929,0.871718140942521,
15.7908547256863));
#94767=CARTESIAN_POINT('Ctrl Pts',(-2.15453125049659,1.00153079454575,15.7808399903655));
#94768=CARTESIAN_POINT('Ctrl Pts',(-2.04450575896787,1.20559174738188,15.7640162710425));
#94769=CARTESIAN_POINT('Ctrl Pts',(-1.99681957150012,1.28303014012067,15.7573529274218));
#94770=CARTESIAN_POINT('Ctrl Pts',(-1.88674710256206,1.44071984064076,15.7433513047515));
#94771=CARTESIAN_POINT('Ctrl Pts',(-1.8234004910064,1.52009995544995,15.7360382966012));
#94772=CARTESIAN_POINT('Ctrl Pts',(-1.75095360765454,1.59981204851793,15.7285892357328));
#94773=CARTESIAN_POINT('Ctrl Pts',(-1.74673157937264,1.6044207423317,15.7281581727187));
#94774=CARTESIAN_POINT('Ctrl Pts',(-1.73566036220545,1.61641039241845,15.7270358711188));
#94775=CARTESIAN_POINT('Ctrl Pts',(-1.72878220297823,1.62376462377793,15.7263465951686));
#94776=CARTESIAN_POINT('Ctrl Pts',(-1.7176602860957,1.63550556362733,15.7252450803992));
#94777=CARTESIAN_POINT('Ctrl Pts',(-1.71344616346962,1.63991998405933,15.7248306753802));
#94778=CARTESIAN_POINT('Ctrl Pts',(-1.70567236417713,1.64800059440189,15.7240717245548));
#94779=CARTESIAN_POINT('Ctrl Pts',(-1.70211789127296,1.65167153463199,15.7237268034905));
#94780=CARTESIAN_POINT('Ctrl Pts',(-1.69408838784669,1.65991068693467,15.7229523206187));
#94781=CARTESIAN_POINT('Ctrl Pts',(-1.68960673712148,1.66447229798099,15.7225232846837));
#94782=CARTESIAN_POINT('Ctrl Pts',(-1.67804747571868,1.67614300117668,15.721424805646));
#94783=CARTESIAN_POINT('Ctrl Pts',(-1.67094302487153,1.68322550706881,15.7207574039355));
#94784=CARTESIAN_POINT('Ctrl Pts',(-1.62705657986959,1.72642469899635,15.7166801761862));
#94785=CARTESIAN_POINT('Ctrl Pts',(-1.58914698497829,1.76138245492169,15.7133527406003));
#94786=CARTESIAN_POINT('Ctrl Pts',(-1.54436194322092,1.80005617340974,15.7095964739088));
#94787=CARTESIAN_POINT('Ctrl Pts',(-1.53857505434597,1.80500494278887,15.7091143350526));
#94788=CARTESIAN_POINT('Ctrl Pts',(-1.52140360789928,1.81954685459245,15.7076928393277));
#94789=CARTESIAN_POINT('Ctrl Pts',(-1.50995231200316,1.82906088592689,15.7067566661975));
#94790=CARTESIAN_POINT('Ctrl Pts',(-1.33517647980236,1.97150905594866,15.6926326741816));
#94791=CARTESIAN_POINT('Ctrl Pts',(-1.15495184694935,2.08221938959674,15.6801328847443));
#94792=CARTESIAN_POINT('Ctrl Pts',(-0.925112102712844,2.18427022318138,
15.6641893985041));
#94793=CARTESIAN_POINT('Ctrl Pts',(-0.887333449476023,2.19988814815114,
15.6615723000295));
#94794=CARTESIAN_POINT('Ctrl Pts',(-0.821753787069529,2.22503506808374,
15.6570213946533));
#94795=CARTESIAN_POINT('Ctrl Pts',(-0.794144014606266,2.23503814287156,
15.6551031045542));
#94796=CARTESIAN_POINT('Ctrl Pts',(-0.754265995440895,2.24865384066947,
15.6523258184863));
#94797=CARTESIAN_POINT('Ctrl Pts',(-0.74214242667253,2.25268415335576,15.6514806185523));
#94798=CARTESIAN_POINT('Ctrl Pts',(-0.72111704641421,2.25948560044177,15.650013071375));
#94799=CARTESIAN_POINT('Ctrl Pts',(-0.712230277849712,2.26230258813555,
15.6493922472451));
#94800=CARTESIAN_POINT('Ctrl Pts',(-0.695133338765421,2.26761136822035,
15.6481967313869));
#94801=CARTESIAN_POINT('Ctrl Pts',(-0.686925786584785,2.27011115065228,
15.6476223129959));
#94802=CARTESIAN_POINT('Ctrl Pts',(-0.667551751197329,2.27589723201266,
15.6462651278366));
#94803=CARTESIAN_POINT('Ctrl Pts',(-0.656374365842741,2.27914594412967,
15.6454811470284));
#94804=CARTESIAN_POINT('Ctrl Pts',(-0.617309551288481,2.29018895157638,
15.6427374341107));
#94805=CARTESIAN_POINT('Ctrl Pts',(-0.58930463531729,2.29755444616941,15.6407639023634));
#94806=CARTESIAN_POINT('Ctrl Pts',(-0.405510698896786,2.34231228123675,
15.627763290267));
#94807=CARTESIAN_POINT('Ctrl Pts',(-0.246436695430811,2.36434282350857,
15.6162429224672));
#94808=CARTESIAN_POINT('Ctrl Pts',(0.0305223052916856,2.37443727383841,
15.5960196491619));
#94809=CARTESIAN_POINT('Ctrl Pts',(0.147591400314387,2.37004287545471,15.5874334085726));
#94810=CARTESIAN_POINT('Ctrl Pts',(0.296628233311328,2.35335862152401,15.5767444166407));
#94811=CARTESIAN_POINT('Ctrl Pts',(0.329315742653128,2.34900755372275,15.5744158525005));
#94812=CARTESIAN_POINT('Ctrl Pts',(0.383190566855927,2.34068942612889,15.5706150045806));
#94813=CARTESIAN_POINT('Ctrl Pts',(0.404432752252761,2.33711279827662,15.5691259774135));
#94814=CARTESIAN_POINT('Ctrl Pts',(0.433372756292473,2.33183364646898,15.5671131337406));
#94815=CARTESIAN_POINT('Ctrl Pts',(0.44111437564362,2.33038155948592,15.5665762358444));
#94816=CARTESIAN_POINT('Ctrl Pts',(0.45408591986779,2.32788154478926,15.565679394864));
#94817=CARTESIAN_POINT('Ctrl Pts',(0.459319743927618,2.32685450421688,15.5653182892404));
#94818=CARTESIAN_POINT('Ctrl Pts',(0.469235769770708,2.32487390752343,15.5646356286755));
#94819=CARTESIAN_POINT('Ctrl Pts',(0.47391861331523,2.32392384610825,15.5643138721748));
#94820=CARTESIAN_POINT('Ctrl Pts',(0.486181443842185,2.32139733917417,15.5634728725083));
#94821=CARTESIAN_POINT('Ctrl Pts',(0.493756719417407,2.31979790260435,15.5629549299859));
#94822=CARTESIAN_POINT('Ctrl Pts',(0.520041119446728,2.31411365432948,15.5611628501551));
#94823=CARTESIAN_POINT('Ctrl Pts',(0.538709110459365,2.30983924187163,15.5598989757146));
#94824=CARTESIAN_POINT('Ctrl Pts',(0.680273982986816,2.27561542413877,15.5503683030772));
#94825=CARTESIAN_POINT('Ctrl Pts',(0.800666791653876,2.23609921589381,15.5425655466694));
#94826=CARTESIAN_POINT('Ctrl Pts',(1.04320994128863,2.13437101562512,15.5264289460545));
#94827=CARTESIAN_POINT('Ctrl Pts',(1.16427438951561,2.07081843612407,15.5181243358305));
#94828=CARTESIAN_POINT('Ctrl Pts',(1.33778254877248,1.95968770741986,15.5051170235499));
#94829=CARTESIAN_POINT('Ctrl Pts',(1.39468193375601,1.91960904777053,15.500654515259));
#94830=CARTESIAN_POINT('Ctrl Pts',(1.46340236473173,1.86653418080533,15.4949639155562));
#94831=CARTESIAN_POINT('Ctrl Pts',(1.47695477547199,1.85582889678899,15.4938263909079));
#94832=CARTESIAN_POINT('Ctrl Pts',(1.49837532876951,1.83852518203905,15.4920032234204));
#94833=CARTESIAN_POINT('Ctrl Pts',(1.50631979928641,1.83202186872252,15.4913214056588));
#94834=CARTESIAN_POINT('Ctrl Pts',(1.52126145608069,1.81962779229639,15.4900282051661));
#94835=CARTESIAN_POINT('Ctrl Pts',(1.52826729767062,1.81374771759362,15.4894172650885));
#94836=CARTESIAN_POINT('Ctrl Pts',(1.54405246594036,1.80034267421544,15.4880301916087));
#94837=CARTESIAN_POINT('Ctrl Pts',(1.55281107256781,1.79279377699712,15.4872530805268));
#94838=CARTESIAN_POINT('Ctrl Pts',(1.57525468649004,1.77316214730051,15.4852421489502));
#94839=CARTESIAN_POINT('Ctrl Pts',(1.58885580325391,1.76098510266316,15.4840044150705));
#94840=CARTESIAN_POINT('Ctrl Pts',(1.68365841238046,1.67411615265017,15.4752395649969));
#94841=CARTESIAN_POINT('Ctrl Pts',(1.75968969943949,1.59400631607207,15.4674795033223));
#94842=CARTESIAN_POINT('Ctrl Pts',(1.93848425021609,1.37718103543882,15.447273532252));
#94843=CARTESIAN_POINT('Ctrl Pts',(2.03255791093118,1.23412022731677,15.4346208836244));
#94844=CARTESIAN_POINT('Ctrl Pts',(2.12849746078623,1.04702426137897,15.4195530831733));
#94845=CARTESIAN_POINT('Ctrl Pts',(2.14565642940838,1.01139512967129,15.4167468026605));
#94846=CARTESIAN_POINT('Ctrl Pts',(2.16873761004793,0.960234493183907,15.4128214764018));
#94847=CARTESIAN_POINT('Ctrl Pts',(2.17539918975181,0.945045768411009,15.4116689010702));
#94848=CARTESIAN_POINT('Ctrl Pts',(2.18688835756502,0.918084536443186,15.4096470209919));
#94849=CARTESIAN_POINT('Ctrl Pts',(2.19178149874506,0.906340876482218,15.4087743062491));
#94850=CARTESIAN_POINT('Ctrl Pts',(2.19898552911719,0.888651439036968,15.4074722669136));
#94851=CARTESIAN_POINT('Ctrl Pts',(2.20136721612126,0.882735022295279,15.4070388764785));
#94852=CARTESIAN_POINT('Ctrl Pts',(2.20543112019826,0.872521022017261,15.4062943644555));
#94853=CARTESIAN_POINT('Ctrl Pts',(2.20712468107788,0.868228082511681,15.4059825684169));
#94854=CARTESIAN_POINT('Ctrl Pts',(2.21095956240096,0.858423460763895,15.4052730257796));
#94855=CARTESIAN_POINT('Ctrl Pts',(2.21309280646223,0.852908703491206,15.4048757666451));
#94856=CARTESIAN_POINT('Ctrl Pts',(2.2188640681435,0.837821681758359,15.4037938141284));
#94857=CARTESIAN_POINT('Ctrl Pts',(2.22246080558044,0.828233602615362,15.4031115313396));
#94858=CARTESIAN_POINT('Ctrl Pts',(2.24015012524344,0.78013285601442,15.3997138139706));
#94859=CARTESIAN_POINT('Ctrl Pts',(2.25330524414738,0.741279861033008,15.3970495710709));
#94860=CARTESIAN_POINT('Ctrl Pts',(2.33688252521683,0.471604252435205,15.3789779048374));
#94861=CARTESIAN_POINT('Ctrl Pts',(2.37272984031019,0.231539202901166,15.3648481760502));
#94862=CARTESIAN_POINT('Ctrl Pts',(2.3714597914905,-0.0749467387794673,
15.345452960439));
#94863=CARTESIAN_POINT('Ctrl Pts',(2.36850826509816,-0.140021188520125,
15.3412683038638));
#94864=CARTESIAN_POINT('Ctrl Pts',(2.36142212425107,-0.22174275603374,15.3358902921084));
#94865=CARTESIAN_POINT('Ctrl Pts',(2.35978031332053,-0.238581530923435,
15.3347756163957));
#94866=CARTESIAN_POINT('Ctrl Pts',(2.35686127844497,-0.265531169756604,
15.3329805306024));
#94867=CARTESIAN_POINT('Ctrl Pts',(2.35569877301529,-0.275654082551759,
15.3323037394639));
#94868=CARTESIAN_POINT('Ctrl Pts',(2.35336731041903,-0.294863164662963,
15.3310145515511));
#94869=CARTESIAN_POINT('Ctrl Pts',(2.35221086601096,-0.303950689051917,
15.3304025608439));
#94870=CARTESIAN_POINT('Ctrl Pts',(2.34945823726129,-0.324624141647093,
15.3290054440933));
#94871=CARTESIAN_POINT('Ctrl Pts',(2.34782895433662,-0.33620534590711,15.3282192847716));
#94872=CARTESIAN_POINT('Ctrl Pts',(2.34337286498678,-0.366266531218341,
15.3261693370552));
#94873=CARTESIAN_POINT('Ctrl Pts',(2.34041314168541,-0.384725678207977,
15.3249013775674));
#94874=CARTESIAN_POINT('Ctrl Pts',(2.31088147635433,-0.555934644427472,
15.3130530028221));
#94875=CARTESIAN_POINT('Ctrl Pts',(2.26961478330569,-0.705739404518133,
15.3019951946732));
#94876=CARTESIAN_POINT('Ctrl Pts',(2.17429511959932,-0.953900677607855,
15.2826483166463));
#94877=CARTESIAN_POINT('Ctrl Pts',(2.12734274542635,-1.05446628587405,15.2745012187566));
#94878=CARTESIAN_POINT('Ctrl Pts',(2.03839427384134,-1.21465422554761,15.2612889834184));
#94879=CARTESIAN_POINT('Ctrl Pts',(2.00037781755153,-1.27629424839385,15.2561445052538));
#94880=CARTESIAN_POINT('Ctrl Pts',(1.95309470854254,-1.34564198902912,15.250364051202));
#94881=CARTESIAN_POINT('Ctrl Pts',(1.94652235843236,-1.35513173712203,15.2495732264203));
#94882=CARTESIAN_POINT('Ctrl Pts',(1.93635172628529,-1.36959033258048,15.2483690787595));
#94883=CARTESIAN_POINT('Ctrl Pts',(1.93280313161056,-1.3745936649038,15.2479525287097));
#94884=CARTESIAN_POINT('Ctrl Pts',(1.92626370166427,-1.38373852653173,15.2471915187425));
#94885=CARTESIAN_POINT('Ctrl Pts',(1.92327890387963,-1.38788415119684,15.2468466692938));
#94886=CARTESIAN_POINT('Ctrl Pts',(1.916548692219,-1.3971684236928,15.246074657047));
#94887=CARTESIAN_POINT('Ctrl Pts',(1.91279600122218,-1.40230166295096,15.2456480043178));
#94888=CARTESIAN_POINT('Ctrl Pts',(1.90314008920739,-1.41539893107691,15.2445597265373));
#94889=CARTESIAN_POINT('Ctrl Pts',(1.8972074269294,-1.42334125247638,15.2439000793855));
#94890=CARTESIAN_POINT('Ctrl Pts',(1.86132323863089,-1.47075802047232,15.2399621069503));
#94891=CARTESIAN_POINT('Ctrl Pts',(1.8301879752349,-1.50932639601643,15.2367598279655));
#94892=CARTESIAN_POINT('Ctrl Pts',(1.77592660046604,-1.57239122103343,15.2314707189579));
#94893=CARTESIAN_POINT('Ctrl Pts',(1.7534478908879,-1.59741982839115,15.2293567201913));
#94894=CARTESIAN_POINT('Ctrl Pts',(1.60522495697014,-1.75555627735332,15.2158391307444));
#94895=CARTESIAN_POINT('Ctrl Pts',(1.46495873073014,-1.87419972936961,15.2048926119263));
#94896=CARTESIAN_POINT('Ctrl Pts',(1.24745570586754,-2.01869718451607,15.1884798855032));
#94897=CARTESIAN_POINT('Ctrl Pts',(1.1803915742276,-2.05863007613359,15.1834928906512));
#94898=CARTESIAN_POINT('Ctrl Pts',(1.095703862192,-2.10355658925593,15.1772141357848));
#94899=CARTESIAN_POINT('Ctrl Pts',(1.07982692638187,-2.11175070921024,15.1760379137506));
#94900=CARTESIAN_POINT('Ctrl Pts',(1.05456638609734,-2.12442837242452,15.1741671925049));
#94901=CARTESIAN_POINT('Ctrl Pts',(1.04524304884126,-2.12903103200157,15.1734768783272));
#94902=CARTESIAN_POINT('Ctrl Pts',(1.0276786342104,-2.13755888939294,15.172176504498));
#94903=CARTESIAN_POINT('Ctrl Pts',(1.01944454905733,-2.14149811772279,15.1715669477575));
#94904=CARTESIAN_POINT('Ctrl Pts',(1.00091113221028,-2.15023348617479,15.1701949526509));
#94905=CARTESIAN_POINT('Ctrl Pts',(0.990599723483981,-2.15500332242454,
15.169431621171));
#94906=CARTESIAN_POINT('Ctrl Pts',(0.964234874947978,-2.16696992802376,
15.1674796928669));
#94907=CARTESIAN_POINT('Ctrl Pts',(0.948135137597761,-2.17406239439141,
15.1662875579813));
#94908=CARTESIAN_POINT('Ctrl Pts',(0.847200648254077,-2.21719298687842,
15.1588110608896));
#94909=CARTESIAN_POINT('Ctrl Pts',(0.760414893120203,-2.24843477666683,
15.152366476678));
#94910=CARTESIAN_POINT('Ctrl Pts',(0.471568132331998,-2.33377793781825,
15.1308690329009));
#94911=CARTESIAN_POINT('Ctrl Pts',(0.264169319705671,-2.36624147709204,
15.1152706012825));
#94912=CARTESIAN_POINT('Ctrl Pts',(0.0271842661256244,-2.37175992832376,
15.0984551707561));
#94913=CARTESIAN_POINT('Ctrl Pts',(-0.000856008987816744,-2.37191558918204,
15.0964832946151));
#94914=CARTESIAN_POINT('Ctrl Pts',(-0.0479729056820139,-2.37134154656322,
15.0932065738879));
#94915=CARTESIAN_POINT('Ctrl Pts',(-0.0670493228838324,-2.37087886171445,
15.0918900282509));
#94916=CARTESIAN_POINT('Ctrl Pts',(-0.0936242064805073,-2.36991328438927,
15.0900719607503));
#94917=CARTESIAN_POINT('Ctrl Pts',(-0.101128377379546,-2.36960492967955,
15.0895603552497));
#94918=CARTESIAN_POINT('Ctrl Pts',(-0.113886129406169,-2.36901998420539,
15.0886937464375));
#94919=CARTESIAN_POINT('Ctrl Pts',(-0.119140447466716,-2.36876155235646,
15.0883377453047));
#94920=CARTESIAN_POINT('Ctrl Pts',(-0.129238693264588,-2.368231187772,15.0876553577104));
#94921=CARTESIAN_POINT('Ctrl Pts',(-0.134082678871221,-2.36796187361332,
15.0873288214136));
#94922=CARTESIAN_POINT('Ctrl Pts',(-0.145698819661519,-2.36728028491948,
15.0865476041563));
#94923=CARTESIAN_POINT('Ctrl Pts',(-0.152470147879234,-2.36685380838694,
15.0860937099072));
#94924=CARTESIAN_POINT('Ctrl Pts',(-0.177019475663254,-2.36520183518045,
15.0844532475073));
#94925=CARTESIAN_POINT('Ctrl Pts',(-0.194785905700682,-2.36380500759528,
15.0832757867304));
#94926=CARTESIAN_POINT('Ctrl Pts',(-0.377394729226437,-2.34737509638493,
15.0712582266444));
#94927=CARTESIAN_POINT('Ctrl Pts',(-0.54027473902114,-2.31532219922393,
15.0612293375868));
#94928=CARTESIAN_POINT('Ctrl Pts',(-0.852703847329381,-2.2190378164147,
15.0411867072496));
#94929=CARTESIAN_POINT('Ctrl Pts',(-1.00162540526861,-2.15591487324638,
15.0312200923291));
#94930=CARTESIAN_POINT('Ctrl Pts',(-1.16191713918939,-2.06775574899828,
15.0192840198992));
#94931=CARTESIAN_POINT('Ctrl Pts',(-1.18071289607803,-2.05708101007848,
15.0178649534504));
#94932=CARTESIAN_POINT('Ctrl Pts',(-1.20901750025377,-2.04049015384406,
15.0156969316168));
#94933=CARTESIAN_POINT('Ctrl Pts',(-1.21863502530075,-2.03476093231182,
15.0149547394725));
#94934=CARTESIAN_POINT('Ctrl Pts',(-1.23601005038821,-2.02424314771093,
15.01360364118));
#94935=CARTESIAN_POINT('Ctrl Pts',(-1.24378123132898,-2.01947750923621,
15.0129955832088));
#94936=CARTESIAN_POINT('Ctrl Pts',(-1.26046007721091,-2.00911649956961,
15.0116823034575));
#94937=CARTESIAN_POINT('Ctrl Pts',(-1.26935834755861,-2.00350644979484,
15.0109765483053));
#94938=CARTESIAN_POINT('Ctrl Pts',(-1.29333607259869,-1.98816547169633,
15.0090607170913));
#94939=CARTESIAN_POINT('Ctrl Pts',(-1.3083426233917,-1.97832244297608,15.0078464854185));
#94940=CARTESIAN_POINT('Ctrl Pts',(-1.3824295380888,-1.92851604366728,15.0017743972143));
#94941=CARTESIAN_POINT('Ctrl Pts',(-1.43979210807213,-1.88607592021797,
14.9968235318599));
#94942=CARTESIAN_POINT('Ctrl Pts',(-1.64251208369558,-1.72144952395835,
14.9783728372181));
#94943=CARTESIAN_POINT('Ctrl Pts',(-1.7749627041595,-1.58452669437551,14.9643354820092));
#94944=CARTESIAN_POINT('Ctrl Pts',(-1.92300311826264,-1.38935301425882,
14.9466118471814));
#94945=CARTESIAN_POINT('Ctrl Pts',(-1.95480744672241,-1.34423639495542,
14.9426564949999));
#94946=CARTESIAN_POINT('Ctrl Pts',(-1.99639817419316,-1.28063472531,14.9373105589053));
#94947=CARTESIAN_POINT('Ctrl Pts',(-2.00755625147056,-1.26307123099609,
14.9358575255901));
#94948=CARTESIAN_POINT('Ctrl Pts',(-2.02645648535382,-1.2324377526826,14.9333660203053));
#94949=CARTESIAN_POINT('Ctrl Pts',(-2.03430673444773,-1.21943628030228,
14.932321651587));
#94950=CARTESIAN_POINT('Ctrl Pts',(-2.04551705796916,-1.20046031996867,
14.9308172312614));
#94951=CARTESIAN_POINT('Ctrl Pts',(-2.04897678099046,-1.19454559068206,
14.9303510796189));
#94952=CARTESIAN_POINT('Ctrl Pts',(-2.05499295541223,-1.18415732121081,
14.9295373119134));
#94953=CARTESIAN_POINT('Ctrl Pts',(-2.05756052616757,-1.17969033708224,
14.9291889874651));
#94954=CARTESIAN_POINT('Ctrl Pts',(-2.06298457192879,-1.17018216077645,
14.928450983254));
#94955=CARTESIAN_POINT('Ctrl Pts',(-2.06583713819187,-1.16513885598103,
14.9280615528165));
#94956=CARTESIAN_POINT('Ctrl Pts',(-2.07354948623876,-1.15138614695593,
14.9270049494077));
#94957=CARTESIAN_POINT('Ctrl Pts',(-2.07837292957114,-1.14265633754892,
14.9263400550907));
#94958=CARTESIAN_POINT('Ctrl Pts',(-2.10070846950034,-1.10162252310833,
14.9232406237444));
#94959=CARTESIAN_POINT('Ctrl Pts',(-2.1175244933606,-1.06894276966595,14.9208468483219));
#94960=CARTESIAN_POINT('Ctrl Pts',(-2.23095214681353,-0.835319485329479,
14.904161479299));
#94961=CARTESIAN_POINT('Ctrl Pts',(-2.29957270271285,-0.62200949898686,
14.8910312443448));
#94962=CARTESIAN_POINT('Ctrl Pts',(-2.3519311619069,-0.317751784463505,
14.8716979076568));
#94963=CARTESIAN_POINT('Ctrl Pts',(-2.36187689590785,-0.232553953821026,
14.8662349030271));
#94964=CARTESIAN_POINT('Ctrl Pts',(-2.3683262126787,-0.12870653940678,14.8594237829296));
#94965=CARTESIAN_POINT('Ctrl Pts',(-2.36925062837203,-0.110389544538584,
14.8582168395338));
#94966=CARTESIAN_POINT('Ctrl Pts',(-2.37037011560242,-0.0815711117898674,
14.8563083837736));
#94967=CARTESIAN_POINT('Ctrl Pts',(-2.37070803168282,-0.0710756898555659,
14.855611352009));
#94968=CARTESIAN_POINT('Ctrl Pts',(-2.37120911297899,-0.0514639198755605,
14.8543050095035));
#94969=CARTESIAN_POINT('Ctrl Pts',(-2.37138942833516,-0.0423481722896496,
14.8536962481865));
#94970=CARTESIAN_POINT('Ctrl Pts',(-2.37167436448929,-0.0220142570688781,
14.8523347376869));
#94971=CARTESIAN_POINT('Ctrl Pts',(-2.37175195957292,-0.0107959910226772,
14.8515811552777));
#94972=CARTESIAN_POINT('Ctrl Pts',(-2.37174609359546,0.0221537695712086,
14.8493603935021));
#94973=CARTESIAN_POINT('Ctrl Pts',(-2.37144354767738,0.0438835641855433,
14.8478864060153));
#94974=CARTESIAN_POINT('Ctrl Pts',(-2.37007987530885,0.0931637545855088,
14.8445212369417));
#94975=CARTESIAN_POINT('Ctrl Pts',(-2.36883687920081,0.120705549485069,
14.8426246159026));
#94976=CARTESIAN_POINT('Ctrl Pts',(-2.36659508990106,0.156507915565579,
14.8401378662955));
#94977=CARTESIAN_POINT('Ctrl Pts',(-2.36603252855054,0.164794130518723,
14.8395608422669));
#94978=CARTESIAN_POINT('Ctrl Pts',(-2.36542649432832,0.173076753001719,
14.8389825814723));
#94979=CARTESIAN_POINT('',(-2.37174911292529,0.00215604138794719,14.6517284628086));
#94980=CARTESIAN_POINT('Ctrl Pts',(-2.3654265029177,0.173076635611311,14.6411792785331));
#94981=CARTESIAN_POINT('Ctrl Pts',(-2.36958616881481,0.116226767218978,
14.6447256661978));
#94982=CARTESIAN_POINT('Ctrl Pts',(-2.37169717082288,0.0592160450641252,
14.6482297751778));
#94983=CARTESIAN_POINT('Ctrl Pts',(-2.37174902082752,0.00215515746287692,
14.6517286780464));
#94984=CARTESIAN_POINT('Ctrl Pts',(-2.37174902001529,0.00215605114073682,
14.6517286232472));
#94985=CARTESIAN_POINT('Ctrl Pts',(-2.37188407915844,-0.146414817317101,
14.6608388048995));
#94986=CARTESIAN_POINT('Ctrl Pts',(-2.35805940655107,-0.294662613876634,
14.6698964317843));
#94987=CARTESIAN_POINT('Ctrl Pts',(-2.3220300978616,-0.485213149403807,
14.6822539492024));
#94988=CARTESIAN_POINT('Ctrl Pts',(-2.31232638921229,-0.529529811924109,
14.6851775598427));
#94989=CARTESIAN_POINT('Ctrl Pts',(-2.29786298848713,-0.587565061965923,
14.6890853884549));
#94990=CARTESIAN_POINT('Ctrl Pts',(-2.29423932220956,-0.60155875287674,
14.6900337775809));
#94991=CARTESIAN_POINT('Ctrl Pts',(-2.28710858702346,-0.628093896280901,
14.6918442832747));
#94992=CARTESIAN_POINT('Ctrl Pts',(-2.28362569159036,-0.640641335449396,
14.6927056006159));
#94993=CARTESIAN_POINT('Ctrl Pts',(-2.27743214611189,-0.662261682418899,
14.6941990134174));
#94994=CARTESIAN_POINT('Ctrl Pts',(-2.27477013505126,-0.671348303314509,
14.6948295157564));
#94995=CARTESIAN_POINT('Ctrl Pts',(-2.26956024319579,-0.688745173680708,
14.6960422318557));
#94996=CARTESIAN_POINT('Ctrl Pts',(-2.26702094418615,-0.697057850469502,
14.6966241561753));
#94997=CARTESIAN_POINT('Ctrl Pts',(-2.26093876765243,-0.716583726961803,
14.6979969364017));
#94998=CARTESIAN_POINT('Ctrl Pts',(-2.25735810031847,-0.727784821951238,
14.698789021556));
#94999=CARTESIAN_POINT('Ctrl Pts',(-2.24462872751488,-0.766607177342344,
14.7015505961192));
#95000=CARTESIAN_POINT('Ctrl Pts',(-2.23505546399521,-0.794085404825248,
14.7035339726358));
#95001=CARTESIAN_POINT('Ctrl Pts',(-2.17032504499603,-0.969429260526127,
14.7163815708037));
#95002=CARTESIAN_POINT('Ctrl Pts',(-2.10104049577333,-1.11162753573527,
14.7277221522006));
#95003=CARTESIAN_POINT('Ctrl Pts',(-1.9560492464894,-1.3464969102428,14.7478565478278));
#95004=CARTESIAN_POINT('Ctrl Pts',(-1.88648850009718,-1.4423405060646,14.7565380655361));
#95005=CARTESIAN_POINT('Ctrl Pts',(-1.77790422004556,-1.57058328601222,
14.7685182191503));
#95006=CARTESIAN_POINT('Ctrl Pts',(-1.74455175217438,-1.6075494773613,14.7720181372453));
#95007=CARTESIAN_POINT('Ctrl Pts',(-1.70297446455836,-1.6508120830478,14.7761443206911));
#95008=CARTESIAN_POINT('Ctrl Pts',(-1.69584336508935,-1.65813686138779,
14.7768440009937));
#95009=CARTESIAN_POINT('Ctrl Pts',(-1.6843803995946,-1.66975985194065,14.7779556530799));
#95010=CARTESIAN_POINT('Ctrl Pts',(-1.68007901968961,-1.67408774663358,
14.7783698972478));
#95011=CARTESIAN_POINT('Ctrl Pts',(-1.67208723920401,-1.68206696552753,
14.7791341264748));
#95012=CARTESIAN_POINT('Ctrl Pts',(-1.66840157627194,-1.68572275099926,
14.779484454621));
#95013=CARTESIAN_POINT('Ctrl Pts',(-1.65999704766947,-1.69400458369598,
14.7802785481569));
#95014=CARTESIAN_POINT('Ctrl Pts',(-1.65527083748654,-1.69862302618862,
14.7807217200125));
#95015=CARTESIAN_POINT('Ctrl Pts',(-1.64292956654227,-1.71058246740024,
14.7818703966056));
#95016=CARTESIAN_POINT('Ctrl Pts',(-1.63528448928846,-1.71789248435492,
14.782573579838));
#95017=CARTESIAN_POINT('Ctrl Pts',(-1.58372774149858,-1.76653359688116,
14.7872619577807));
#95018=CARTESIAN_POINT('Ctrl Pts',(-1.53829817834778,-1.80623217010358,
14.7911343230446));
#95019=CARTESIAN_POINT('Ctrl Pts',(-1.3604906255676,-1.95002790562508,14.80556257972));
#95020=CARTESIAN_POINT('Ctrl Pts',(-1.21867405519078,-2.04166221802933,
14.8156523286273));
#95021=CARTESIAN_POINT('Ctrl Pts',(-1.00255946174628,-2.15069783848545,
14.8306582334018));
#95022=CARTESIAN_POINT('Ctrl Pts',(-0.935272425592493,-2.18080050035398,
14.8352785916219));
#95023=CARTESIAN_POINT('Ctrl Pts',(-0.838201431012205,-2.21890819725326,
14.8419553869037));
#95024=CARTESIAN_POINT('Ctrl Pts',(-0.809492620791687,-2.22954183449925,
14.8439311522988));
#95025=CARTESIAN_POINT('Ctrl Pts',(-0.758572156691437,-2.24728945046012,
14.8474429145604));
#95026=CARTESIAN_POINT('Ctrl Pts',(-0.73644602866137,-2.25463717138054,
14.8489712544664));
#95027=CARTESIAN_POINT('Ctrl Pts',(-0.702935621056583,-2.26521952734965,
14.8512912096976));
#95028=CARTESIAN_POINT('Ctrl Pts',(-0.691629118248512,-2.26869723600131,
14.8520748591022));
#95029=CARTESIAN_POINT('Ctrl Pts',(-0.67139772026644,-2.27475481439072,
14.8534788915955));
#95030=CARTESIAN_POINT('Ctrl Pts',(-0.662482728436488,-2.27736711899384,
14.8540982011746));
#95031=CARTESIAN_POINT('Ctrl Pts',(-0.64359457038248,-2.28278150615841,
14.8554117508069));
#95032=CARTESIAN_POINT('Ctrl Pts',(-0.633617958003769,-2.28557075000316,
14.8561063939867));
#95033=CARTESIAN_POINT('Ctrl Pts',(-0.606965035238863,-2.29283440845556,
14.857964550659));
#95034=CARTESIAN_POINT('Ctrl Pts',(-0.590257860485844,-2.29719215765701,
14.8591318100629));
#95035=CARTESIAN_POINT('Ctrl Pts',(-0.515584650582316,-2.31580086160872,
14.8643610256478));
#95036=CARTESIAN_POINT('Ctrl Pts',(-0.457145031694033,-2.32804176844397,
14.8684866177011));
#95037=CARTESIAN_POINT('Ctrl Pts',(-0.185879074554081,-2.37425434998922,
14.8878032272628));
#95038=CARTESIAN_POINT('Ctrl Pts',(0.0304803080597236,-2.3813186274865,
14.9038006607889));
#95039=CARTESIAN_POINT('Ctrl Pts',(0.313699421184216,-2.35193425649568,
14.9243059976412));
#95040=CARTESIAN_POINT('Ctrl Pts',(0.382301447171688,-2.34176210302865,
14.9292261053387));
#95041=CARTESIAN_POINT('Ctrl Pts',(0.461703040152434,-2.32640531740401,
14.9347956294977));
#95042=CARTESIAN_POINT('Ctrl Pts',(0.473024183568396,-2.32412984438194,
14.9355867155604));
#95043=CARTESIAN_POINT('Ctrl Pts',(0.49038569553102,-2.32050818092702,14.9367947723344));
#95044=CARTESIAN_POINT('Ctrl Pts',(0.496437968678867,-2.31922092384733,
14.9372149473856));
#95045=CARTESIAN_POINT('Ctrl Pts',(0.507552272119802,-2.31681152344353,
14.9379847035603));
#95046=CARTESIAN_POINT('Ctrl Pts',(0.512615644213608,-2.3156964711449,14.9383346681992));
#95047=CARTESIAN_POINT('Ctrl Pts',(0.524018163837556,-2.31314618399231,
14.9391211869554));
#95048=CARTESIAN_POINT('Ctrl Pts',(0.530355083448118,-2.31170149296202,
14.9395571954198));
#95049=CARTESIAN_POINT('Ctrl Pts',(0.546639768905023,-2.30791842323976,
14.9406750193388));
#95050=CARTESIAN_POINT('Ctrl Pts',(0.556578632375637,-2.30554174123821,
14.941354714291));
#95051=CARTESIAN_POINT('Ctrl Pts',(0.618234443303363,-2.29037603839949,
14.9455572123572));
#95052=CARTESIAN_POINT('Ctrl Pts',(0.669528167059367,-2.27591064849159,
14.9489922011807));
#95053=CARTESIAN_POINT('Ctrl Pts',(0.746125572671108,-2.25149498684292,
14.9540890844331));
#95054=CARTESIAN_POINT('Ctrl Pts',(0.77181339914516,-2.24281903226161,14.9557927132238));
#95055=CARTESIAN_POINT('Ctrl Pts',(0.97105013081545,-2.17169908891392,14.9690015845943));
#95056=CARTESIAN_POINT('Ctrl Pts',(1.13692704357163,-2.08964504591076,14.9800233120382));
#95057=CARTESIAN_POINT('Ctrl Pts',(1.35737603429716,-1.94650308303175,14.9965402697932));
#95058=CARTESIAN_POINT('Ctrl Pts',(1.42096334074232,-1.90058020396791,15.0015504883894));
#95059=CARTESIAN_POINT('Ctrl Pts',(1.49625450140992,-1.84031156746689,15.0078659166613));
#95060=CARTESIAN_POINT('Ctrl Pts',(1.51022343750123,-1.82886558752378,15.0090546846172));
#95061=CARTESIAN_POINT('Ctrl Pts',(1.53213066004606,-1.81049293060851,15.0109470146997));
#95062=CARTESIAN_POINT('Ctrl Pts',(1.54015603950557,-1.80367080674768,15.0116463155656));
#95063=CARTESIAN_POINT('Ctrl Pts',(1.55515275794233,-1.79074949592438,15.0129647065017));
#95064=CARTESIAN_POINT('Ctrl Pts',(1.56213434973657,-1.78466246860957,15.0135832865284));
#95065=CARTESIAN_POINT('Ctrl Pts',(1.57774183428862,-1.77089304866532,15.0149771190655));
#95066=CARTESIAN_POINT('Ctrl Pts',(1.58634756972254,-1.76318826711683,15.0157533000154));
#95067=CARTESIAN_POINT('Ctrl Pts',(1.60816923232508,-1.7433620866982,15.0177413173231));
#95068=CARTESIAN_POINT('Ctrl Pts',(1.62130439243005,-1.73115328072409,15.018956838408));
#95069=CARTESIAN_POINT('Ctrl Pts',(1.70440942380411,-1.65213375990979,15.0267708210299));
#95070=CARTESIAN_POINT('Ctrl Pts',(1.77036532926587,-1.58125252367993,15.0335461051405));
#95071=CARTESIAN_POINT('Ctrl Pts',(1.947877243474,-1.36541726744294,15.0535322448719));
#95072=CARTESIAN_POINT('Ctrl Pts',(2.04724073255277,-1.2113575385468,15.067088396166));
#95073=CARTESIAN_POINT('Ctrl Pts',(2.15474540495974,-0.992953590609145,
15.0845484657005));
#95074=CARTESIAN_POINT('Ctrl Pts',(2.17946062796281,-0.937463297247468,
15.0888411724001));
#95075=CARTESIAN_POINT('Ctrl Pts',(2.20617544200097,-0.870696881086827,
15.0937908285052));
#95076=CARTESIAN_POINT('Ctrl Pts',(2.21025671114814,-0.860283919930739,
15.0945566964036));
#95077=CARTESIAN_POINT('Ctrl Pts',(2.21645356154783,-0.844138023600395,
15.0957344089074));
#95078=CARTESIAN_POINT('Ctrl Pts',(2.21862083421389,-0.838425303485623,
15.0961492174612));
#95079=CARTESIAN_POINT('Ctrl Pts',(2.22258839060707,-0.827844097587817,
15.0969139624857));
#95080=CARTESIAN_POINT('Ctrl Pts',(2.22439475842074,-0.822978106399219,
15.0972642459179));
#95081=CARTESIAN_POINT('Ctrl Pts',(2.22846078673267,-0.811913854020796,
15.0980575730636));
#95082=CARTESIAN_POINT('Ctrl Pts',(2.23071056789279,-0.805712075937854,
15.0985000280209));
#95083=CARTESIAN_POINT('Ctrl Pts',(2.23648781269638,-0.789576748061331,
15.0996456061896));
#95084=CARTESIAN_POINT('Ctrl Pts',(2.23997502951377,-0.779628792942433,
15.1003464284599));
#95085=CARTESIAN_POINT('Ctrl Pts',(2.26272031862458,-0.713330893769666,
15.1049828851964));
#95086=CARTESIAN_POINT('Ctrl Pts',(2.27991845296082,-0.656290662968781,
15.1088085193969));
#95087=CARTESIAN_POINT('Ctrl Pts',(2.31228212858095,-0.53222471196045,15.1169023755771));
#95088=CARTESIAN_POINT('Ctrl Pts',(2.32672001592493,-0.465066407494585,
15.121145356429));
#95089=CARTESIAN_POINT('Ctrl Pts',(2.35892814836613,-0.275547189256023,
15.1329590184188));
#95090=CARTESIAN_POINT('Ctrl Pts',(2.37007882267018,-0.152294011403453,
15.1404676034347));
#95091=CARTESIAN_POINT('Ctrl Pts',(2.37229237931211,0.0303956330879317,
15.1518890829129));
#95092=CARTESIAN_POINT('Ctrl Pts',(2.37079708877883,0.0895288105885493,
15.1556290710958));
#95093=CARTESIAN_POINT('Ctrl Pts',(2.36544366523301,0.174838825398544,15.1611272287962));
#95094=CARTESIAN_POINT('Ctrl Pts',(2.36335535873658,0.20110621679509,15.1628341394351));
#95095=CARTESIAN_POINT('Ctrl Pts',(2.35881515900443,0.248255814529363,15.1659265974966));
#95096=CARTESIAN_POINT('Ctrl Pts',(2.35652237844452,0.269150769800251,15.1673071865638));
#95097=CARTESIAN_POINT('Ctrl Pts',(2.35258666572137,0.301095935328145,15.1694346221225));
#95098=CARTESIAN_POINT('Ctrl Pts',(2.35114284616125,0.312169972451478,15.1701752002129));
#95099=CARTESIAN_POINT('Ctrl Pts',(2.34848424031921,0.331495694677993,15.1714731816141));
#95100=CARTESIAN_POINT('Ctrl Pts',(2.34730402716108,0.33975200313287,15.172029483578));
#95101=CARTESIAN_POINT('Ctrl Pts',(2.34453988231379,0.358386692141769,15.173289178486));
#95102=CARTESIAN_POINT('Ctrl Pts',(2.34293054712228,0.368761069083972,15.1739933650291));
#95103=CARTESIAN_POINT('Ctrl Pts',(2.33839100185604,0.396794676942097,15.1759042026645));
#95104=CARTESIAN_POINT('Ctrl Pts',(2.33532970803214,0.41443167989719,15.1771149809511));
#95105=CARTESIAN_POINT('Ctrl Pts',(2.32006243002613,0.496843061129686,15.1828140615002));
#95106=CARTESIAN_POINT('Ctrl Pts',(2.30536033336788,0.561119381146274,15.187380776995));
#95107=CARTESIAN_POINT('Ctrl Pts',(2.23169526248906,0.830924396912919,15.2070847821052));
#95108=CARTESIAN_POINT('Ctrl Pts',(2.1477637219239,1.02858446220783,15.2229767452182));
#95109=CARTESIAN_POINT('Ctrl Pts',(2.01655841703121,1.24921453156977,15.241417722844));
#95110=CARTESIAN_POINT('Ctrl Pts',(1.99359196459685,1.28554904115497,15.2444753204328));
#95111=CARTESIAN_POINT('Ctrl Pts',(1.95505671005739,1.34299572489189,15.2493205954363));
#95112=CARTESIAN_POINT('Ctrl Pts',(1.94010378572815,1.36450786066598,15.2511375763042));
#95113=CARTESIAN_POINT('Ctrl Pts',(1.91979580876341,1.39271510865154,15.2535189084736));
#95114=CARTESIAN_POINT('Ctrl Pts',(1.91475720757121,1.39963429615781,15.2541029510482));
#95115=CARTESIAN_POINT('Ctrl Pts',(1.90640030776704,1.41098069998046,15.2550603320241));
#95116=CARTESIAN_POINT('Ctrl Pts',(1.90310383411348,1.41542377660126,15.255435136135));
#95117=CARTESIAN_POINT('Ctrl Pts',(1.89660594535028,1.42411806782916,15.2561683133144));
#95118=CARTESIAN_POINT('Ctrl Pts',(1.8934057270203,1.42837009801208,15.256526760657));
#95119=CARTESIAN_POINT('Ctrl Pts',(1.88546936141968,1.43884135966132,15.2574092911295));
#95120=CARTESIAN_POINT('Ctrl Pts',(1.88071667119692,1.4450480885286,15.2579322271438));
#95121=CARTESIAN_POINT('Ctrl Pts',(1.86417590617694,1.46642949857931,15.2597335147248));
#95122=CARTESIAN_POINT('Ctrl Pts',(1.85223378870077,1.48148484091234,15.2610015758265));
#95123=CARTESIAN_POINT('Ctrl Pts',(1.76158619417707,1.59295381731406,15.2704023289056));
#95124=CARTESIAN_POINT('Ctrl Pts',(1.67557291078516,1.68319683948664,15.278087237919));
#95125=CARTESIAN_POINT('Ctrl Pts',(1.48050011699526,1.85801245203081,15.2941643012499));
#95126=CARTESIAN_POINT('Ctrl Pts',(1.37036413288083,1.94066749617801,15.3025244507063));
#95127=CARTESIAN_POINT('Ctrl Pts',(1.21448141570072,2.03773569614314,15.3141139268554));
#95128=CARTESIAN_POINT('Ctrl Pts',(1.17456625541696,2.06100111043549,15.3170601976165));
#95129=CARTESIAN_POINT('Ctrl Pts',(1.10539073973818,2.09865918166663,15.3221513434685));
#95130=CARTESIAN_POINT('Ctrl Pts',(1.07646579789997,2.1136414704478,15.3242757940824));
#95131=CARTESIAN_POINT('Ctrl Pts',(1.03531410950908,2.13389303998039,15.3272967576469));
#95132=CARTESIAN_POINT('Ctrl Pts',(1.0233366742371,2.13966278896058,15.3281758400736));
#95133=CARTESIAN_POINT('Ctrl Pts',(1.00270190958164,2.14939003939643,15.3296903130966));
#95134=CARTESIAN_POINT('Ctrl Pts',(0.994068008356898,2.15339672405444,15.330323987384));
#95135=CARTESIAN_POINT('Ctrl Pts',(0.977554320270775,2.16093965828936,15.3315360900953));
#95136=CARTESIAN_POINT('Ctrl Pts',(0.969678859997232,2.1644850567527,15.3321141915063));
#95137=CARTESIAN_POINT('Ctrl Pts',(0.949260759971957,2.17354313926609,15.3336132021712));
#95138=CARTESIAN_POINT('Ctrl Pts',(0.936689549640122,2.17899023461167,15.3345363341513));
#95139=CARTESIAN_POINT('Ctrl Pts',(0.900633508450888,2.19424361265366,15.33718497023));
#95140=CARTESIAN_POINT('Ctrl Pts',(0.877037693912088,2.20378096545064,15.338919467926));
#95141=CARTESIAN_POINT('Ctrl Pts',(0.674657946939588,2.28181726577387,15.3538109982713));
#95142=CARTESIAN_POINT('Ctrl Pts',(0.488372604105772,2.3288015298481,15.367702749917));
#95143=CARTESIAN_POINT('Ctrl Pts',(0.178264514818422,2.36814540170152,15.3905327926856));
#95144=CARTESIAN_POINT('Ctrl Pts',(0.05700911703828,2.37416235216484,15.3993643359055));
#95145=CARTESIAN_POINT('Ctrl Pts',(-0.0850730743664251,2.37031585521377,
15.4092678461821));
#95146=CARTESIAN_POINT('Ctrl Pts',(-0.105953385329535,2.36947433778072,
15.4107117039305));
#95147=CARTESIAN_POINT('Ctrl Pts',(-0.134660229625759,2.36793714422441,
15.4126784252293));
#95148=CARTESIAN_POINT('Ctrl Pts',(-0.142497736268541,2.36747842567647,
15.4132134941106));
#95149=CARTESIAN_POINT('Ctrl Pts',(-0.155703984657882,2.3666396633045,15.4141117525515));
#95150=CARTESIAN_POINT('Ctrl Pts',(-0.161073921805298,2.36628024977837,
15.4144760726008));
#95151=CARTESIAN_POINT('Ctrl Pts',(-0.17130588959036,2.36556042461378,15.4151684223748));
#95152=CARTESIAN_POINT('Ctrl Pts',(-0.176168083728361,2.36520329732695,
15.4154966390823));
#95153=CARTESIAN_POINT('Ctrl Pts',(-0.187716036577664,2.36431929483684,
15.416274377685));
#95154=CARTESIAN_POINT('Ctrl Pts',(-0.194400775885755,2.36377904623439,
15.4167231575918));
#95155=CARTESIAN_POINT('Ctrl Pts',(-0.217976359209992,2.36177302320012,
15.4183011499951));
#95156=CARTESIAN_POINT('Ctrl Pts',(-0.234854183731834,2.36015445668455,
15.4194222245435));
#95157=CARTESIAN_POINT('Ctrl Pts',(-0.425286930044106,2.3398290395197,15.4319886928342));
#95158=CARTESIAN_POINT('Ctrl Pts',(-0.596312956175944,2.30219446218493,
15.4425248252931));
#95159=CARTESIAN_POINT('Ctrl Pts',(-0.843344323952578,2.21842390892055,
15.4585313339605));
#95160=CARTESIAN_POINT('Ctrl Pts',(-0.923434994510418,2.18629840932515,
15.4638488995471));
#95161=CARTESIAN_POINT('Ctrl Pts',(-1.06843643381551,2.11874472183461,15.4739246455523));
#95162=CARTESIAN_POINT('Ctrl Pts',(-1.13378347644475,2.08450687777171,15.4786461563837));
#95163=CARTESIAN_POINT('Ctrl Pts',(-1.21273769158019,2.03832775471391,15.4846379006));
#95164=CARTESIAN_POINT('Ctrl Pts',(-1.22794883147133,2.02920042950557,15.48580590956));
#95165=CARTESIAN_POINT('Ctrl Pts',(-1.25196676623674,2.01441970703472,15.4876727305471));
#95166=CARTESIAN_POINT('Ctrl Pts',(-1.26084120320339,2.0088770480488,15.4883674779864));
#95167=CARTESIAN_POINT('Ctrl Pts',(-1.27751014367972,1.99831225465248,15.4896819961845));
#95168=CARTESIAN_POINT('Ctrl Pts',(-1.28531246004263,1.99330276429487,15.4903012895199));
#95169=CARTESIAN_POINT('Ctrl Pts',(-1.30285751027588,1.98189209196657,15.491703067741));
#95170=CARTESIAN_POINT('Ctrl Pts',(-1.31258276794445,1.97546460994222,15.4924865263094));
#95171=CARTESIAN_POINT('Ctrl Pts',(-1.33743778065287,1.9587732120232,15.4945056899544));
#95172=CARTESIAN_POINT('Ctrl Pts',(-1.35249671857184,1.9484057346483,15.495745279423));
#95173=CARTESIAN_POINT('Ctrl Pts',(-1.45414015891353,1.87668213295483,15.5042252346625));
#95174=CARTESIAN_POINT('Ctrl Pts',(-1.53662954343993,1.80975777666961,15.511679967145));
#95175=CARTESIAN_POINT('Ctrl Pts',(-1.76947049451228,1.59342535986851,15.5344960603421));
#95176=CARTESIAN_POINT('Ctrl Pts',(-1.90458076916447,1.42919465779465,15.5503199148087));
#95177=CARTESIAN_POINT('Ctrl Pts',(-2.03012248219144,1.2265846022667,15.5670218090217));
#95178=CARTESIAN_POINT('Ctrl Pts',(-2.04376591912257,1.20371429273349,15.5688692978379));
#95179=CARTESIAN_POINT('Ctrl Pts',(-2.06130853139191,1.17314933167095,15.5712840569237));
#95180=CARTESIAN_POINT('Ctrl Pts',(-2.06555444311969,1.16565735287634,15.5718717036749));
#95181=CARTESIAN_POINT('Ctrl Pts',(-2.07246658434096,1.1533044057457,15.5728334558691));
#95182=CARTESIAN_POINT('Ctrl Pts',(-2.07515669584047,1.14845700174375,15.5732090528179));
#95183=CARTESIAN_POINT('Ctrl Pts',(-2.08039191624003,1.13894502581081,15.5739424892654));
#95184=CARTESIAN_POINT('Ctrl Pts',(-2.08293837817727,1.13428127490075,15.5743004099822));
#95185=CARTESIAN_POINT('Ctrl Pts',(-2.08917264981897,1.12277164484894,15.5751796717716));
#95186=CARTESIAN_POINT('Ctrl Pts',(-2.09284255060222,1.11591603174464,15.5756998850522));
#95187=CARTESIAN_POINT('Ctrl Pts',(-2.10534779883016,1.09227673029467,15.5774820563793));
#95188=CARTESIAN_POINT('Ctrl Pts',(-2.11401577944215,1.07540464481927,15.5787340132242));
#95189=CARTESIAN_POINT('Ctrl Pts',(-2.18612238692098,0.930808474258009,
15.5893094541972));
#95190=CARTESIAN_POINT('Ctrl Pts',(-2.23813340819028,0.797687955272024,
15.5980405478792));
#95191=CARTESIAN_POINT('Ctrl Pts',(-2.29648430277262,0.596508853296747,
15.6108779156309));
#95192=CARTESIAN_POINT('Ctrl Pts',(-2.31237730707812,0.531576793309128,
15.6149674495067));
#95193=CARTESIAN_POINT('Ctrl Pts',(-2.340985853288,0.388828751946018,15.6239711531178));
#95194=CARTESIAN_POINT('Ctrl Pts',(-2.35260612703856,0.310878471967256,
15.6288969703466));
#95195=CARTESIAN_POINT('Ctrl Pts',(-2.36227572960904,0.212712792373175,
15.6352034205374));
#95196=CARTESIAN_POINT('Ctrl Pts',(-2.36397576033377,0.19290382185746,15.6364810911436));
#95197=CARTESIAN_POINT('Ctrl Pts',(-2.36542649459319,0.173076749381846,
15.6377659025437));
#95198=CARTESIAN_POINT('Origin',(0.,0.,-1.84858989190503));
#95199=CARTESIAN_POINT('',(-2.36542649454112,0.173076750093503,16.8347081153257));
#95200=CARTESIAN_POINT('',(-2.36542650336594,0.173076629485306,16.639047070016));
#95201=CARTESIAN_POINT('',(-2.36542649454111,0.173076750093529,-1.84858989190503));
#95202=CARTESIAN_POINT('',(-2.37174901238863,-0.00218034299483271,15.8485516738248));
#95203=CARTESIAN_POINT('Ctrl Pts',(-2.36542649454112,0.173076750093436,
16.8347081153257));
#95204=CARTESIAN_POINT('Ctrl Pts',(-2.36533617570272,0.174311130639557,
16.8346254070491));
#95205=CARTESIAN_POINT('Ctrl Pts',(-2.36524489032645,0.175545444712604,
16.8345427506042));
#95206=CARTESIAN_POINT('Ctrl Pts',(-2.36391281400652,0.193367423027911,
16.8333499699269));
#95207=CARTESIAN_POINT('Ctrl Pts',(-2.36249847603169,0.209942235006699,
16.8322491253632));
#95208=CARTESIAN_POINT('Ctrl Pts',(-2.35359957088513,0.302698903603241,
16.8261290782948));
#95209=CARTESIAN_POINT('Ctrl Pts',(-2.34260389197387,0.378506420972745,
16.8212801743013));
#95210=CARTESIAN_POINT('Ctrl Pts',(-2.29067130219724,0.645000732237099,
16.804363538187));
#95211=CARTESIAN_POINT('Ctrl Pts',(-2.22993731004444,0.831013748684088,
16.7927308734518));
#95212=CARTESIAN_POINT('Ctrl Pts',(-2.11971056829759,1.0659219185898,16.7763160834327));
#95213=CARTESIAN_POINT('Ctrl Pts',(-2.08992726287125,1.12319423164069,16.7721714559497));
#95214=CARTESIAN_POINT('Ctrl Pts',(-2.04908633141048,1.19446801615383,16.7667899210928));
#95215=CARTESIAN_POINT('Ctrl Pts',(-2.04015461308784,1.20966018451698,16.7656295031259));
#95216=CARTESIAN_POINT('Ctrl Pts',(-2.02571293365896,1.23360941008247,16.7637782008537));
#95217=CARTESIAN_POINT('Ctrl Pts',(-2.02031342522013,1.242432583414,16.7630913529259));
#95218=CARTESIAN_POINT('Ctrl Pts',(-2.01051938240359,1.25820406223153,16.7618548078621));
#95219=CARTESIAN_POINT('Ctrl Pts',(-2.00614608595954,1.26516541530651,16.7613059012589));
#95220=CARTESIAN_POINT('Ctrl Pts',(-1.99583076141785,1.28139723836003,16.7600186334271));
#95221=CARTESIAN_POINT('Ctrl Pts',(-1.9898602311561,1.29064928003093,16.7592792202131));
#95222=CARTESIAN_POINT('Ctrl Pts',(-1.97246445608558,1.31719844896596,16.7571407864881));
#95223=CARTESIAN_POINT('Ctrl Pts',(-1.96087682681101,1.33438742756422,16.7557357025098));
#95224=CARTESIAN_POINT('Ctrl Pts',(-1.85406522923017,1.48843467876153,16.742952261787));
#95225=CARTESIAN_POINT('Ctrl Pts',(-1.74490208264013,1.61502055063036,16.7310176564493));
#95226=CARTESIAN_POINT('Ctrl Pts',(-1.50581348109747,1.83949381046031,16.7071068823235));
#95227=CARTESIAN_POINT('Ctrl Pts',(-1.37726570381673,1.93761693322448,16.6952162024716));
#95228=CARTESIAN_POINT('Ctrl Pts',(-1.22431931440361,2.03139549522977,16.6827489309086));
#95229=CARTESIAN_POINT('Ctrl Pts',(-1.20878602382077,2.04067680936544,16.6815009110854));
#95230=CARTESIAN_POINT('Ctrl Pts',(-1.1872528034207,2.05321098849625,16.6797972495607));
#95231=CARTESIAN_POINT('Ctrl Pts',(-1.18134328461928,2.05661679204363,16.6793324095788));
#95232=CARTESIAN_POINT('Ctrl Pts',(-1.1711970383492,2.06240616487493,16.6785390452809));
#95233=CARTESIAN_POINT('Ctrl Pts',(-1.1669675675838,2.0648022638635,16.6782097313688));
#95234=CARTESIAN_POINT('Ctrl Pts',(-1.15815231821045,2.06976058125513,16.6775263176511));
#95235=CARTESIAN_POINT('Ctrl Pts',(-1.15356536516053,2.07232058447675,16.6771723711277));
#95236=CARTESIAN_POINT('Ctrl Pts',(-1.14243531716525,2.07848391947978,16.6763174676491));
#95237=CARTESIAN_POINT('Ctrl Pts',(-1.13588355611618,2.08207166260082,16.6758174997181));
#95238=CARTESIAN_POINT('Ctrl Pts',(-1.11276433339208,2.09459013458696,16.674064366193));
#95239=CARTESIAN_POINT('Ctrl Pts',(-1.09610708943823,2.10335484343125,16.6728212237736));
#95240=CARTESIAN_POINT('Ctrl Pts',(-0.991861081030645,2.15663221289448,
16.6651536253653));
#95241=CARTESIAN_POINT('Ctrl Pts',(-0.901670595950356,2.19587015915884,
16.6590071197204));
#95242=CARTESIAN_POINT('Ctrl Pts',(-0.658672096993869,2.28408106635424,
16.6430487977259));
#95243=CARTESIAN_POINT('Ctrl Pts',(-0.502901181207463,2.32335203886898,
16.6333870689937));
#95244=CARTESIAN_POINT('Ctrl Pts',(-0.271985804316576,2.3572383787849,16.6186908837538));
#95245=CARTESIAN_POINT('Ctrl Pts',(-0.199164422236027,2.3645043696942,16.6140091751904));
#95246=CARTESIAN_POINT('Ctrl Pts',(-0.10807750245448,2.3693552060209,16.6080377281787));
#95247=CARTESIAN_POINT('Ctrl Pts',(-0.0900161544375763,2.37011010308593,
16.6068481338259));
#95248=CARTESIAN_POINT('Ctrl Pts',(-0.0614041847593705,2.37097846265692,
16.6049541071176));
#95249=CARTESIAN_POINT('Ctrl Pts',(-0.0508581517034558,2.37122811778336,
16.6042539450632));
#95250=CARTESIAN_POINT('Ctrl Pts',(-0.0311983581266371,2.37156230958205,
16.6029447430095));
#95251=CARTESIAN_POINT('Ctrl Pts',(-0.0220850632155012,2.37166468366853,
16.6023362738307));
#95252=CARTESIAN_POINT('Ctrl Pts',(-0.00181518510370797,2.37177554481518,
16.600979271786));
#95253=CARTESIAN_POINT('Ctrl Pts',(0.00934126530847542,2.37175784245316,
16.6002299318039));
#95254=CARTESIAN_POINT('Ctrl Pts',(0.0419255783884655,2.3714762335178,16.598033972593));
#95255=CARTESIAN_POINT('Ctrl Pts',(0.0633500117264997,2.37100063339745,
16.5965807739839));
#95256=CARTESIAN_POINT('Ctrl Pts',(0.252211877356171,2.36424654562392,16.5836844607207));
#95257=CARTESIAN_POINT('Ctrl Pts',(0.418519295769792,2.34053262250061,16.5716804045725));
#95258=CARTESIAN_POINT('Ctrl Pts',(0.735236340058118,2.26052261831971,16.5478571236935));
#95259=CARTESIAN_POINT('Ctrl Pts',(0.885259017458775,2.20609608089654,16.5361293189005));
#95260=CARTESIAN_POINT('Ctrl Pts',(1.04508637725509,2.12916015845876,16.5238017350609));
#95261=CARTESIAN_POINT('Ctrl Pts',(1.06137530294645,2.12108722905776,16.5225477855257));
#95262=CARTESIAN_POINT('Ctrl Pts',(1.08365631243148,2.10972361492944,16.5208375164233));
#95263=CARTESIAN_POINT('Ctrl Pts',(1.08972887215594,2.10659339289433,16.5203719050675));
#95264=CARTESIAN_POINT('Ctrl Pts',(1.10010161639664,2.10118969970303,16.519577566067));
#95265=CARTESIAN_POINT('Ctrl Pts',(1.10440844346936,2.09892918213749,16.51924804467));
#95266=CARTESIAN_POINT('Ctrl Pts',(1.11334994336599,2.09420092996764,16.5185645759924));
#95267=CARTESIAN_POINT('Ctrl Pts',(1.11798340429571,2.09173103907508,16.5182107802222));
#95268=CARTESIAN_POINT('Ctrl Pts',(1.12917760214604,2.0857160916241,16.5173568524488));
#95269=CARTESIAN_POINT('Ctrl Pts',(1.1357299710987,2.08215539972302,16.5168577038867));
#95270=CARTESIAN_POINT('Ctrl Pts',(1.15869109753201,2.06953721419665,16.5151105892596));
#95271=CARTESIAN_POINT('Ctrl Pts',(1.17500971292941,2.06031589073837,16.5138725551421));
#95272=CARTESIAN_POINT('Ctrl Pts',(1.27544571060828,2.00198000894331,16.5062646627697));
#95273=CARTESIAN_POINT('Ctrl Pts',(1.35659050829796,1.94790978384181,16.5001681086439));
#95274=CARTESIAN_POINT('Ctrl Pts',(1.46044632887465,1.86905899972199,16.4921162388261));
#95275=CARTESIAN_POINT('Ctrl Pts',(1.48628657622867,1.84857709975849,16.4900907974325));
#95276=CARTESIAN_POINT('Ctrl Pts',(1.6541571684501,1.70972082054441,16.4767290701639));
#95277=CARTESIAN_POINT('Ctrl Pts',(1.78233742009686,1.57564116773329,16.4654791236031));
#95278=CARTESIAN_POINT('Ctrl Pts',(1.91054789826366,1.40562904757918,16.4516716397998));
#95279=CARTESIAN_POINT('Ctrl Pts',(1.9270523009774,1.38291561962534,16.4498368080758));
#95280=CARTESIAN_POINT('Ctrl Pts',(1.94973692362416,1.35050212860594,16.4472292216274));
#95281=CARTESIAN_POINT('Ctrl Pts',(1.95625618206859,1.34104131666104,16.4464693995572));
#95282=CARTESIAN_POINT('Ctrl Pts',(1.9675022376664,1.32446441323959,16.4451400815902));
#95283=CARTESIAN_POINT('Ctrl Pts',(1.97225984601859,1.3173693990945,16.4445717617784));
#95284=CARTESIAN_POINT('Ctrl Pts',(1.98214641608798,1.30245197321451,16.4433780963415));
#95285=CARTESIAN_POINT('Ctrl Pts',(1.98726762861412,1.29462462716546,16.442752473146));
#95286=CARTESIAN_POINT('Ctrl Pts',(1.999368548526,1.27588839152302,16.4412564862635));
#95287=CARTESIAN_POINT('Ctrl Pts',(2.00630540839049,1.26495232207124,16.4403845494136));
#95288=CARTESIAN_POINT('Ctrl Pts',(2.02961681583138,1.227527359973,16.4374044913445));
#95289=CARTESIAN_POINT('Ctrl Pts',(2.04555847719562,1.20077399776745,16.4352806365019));
#95290=CARTESIAN_POINT('Ctrl Pts',(2.08259546773821,1.1357394546441,16.4301306219768));
#95291=CARTESIAN_POINT('Ctrl Pts',(2.10316771981346,1.09717505862559,16.4270870393097));
#95292=CARTESIAN_POINT('Ctrl Pts',(2.23679871427543,0.829088480404798,16.4059963486313));
#95293=CARTESIAN_POINT('Ctrl Pts',(2.31311270784828,0.583206262588846,16.3867357693863));
#95294=CARTESIAN_POINT('Ctrl Pts',(2.35257849925455,0.302246837219172,16.3668222853823));
#95295=CARTESIAN_POINT('Ctrl Pts',(2.35597609363102,0.274509681348841,16.364881024595));
#95296=CARTESIAN_POINT('Ctrl Pts',(2.35982011674732,0.237756709145371,16.3623468315939));
#95297=CARTESIAN_POINT('Ctrl Pts',(2.36070628259687,0.228790493897491,16.3617315805551));
#95298=CARTESIAN_POINT('Ctrl Pts',(2.36205853424685,0.214263113001964,16.3607397987397));
#95299=CARTESIAN_POINT('Ctrl Pts',(2.3625561141146,0.208705079273164,16.3603615529729));
#95300=CARTESIAN_POINT('Ctrl Pts',(2.3634818965698,0.197936157527195,16.3596310772723));
#95301=CARTESIAN_POINT('Ctrl Pts',(2.36391248840145,0.192725570722194,16.3592787243643));
#95302=CARTESIAN_POINT('Ctrl Pts',(2.36490578697394,0.180201241814655,16.358434336287));
#95303=CARTESIAN_POINT('Ctrl Pts',(2.36545180706015,0.172886150146965,16.3579432301242));
#95304=CARTESIAN_POINT('Ctrl Pts',(2.36721929880935,0.14762880262042,16.3562543497708));
#95305=CARTESIAN_POINT('Ctrl Pts',(2.36827067489717,0.129674712189231,16.3550656476386));
#95306=CARTESIAN_POINT('Ctrl Pts',(2.37872711325141,-0.0920833506401716,
16.3405102065191));
#95307=CARTESIAN_POINT('Ctrl Pts',(2.36200287983935,-0.296297986119699,
16.3283711887797));
#95308=CARTESIAN_POINT('Ctrl Pts',(2.29326099487223,-0.617820652472512,
16.3080826352234));
#95309=CARTESIAN_POINT('Ctrl Pts',(2.25761633218332,-0.737502838405029,
16.3002624276322));
#95310=CARTESIAN_POINT('Ctrl Pts',(2.20601910657216,-0.871220796122533,
16.2909025801712));
#95311=CARTESIAN_POINT('Ctrl Pts',(2.19909944774937,-0.888542379610534,
16.289677974538));
#95312=CARTESIAN_POINT('Ctrl Pts',(2.18751475642649,-0.916577184348615,
16.2876752193181));
#95313=CARTESIAN_POINT('Ctrl Pts',(2.18297350301448,-0.927340941243415,
16.2869012497671));
#95314=CARTESIAN_POINT('Ctrl Pts',(2.1747302721878,-0.946483069195635,16.2855156296985));
#95315=CARTESIAN_POINT('Ctrl Pts',(2.17105890594106,-0.95487443149719,16.2849050327117));
#95316=CARTESIAN_POINT('Ctrl Pts',(2.16319788135841,-0.972562059829648,
16.2836111498312));
#95317=CARTESIAN_POINT('Ctrl Pts',(2.15899670476978,-0.981852971317604,
16.2829274783043));
#95318=CARTESIAN_POINT('Ctrl Pts',(2.14765220402877,-1.00651647446432,16.2811017091746));
#95319=CARTESIAN_POINT('Ctrl Pts',(2.140403874461,-1.02183982646383,16.2799560069773));
#95320=CARTESIAN_POINT('Ctrl Pts',(2.10434358847059,-1.09600577371286,16.2743541112912));
#95321=CARTESIAN_POINT('Ctrl Pts',(2.0732686402692,-1.15370979010063,16.2698196648299));
#95322=CARTESIAN_POINT('Ctrl Pts',(1.91417641015858,-1.42190050384566,16.2478724385789));
#95323=CARTESIAN_POINT('Ctrl Pts',(1.75630270374976,-1.61283575755307,16.229388119014));
#95324=CARTESIAN_POINT('Ctrl Pts',(1.54464106643181,-1.80016866782357,16.2094094376548));
#95325=CARTESIAN_POINT('Ctrl Pts',(1.5168273976501,-1.8236661609592,16.2068668467367));
#95326=CARTESIAN_POINT('Ctrl Pts',(1.48074295088946,-1.85275394635916,16.2036830757187));
#95327=CARTESIAN_POINT('Ctrl Pts',(1.47296464575211,-1.85894379516006,16.2030033923139));
#95328=CARTESIAN_POINT('Ctrl Pts',(1.46059694040858,-1.86865944635325,16.2019333830018));
#95329=CARTESIAN_POINT('Ctrl Pts',(1.45603326880744,-1.87221758103514,16.2015408320305));
#95330=CARTESIAN_POINT('Ctrl Pts',(1.44738027045671,-1.87891324451396,16.2008009058681));
#95331=CARTESIAN_POINT('Ctrl Pts',(1.44329378598774,-1.88205411069947,16.2004533060632));
#95332=CARTESIAN_POINT('Ctrl Pts',(1.4337397347113,-1.88934792305906,16.1996448523224));
#95333=CARTESIAN_POINT('Ctrl Pts',(1.4282643392905,-1.89349047564534,16.1991847280566));
#95334=CARTESIAN_POINT('Ctrl Pts',(1.41056043560559,-1.906764335725,16.197706975059));
#95335=CARTESIAN_POINT('Ctrl Pts',(1.39826144800889,-1.91580164102501,16.1966956418841));
#95336=CARTESIAN_POINT('Ctrl Pts',(1.36888366370195,-1.93695482659693,16.1943136344407));
#95337=CARTESIAN_POINT('Ctrl Pts',(1.35172970773243,-1.94896468665653,16.1929493091814));
#95338=CARTESIAN_POINT('Ctrl Pts',(1.28836573615744,-1.99208808581077,16.1879970125502));
#95339=CARTESIAN_POINT('Ctrl Pts',(1.24121986128674,-2.02180002900068,16.1844793434659));
#95340=CARTESIAN_POINT('Ctrl Pts',(1.02688626074101,-2.14654944682609,16.1690142813773));
#95341=CARTESIAN_POINT('Ctrl Pts',(0.849562055822769,-2.22270511311299,
16.1575391100184));
#95342=CARTESIAN_POINT('Ctrl Pts',(0.599215427544226,-2.29582959502444,
16.1410761667402));
#95343=CARTESIAN_POINT('Ctrl Pts',(0.532650579853703,-2.31217962553114,
16.1366826892701));
#95344=CARTESIAN_POINT('Ctrl Pts',(0.448102133597615,-2.32910207647693,
16.1310357650741));
#95345=CARTESIAN_POINT('Ctrl Pts',(0.430690284209022,-2.3323845856906,16.1298694274504));
#95346=CARTESIAN_POINT('Ctrl Pts',(0.402936932366686,-2.33729532705455,
16.1280042209181));
#95347=CARTESIAN_POINT('Ctrl Pts',(0.392618373174155,-2.33905075284699,
16.1273094033278));
#95348=CARTESIAN_POINT('Ctrl Pts',(0.373287346545925,-2.34220789095282,
16.1260050544224));
#95349=CARTESIAN_POINT('Ctrl Pts',(0.364277726658014,-2.34362603274966,
16.1253960572953));
#95350=CARTESIAN_POINT('Ctrl Pts',(0.344123236211176,-2.34667938602927,
16.1240312177397));
#95351=CARTESIAN_POINT('Ctrl Pts',(0.332974506141521,-2.34828722969584,
16.123274522952));
#95352=CARTESIAN_POINT('Ctrl Pts',(0.300063484305986,-2.35279450153916,
16.1210354787866));
#95353=CARTESIAN_POINT('Ctrl Pts',(0.278272408952129,-2.35547117809369,
16.1195461502331));
#95354=CARTESIAN_POINT('Ctrl Pts',(0.108378267009901,-2.37394949405787,
16.1078782791159));
#95355=CARTESIAN_POINT('Ctrl Pts',(-0.0408509129551264,-2.37606776643412,
16.0972650740089));
#95356=CARTESIAN_POINT('Ctrl Pts',(-0.273901578097779,-2.35741060508209,
16.08026335504));
#95357=CARTESIAN_POINT('Ctrl Pts',(-0.358109371584906,-2.34609554568976,
16.0740386865986));
#95358=CARTESIAN_POINT('Ctrl Pts',(-0.540205367386482,-2.31159315547355,
16.0605545377084));
#95359=CARTESIAN_POINT('Ctrl Pts',(-0.637607967696352,-2.28664510532846,
16.0533264306466));
#95360=CARTESIAN_POINT('Ctrl Pts',(-0.745128999687133,-2.25169705193351,
16.0455262453547));
#95361=CARTESIAN_POINT('Ctrl Pts',(-0.75708166587365,-2.24770643293271,
16.0446617413604));
#95362=CARTESIAN_POINT('Ctrl Pts',(-0.775091696695292,-2.24153348431924,
16.0433636713543));
#95363=CARTESIAN_POINT('Ctrl Pts',(-0.781172676876621,-2.23942152151149,
16.0429261732525));
#95364=CARTESIAN_POINT('Ctrl Pts',(-0.792067212753133,-2.23558800432949,
16.042143872362));
#95365=CARTESIAN_POINT('Ctrl Pts',(-0.796883848702104,-2.23387562946221,
16.0417985435126));
#95366=CARTESIAN_POINT('Ctrl Pts',(-0.807405736566323,-2.23009660275287,
16.0410453600294));
#95367=CARTESIAN_POINT('Ctrl Pts',(-0.813108599435453,-2.22802362839086,
16.0406378855409));
#95368=CARTESIAN_POINT('Ctrl Pts',(-0.828687360842096,-2.22229301159185,
16.0395266625553));
#95369=CARTESIAN_POINT('Ctrl Pts',(-0.83854710093816,-2.21859138671503,
16.0388254609616));
#95370=CARTESIAN_POINT('Ctrl Pts',(-0.899640904612517,-2.19518957885801,
16.0344916623222));
#95371=CARTESIAN_POINT('Ctrl Pts',(-0.950207518037905,-2.17377962025859,
16.0309529724007));
#95372=CARTESIAN_POINT('Ctrl Pts',(-1.13140032553404,-2.08952950890807,
16.0182914772698));
#95373=CARTESIAN_POINT('Ctrl Pts',(-1.25694335468402,-2.01650691556494,
16.0095392689006));
#95374=CARTESIAN_POINT('Ctrl Pts',(-1.48867711433565,-1.8516180171476,15.9920485441622));
#95375=CARTESIAN_POINT('Ctrl Pts',(-1.59494300794087,-1.76090815367774,
15.9833527433846));
#95376=CARTESIAN_POINT('Ctrl Pts',(-1.70579422406851,-1.64797389206909,
15.9730203504685));
#95377=CARTESIAN_POINT('Ctrl Pts',(-1.71881013690306,-1.63439394381048,
15.9717855463248));
#95378=CARTESIAN_POINT('Ctrl Pts',(-1.73967811049984,-1.61209668602616,
15.9697694130094));
#95379=CARTESIAN_POINT('Ctrl Pts',(-1.74762960622435,-1.60347323155543,
15.9689923581639));
#95380=CARTESIAN_POINT('Ctrl Pts',(-1.76167924631987,-1.58800764807777,
15.9676032996199));
#95381=CARTESIAN_POINT('Ctrl Pts',(-1.76780235768211,-1.58118843829046,
15.966992369422));
#95382=CARTESIAN_POINT('Ctrl Pts',(-1.78063657639965,-1.56672744246382,
15.9656999508173));
#95383=CARTESIAN_POINT('Ctrl Pts',(-1.78733834508678,-1.55907765386027,
15.9650180893987));
#95384=CARTESIAN_POINT('Ctrl Pts',(-1.8008619095087,-1.54343927518922,15.9636277258134));
#95385=CARTESIAN_POINT('Ctrl Pts',(-1.8076802387571,-1.53544800026534,15.9629191013909));
#95386=CARTESIAN_POINT('Ctrl Pts',(-1.83714539922911,-1.50044570574904,
15.9598230750714));
#95387=CARTESIAN_POINT('Ctrl Pts',(-1.85924053461064,-1.47297825340967,
15.957413462809));
#95388=CARTESIAN_POINT('Ctrl Pts',(-1.93973270080922,-1.36821725339418,
15.9482915147709));
#95389=CARTESIAN_POINT('Ctrl Pts',(-1.99398244553544,-1.28787080424194,
15.9414256504957));
#95390=CARTESIAN_POINT('Ctrl Pts',(-2.08667011980185,-1.13063943018615,
15.9282625183686));
#95391=CARTESIAN_POINT('Ctrl Pts',(-2.12614426868707,-1.054536450132,15.9220016201069));
#95392=CARTESIAN_POINT('Ctrl Pts',(-2.21575877287421,-0.85617471462228,
15.9061033935888));
#95393=CARTESIAN_POINT('Ctrl Pts',(-2.25997385379626,-0.731538661048981,
15.8964908511269));
#95394=CARTESIAN_POINT('Ctrl Pts',(-2.29676236927959,-0.591807356432421,
15.8865239123712));
#95395=CARTESIAN_POINT('Ctrl Pts',(-2.29983995670252,-0.579732281874622,
15.8856691522359));
#95396=CARTESIAN_POINT('Ctrl Pts',(-2.30435575927281,-0.561412192081109,
15.8843827933144));
#95397=CARTESIAN_POINT('Ctrl Pts',(-2.30586400863065,-0.555184915930167,
15.8839473646129));
#95398=CARTESIAN_POINT('Ctrl Pts',(-2.30852985023345,-0.54397987947777,
15.8831672468825));
#95399=CARTESIAN_POINT('Ctrl Pts',(-2.30969660047925,-0.539004447097838,
15.8828220451017));
#95400=CARTESIAN_POINT('Ctrl Pts',(-2.31221905592662,-0.528089212803355,
15.8820673602205));
#95401=CARTESIAN_POINT('Ctrl Pts',(-2.31356795803539,-0.522147953112554,
15.8816582684804));
#95402=CARTESIAN_POINT('Ctrl Pts',(-2.31631188806069,-0.509842860325071,
15.880814356802));
#95403=CARTESIAN_POINT('Ctrl Pts',(-2.31770362059747,-0.503478335719643,
15.8803797226988));
#95404=CARTESIAN_POINT('Ctrl Pts',(-2.32123047074438,-0.487025154039982,
15.8792607402974));
#95405=CARTESIAN_POINT('Ctrl Pts',(-2.32332607620465,-0.476928036305058,
15.8785784992669));
#95406=CARTESIAN_POINT('Ctrl Pts',(-2.3293147153752,-0.447096847026955,
15.8765751560402));
#95407=CARTESIAN_POINT('Ctrl Pts',(-2.33302275033609,-0.427326035668191,
15.8752632486081));
#95408=CARTESIAN_POINT('Ctrl Pts',(-2.35982196460956,-0.273671294235081,
15.8651728829661));
#95409=CARTESIAN_POINT('Ctrl Pts',(-2.3716240877574,-0.138062488030204,
15.8568770509635));
#95410=CARTESIAN_POINT('Ctrl Pts',(-2.37174899790563,-0.00218023705663272,
15.8485516447737));
#95411=CARTESIAN_POINT('Ctrl Pts',(-2.37174899780696,-0.00218034439917192,
15.8485516513505));
#95412=CARTESIAN_POINT('Ctrl Pts',(-2.37180279384753,0.0563382572370928,
15.8449662594045));
#95413=CARTESIAN_POINT('Ctrl Pts',(-2.36969079452154,0.114797017167598,
15.8413837181339));
#95414=CARTESIAN_POINT('Ctrl Pts',(-2.3654264678378,0.173077115045234,15.8377719611872));
#95415=CARTESIAN_POINT('Ctrl Pts',(-2.36542649459319,0.173076749381846,
15.6377659025437));
#95416=CARTESIAN_POINT('Ctrl Pts',(-2.36631134326739,0.160983591258964,
15.6385495496222));
#95417=CARTESIAN_POINT('Ctrl Pts',(-2.36710344948036,0.148883698754822,
15.6393358508964));
#95418=CARTESIAN_POINT('Ctrl Pts',(-2.36921667602307,0.112301069719473,
15.6417203895829));
#95419=CARTESIAN_POINT('Ctrl Pts',(-2.37025093872748,0.087804339989173,
15.6433269601623));
#95420=CARTESIAN_POINT('Ctrl Pts',(-2.37122207081869,0.0514286380925134,
15.6457290649617));
#95421=CARTESIAN_POINT('Ctrl Pts',(-2.37144979429577,0.0395585440656365,
15.6465155157445));
#95422=CARTESIAN_POINT('Ctrl Pts',(-2.37169689066206,0.0183933053218808,
15.6479226634835));
#95423=CARTESIAN_POINT('Ctrl Pts',(-2.37175075912594,0.00909874794829185,
15.648542268556));
#95424=CARTESIAN_POINT('Ctrl Pts',(-2.37174913884153,-0.010530621915938,
15.6498544549616));
#95425=CARTESIAN_POINT('Ctrl Pts',(-2.3716807349954,-0.0208652097371478,
15.6505474276722));
#95426=CARTESIAN_POINT('Ctrl Pts',(-2.37131912426492,-0.0483526079760888,
15.652396380362));
#95427=CARTESIAN_POINT('Ctrl Pts',(-2.37090735729391,-0.0655029764717682,
15.6535560412081));
#95428=CARTESIAN_POINT('Ctrl Pts',(-2.36800590946871,-0.148716293252062,
15.6592131153046));
#95429=CARTESIAN_POINT('Ctrl Pts',(-2.36294109887037,-0.214654117274369,
15.6637900571563));
#95430=CARTESIAN_POINT('Ctrl Pts',(-2.32516883836494,-0.532035648390992,
15.6862948703533));
#95431=CARTESIAN_POINT('Ctrl Pts',(-2.25505024466011,-0.777293436356326,
15.7053643700398));
#95432=CARTESIAN_POINT('Ctrl Pts',(-2.13496872761573,-1.03342772216534,
15.7252461944924));
#95433=CARTESIAN_POINT('Ctrl Pts',(-2.12197935460644,-1.05984345240878,
15.7272931885206));
#95434=CARTESIAN_POINT('Ctrl Pts',(-2.10425637371343,-1.09425275966583,
15.7299486161534));
#95435=CARTESIAN_POINT('Ctrl Pts',(-2.09996349835073,-1.10246873023807,
15.730581817809));
#95436=CARTESIAN_POINT('Ctrl Pts',(-2.09295825398374,-1.11568641544864,
15.7315988874223));
#95437=CARTESIAN_POINT('Ctrl Pts',(-2.09027591817234,-1.12070380484424,
15.7319845861501));
#95438=CARTESIAN_POINT('Ctrl Pts',(-2.0850635669779,-1.13036984819048,15.7327268371551));
#95439=CARTESIAN_POINT('Ctrl Pts',(-2.08253602848405,-1.13501971905999,
15.7330835307112));
#95440=CARTESIAN_POINT('Ctrl Pts',(-2.07644831807439,-1.14613038540311,
15.7339350347479));
#95441=CARTESIAN_POINT('Ctrl Pts',(-2.07287348946835,-1.15258317631219,
15.7344289194539));
#95442=CARTESIAN_POINT('Ctrl Pts',(-2.06054219413112,-1.17459899763979,
15.7361121193993));
#95443=CARTESIAN_POINT('Ctrl Pts',(-2.05163983692345,-1.19008023514798,
15.7372925459132));
#95444=CARTESIAN_POINT('Ctrl Pts',(-1.94441592511465,-1.37176325021753,
15.7511259403435));
#95445=CARTESIAN_POINT('Ctrl Pts',(-1.82630988652712,-1.52548501698307,
15.7626764463837));
#95446=CARTESIAN_POINT('Ctrl Pts',(-1.59621020903865,-1.7594102709425,15.7828753777435));
#95447=CARTESIAN_POINT('Ctrl Pts',(-1.49354547756389,-1.84735645835428,
15.7913042326119));
#95448=CARTESIAN_POINT('Ctrl Pts',(-1.36858058133164,-1.93714851196461,
15.801350165109));
#95449=CARTESIAN_POINT('Ctrl Pts',(-1.35305975293344,-1.94802115896561,
15.8025940309628));
#95450=CARTESIAN_POINT('Ctrl Pts',(-1.32761702485824,-1.9653935308073,15.8046277878265));
#95451=CARTESIAN_POINT('Ctrl Pts',(-1.31777351977363,-1.97200700748384,
15.8054133650298));
#95452=CARTESIAN_POINT('Ctrl Pts',(-1.30012845483306,-1.9836709473229,15.8068195401472));
#95453=CARTESIAN_POINT('Ctrl Pts',(-1.29234597248754,-1.98874993638936,
15.8074390519087));
#95454=CARTESIAN_POINT('Ctrl Pts',(-1.27583973779702,-1.99938440296286,
15.808751657762));
#95455=CARTESIAN_POINT('Ctrl Pts',(-1.26710911587882,-2.00492880420458,
15.809445146872));
#95456=CARTESIAN_POINT('Ctrl Pts',(-1.2437719625559,-2.01953579949575,15.8112969444497));
#95457=CARTESIAN_POINT('Ctrl Pts',(-1.229102926197,-2.02849685972918,15.8124589538399));
#95458=CARTESIAN_POINT('Ctrl Pts',(-1.15719014017813,-2.07136072116984,
15.8181471208542));
#95459=CARTESIAN_POINT('Ctrl Pts',(-1.09863970524698,-2.10300107736592,
15.8227538720135));
#95460=CARTESIAN_POINT('Ctrl Pts',(-0.804860947462469,-2.24613902027037,
15.8457691102005));
#95461=CARTESIAN_POINT('Ctrl Pts',(-0.55376648330663,-2.32082903353083,
15.8653908050566));
#95462=CARTESIAN_POINT('Ctrl Pts',(-0.272029619000312,-2.35621769094964,
15.8852423421883));
#95463=CARTESIAN_POINT('Ctrl Pts',(-0.248424784876344,-2.35882325659125,
15.8868874403877));
#95464=CARTESIAN_POINT('Ctrl Pts',(-0.216295793451214,-2.3618820651424,
15.8890985143586));
#95465=CARTESIAN_POINT('Ctrl Pts',(-0.207803433990869,-2.36264438677919,
15.8896802848559));
#95466=CARTESIAN_POINT('Ctrl Pts',(-0.194348917044858,-2.36377903328643,
15.8905975809338));
#95467=CARTESIAN_POINT('Ctrl Pts',(-0.189389487173416,-2.36418155882362,
15.8909347553056));
#95468=CARTESIAN_POINT('Ctrl Pts',(-0.179145571107979,-2.36498055147068,
15.8916291967896));
#95469=CARTESIAN_POINT('Ctrl Pts',(-0.17386099911327,-2.36537491701392,
15.8919863313915));
#95470=CARTESIAN_POINT('Ctrl Pts',(-0.161178102738392,-2.36627865543115,
15.8928408711688));
#95471=CARTESIAN_POINT('Ctrl Pts',(-0.153778544067317,-2.36677105337061,
15.8933373330714));
#95472=CARTESIAN_POINT('Ctrl Pts',(-0.128316864190886,-2.36834546648013,
15.895038797576));
#95473=CARTESIAN_POINT('Ctrl Pts',(-0.110244186457916,-2.36925552334713,
15.8962346494589));
#95474=CARTESIAN_POINT('Ctrl Pts',(-0.00260461544937177,-2.37344137628158,
15.9032960410269));
#95475=CARTESIAN_POINT('Ctrl Pts',(0.0870893102498231,-2.37184526406578,
15.9089300712097));
#95476=CARTESIAN_POINT('Ctrl Pts',(0.262626872989535,-2.35874682502402,
15.919831644605));
#95477=CARTESIAN_POINT('Ctrl Pts',(0.348352970704382,-2.34761800585365,
15.9250973675146));
#95478=CARTESIAN_POINT('Ctrl Pts',(0.5822925405043,-2.30414932650543,15.9397031800274));
#95479=CARTESIAN_POINT('Ctrl Pts',(0.728283654516866,-2.2622471630529,15.9491074507989));
#95480=CARTESIAN_POINT('Ctrl Pts',(0.886913424052246,-2.19975959467743,
15.9602378773239));
#95481=CARTESIAN_POINT('Ctrl Pts',(0.904473376747888,-2.19259790490656,
15.961482648542));
#95482=CARTESIAN_POINT('Ctrl Pts',(0.932875283084999,-2.18061516587046,
15.963517593173));
#95483=CARTESIAN_POINT('Ctrl Pts',(0.943770491125504,-2.17592188435986,
15.9643034443188));
#95484=CARTESIAN_POINT('Ctrl Pts',(0.963137497869736,-2.16740642137893,
15.9657099243245));
#95485=CARTESIAN_POINT('Ctrl Pts',(0.971622963394734,-2.16361578105142,
15.9663294652346));
#95486=CARTESIAN_POINT('Ctrl Pts',(0.989501704740244,-2.15550257589281,
15.9676419390078));
#95487=CARTESIAN_POINT('Ctrl Pts',(0.998889406674494,-2.15116826996895,
15.9683352657454));
#95488=CARTESIAN_POINT('Ctrl Pts',(1.02379751441148,-2.13946998566868,15.9701861687651));
#95489=CARTESIAN_POINT('Ctrl Pts',(1.03926652070592,-2.13199864960447,15.9713474396586));
#95490=CARTESIAN_POINT('Ctrl Pts',(1.11412415492165,-2.09483508093924,15.977025806264));
#95491=CARTESIAN_POINT('Ctrl Pts',(1.17232393371998,-2.06282857451295,15.9816231590127));
#95492=CARTESIAN_POINT('Ctrl Pts',(1.44978472303103,-1.89470457806378,16.0044697084451));
#95493=CARTESIAN_POINT('Ctrl Pts',(1.6471212070856,-1.72590164929287,16.023908047607));
#95494=CARTESIAN_POINT('Ctrl Pts',(1.82988567228383,-1.5090962922528,16.0437678882579));
#95495=CARTESIAN_POINT('Ctrl Pts',(1.84606576412765,-1.48925972287497,16.0455434557501));
#95496=CARTESIAN_POINT('Ctrl Pts',(1.86736132667646,-1.46227112185837,16.0478998672218));
#95497=CARTESIAN_POINT('Ctrl Pts',(1.87276208353858,-1.45534784254626,16.0484992159628));
#95498=CARTESIAN_POINT('Ctrl Pts',(1.88119363931474,-1.44441469594736,16.0494374537593));
#95499=CARTESIAN_POINT('Ctrl Pts',(1.8842502826396,-1.44042500535293,16.0497781220154));
#95500=CARTESIAN_POINT('Ctrl Pts',(1.89048600929064,-1.43223199399843,16.0504741520808));
#95501=CARTESIAN_POINT('Ctrl Pts',(1.89366377337741,-1.42802778329928,16.0508294088157));
#95502=CARTESIAN_POINT('Ctrl Pts',(1.90117613402937,-1.41801969040789,16.0516706506771));
#95503=CARTESIAN_POINT('Ctrl Pts',(1.90549824681049,-1.41220641900579,16.0521557690981));
#95504=CARTESIAN_POINT('Ctrl Pts',(1.91991382147241,-1.39263069660829,16.0537779257677));
#95505=CARTESIAN_POINT('Ctrl Pts',(1.92988564566857,-1.37877872602922,16.0549069219039));
#95506=CARTESIAN_POINT('Ctrl Pts',(1.98554862906991,-1.29966945456524,16.0612561868064));
#95507=CARTESIAN_POINT('Ctrl Pts',(2.02808358047842,-1.23224341729562,16.0662927950689));
#95508=CARTESIAN_POINT('Ctrl Pts',(2.16535194256524,-0.988216354172134,
16.0837104603745));
#95509=CARTESIAN_POINT('Ctrl Pts',(2.24104234669843,-0.801905214317238,
16.0956646999749));
#95510=CARTESIAN_POINT('Ctrl Pts',(2.30692333880819,-0.553626026889995,
16.1119899127481));
#95511=CARTESIAN_POINT('Ctrl Pts',(2.31946831013191,-0.498460639596935,
16.1156347928399));
#95512=CARTESIAN_POINT('Ctrl Pts',(2.33319204266687,-0.426262662596877,
16.1204532279965));
#95513=CARTESIAN_POINT('Ctrl Pts',(2.33617668133387,-0.409589372785323,
16.1215692392768));
#95514=CARTESIAN_POINT('Ctrl Pts',(2.34068649944891,-0.38274090274353,16.1233721569007));
#95515=CARTESIAN_POINT('Ctrl Pts',(2.34232453975285,-0.372585066957693,
16.1240554740859));
#95516=CARTESIAN_POINT('Ctrl Pts',(2.34531832248156,-0.353223179002146,
16.1253608912502));
#95517=CARTESIAN_POINT('Ctrl Pts',(2.34668606026206,-0.3440191539199,16.1259825982509));
#95518=CARTESIAN_POINT('Ctrl Pts',(2.34968788895487,-0.322967373467029,
16.1274073361614));
#95519=CARTESIAN_POINT('Ctrl Pts',(2.35128658491925,-0.311114908487316,
16.1282114695021));
#95520=CARTESIAN_POINT('Ctrl Pts',(2.35594635326863,-0.274478504451135,
16.1307034797173));
#95521=CARTESIAN_POINT('Ctrl Pts',(2.35870561189589,-0.24965861100176,16.1324007841839));
#95522=CARTESIAN_POINT('Ctrl Pts',(2.37009713187918,-0.130013889384252,
16.1406290551175));
#95523=CARTESIAN_POINT('Ctrl Pts',(2.3734047312238,-0.0347822048791796,
16.1473234187161));
#95524=CARTESIAN_POINT('Ctrl Pts',(2.36700753309429,0.216419937859404,16.1653406258765));
#95525=CARTESIAN_POINT('Ctrl Pts',(2.34763891667966,0.371683116098985,16.1768638115163));
#95526=CARTESIAN_POINT('Ctrl Pts',(2.30730454719941,0.549770269147731,16.1900657858004));
#95527=CARTESIAN_POINT('Ctrl Pts',(2.30101171848522,0.575540419663705,16.1919748281507));
#95528=CARTESIAN_POINT('Ctrl Pts',(2.28066973482631,0.653169064556107,16.1977120649367));
#95529=CARTESIAN_POINT('Ctrl Pts',(2.26528860714011,0.704665059014168,16.201499815575));
#95530=CARTESIAN_POINT('Ctrl Pts',(2.24490643746561,0.765309152039998,16.2059045759265));
#95531=CARTESIAN_POINT('Ctrl Pts',(2.24157977842134,0.774998785582229,16.2066066284557));
#95532=CARTESIAN_POINT('Ctrl Pts',(2.23603752744574,0.790807550649909,16.2077488491666));
#95533=CARTESIAN_POINT('Ctrl Pts',(2.23385939377354,0.796939532045251,16.2081911111398));
#95534=CARTESIAN_POINT('Ctrl Pts',(2.22990037324158,0.807941379709544,16.208983089878));
#95535=CARTESIAN_POINT('Ctrl Pts',(2.22812873812324,0.812814416464725,16.2093333365608));
#95536=CARTESIAN_POINT('Ctrl Pts',(2.2242101151525,0.823483837887346,16.2100989981503));
#95537=CARTESIAN_POINT('Ctrl Pts',(2.2220564472532,0.829277646531788,16.2105140109562));
#95538=CARTESIAN_POINT('Ctrl Pts',(2.21582531816323,0.84584209583743,16.2116985201911));
#95539=CARTESIAN_POINT('Ctrl Pts',(2.21169195540132,0.856591734435686,16.2124647783753));
#95540=CARTESIAN_POINT('Ctrl Pts',(2.18242541852354,0.931080928072647,16.21776038779));
#95541=CARTESIAN_POINT('Ctrl Pts',(2.15461617268167,0.993742210508296,16.2221431591681));
#95542=CARTESIAN_POINT('Ctrl Pts',(2.07375581623797,1.15652773882642,16.2335598488762));
#95543=CARTESIAN_POINT('Ctrl Pts',(2.01618207264991,1.25420581714142,16.2404479159748));
#95544=CARTESIAN_POINT('Ctrl Pts',(1.86325014110692,1.47574325160229,16.2569635762311));
#95545=CARTESIAN_POINT('Ctrl Pts',(1.76222459476682,1.59501530850938,16.2666236821927));
#95546=CARTESIAN_POINT('Ctrl Pts',(1.63665258877876,1.71666070253472,16.2780379353255));
#95547=CARTESIAN_POINT('Ctrl Pts',(1.622913736542,1.72965506206226,16.2792792388647));
#95548=CARTESIAN_POINT('Ctrl Pts',(1.60031752330987,1.75052056197424,16.2813096338896));
#95549=CARTESIAN_POINT('Ctrl Pts',(1.5915537976266,1.75849222743307,16.2820944354729));
#95550=CARTESIAN_POINT('Ctrl Pts',(1.57581058967376,1.7725984843435,16.2834997479155));
#95551=CARTESIAN_POINT('Ctrl Pts',(1.56885403650617,1.7787583897592,16.2841191777095));
#95552=CARTESIAN_POINT('Ctrl Pts',(1.55407324730291,1.79169235885959,16.2854321602534));
#95553=CARTESIAN_POINT('Ctrl Pts',(1.54624052995704,1.79845638935291,16.2861261112714));
#95554=CARTESIAN_POINT('Ctrl Pts',(1.52525745687911,1.81633815270661,16.2879804538177));
#95555=CARTESIAN_POINT('Ctrl Pts',(1.51203007067873,1.82736412156763,16.289144564247));
#95556=CARTESIAN_POINT('Ctrl Pts',(1.44682628597602,1.88052345777757,16.2948607314237));
#95557=CARTESIAN_POINT('Ctrl Pts',(1.39320766631885,1.92058470931037,16.2994943473301));
#95558=CARTESIAN_POINT('Ctrl Pts',(1.13833937031688,2.09471667176372,16.3212380101209));
#95559=CARTESIAN_POINT('Ctrl Pts',(0.919071448557426,2.19975693976898,16.3393601541189));
#95560=CARTESIAN_POINT('Ctrl Pts',(0.651006461277558,2.2809783485855,16.3591881085869));
#95561=CARTESIAN_POINT('Ctrl Pts',(0.61400105479112,2.29121687429302,16.3618725218722));
#95562=CARTESIAN_POINT('Ctrl Pts',(0.566849618394449,2.30303798923258,16.3652130777629));
#95563=CARTESIAN_POINT('Ctrl Pts',(0.556922180982075,2.30545877508622,16.3659119667044));
#95564=CARTESIAN_POINT('Ctrl Pts',(0.541238689485686,2.30917594563744,16.3670087499883));
#95565=CARTESIAN_POINT('Ctrl Pts',(0.535493058692275,2.31051510554239,16.3674090087311));
#95566=CARTESIAN_POINT('Ctrl Pts',(0.525161880149412,2.31288243217529,16.3681258614494));
#95567=CARTESIAN_POINT('Ctrl Pts',(0.520578312860992,2.31391840091876,16.3684428901693));
#95568=CARTESIAN_POINT('Ctrl Pts',(0.509526474841681,2.31638181395521,16.369204904818));
#95569=CARTESIAN_POINT('Ctrl Pts',(0.503055270548331,2.31779579213878,16.3696491173834));
#95570=CARTESIAN_POINT('Ctrl Pts',(0.483199717937665,2.32204721800046,16.3710062930981));
#95571=CARTESIAN_POINT('Ctrl Pts',(0.469796377252478,2.32479604180571,16.3719143817251));
#95572=CARTESIAN_POINT('Ctrl Pts',(0.438573974559455,2.33091822936595,16.3740126108513));
#95573=CARTESIAN_POINT('Ctrl Pts',(0.42073829119197,2.33420355982982,16.3751983089881));
#95574=CARTESIAN_POINT('Ctrl Pts',(0.194010155285068,2.37328356462553,16.3901278026231));
#95575=CARTESIAN_POINT('Ctrl Pts',(-0.0187557240737306,2.38113192331203,
16.402671331518));
#95576=CARTESIAN_POINT('Ctrl Pts',(-0.334738812670418,2.35037736255527,
16.4223808911361));
#95577=CARTESIAN_POINT('Ctrl Pts',(-0.438910140511386,2.33316895835173,
16.4290451302656));
#95578=CARTESIAN_POINT('Ctrl Pts',(-0.559361175096658,2.30491792067688,
16.437128193812));
#95579=CARTESIAN_POINT('Ctrl Pts',(-0.577091036013345,2.3005428600057,16.4383275482758));
#95580=CARTESIAN_POINT('Ctrl Pts',(-0.606046887676739,2.29304186128059,
16.4403028470243));
#95581=CARTESIAN_POINT('Ctrl Pts',(-0.617303710468162,2.29003710198756,
16.4410748842376));
#95582=CARTESIAN_POINT('Ctrl Pts',(-0.637477766645613,2.28449253010937,
16.4424661266822));
#95583=CARTESIAN_POINT('Ctrl Pts',(-0.646403168537081,2.28198312057731,
16.4430843344653));
#95584=CARTESIAN_POINT('Ctrl Pts',(-0.665373257611699,2.27652938769551,
16.4444041314596));
#95585=CARTESIAN_POINT('Ctrl Pts',(-0.675413597174228,2.27357077999345,
16.4451061749616));
#95586=CARTESIAN_POINT('Ctrl Pts',(-0.702433975455513,2.26541385029123,
16.447005164379));
#95587=CARTESIAN_POINT('Ctrl Pts',(-0.719375475673119,2.26009121453313,
16.4482061503907));
#95588=CARTESIAN_POINT('Ctrl Pts',(-0.805512092615517,2.23196244439509,
16.454366626511));
#95589=CARTESIAN_POINT('Ctrl Pts',(-0.87368283898543,2.20616916716439,16.4594235393733));
#95590=CARTESIAN_POINT('Ctrl Pts',(-1.08484824146486,2.11494893451944,16.4756803479646));
#95591=CARTESIAN_POINT('Ctrl Pts',(-1.22257632674005,2.03843100769523,16.4872042469043));
#95592=CARTESIAN_POINT('Ctrl Pts',(-1.44297470466723,1.88556605096541,16.5067547322551));
#95593=CARTESIAN_POINT('Ctrl Pts',(-1.52969607430036,1.81592164463275,16.5147817610046));
#95594=CARTESIAN_POINT('Ctrl Pts',(-1.62059621745061,1.73177049814813,16.5233298979126));
#95595=CARTESIAN_POINT('Ctrl Pts',(-1.62989784121626,1.72301892146699,16.5242062240611));
#95596=CARTESIAN_POINT('Ctrl Pts',(-1.64384600106517,1.70968154611866,16.5255221503006));
#95597=CARTESIAN_POINT('Ctrl Pts',(-1.64854485659463,1.70515117299054,16.5259657797996));
#95598=CARTESIAN_POINT('Ctrl Pts',(-1.65694358403618,1.69698642231767,16.5267592006612));
#95599=CARTESIAN_POINT('Ctrl Pts',(-1.66065027601395,1.69335927099031,16.5271095308544));
#95600=CARTESIAN_POINT('Ctrl Pts',(-1.6678577292978,1.68626005284801,16.5277910406233));
#95601=CARTESIAN_POINT('Ctrl Pts',(-1.67135954290541,1.68278924719491,16.5281223125147));
#95602=CARTESIAN_POINT('Ctrl Pts',(-1.68138178448826,1.67279360509633,16.5290709520292));
#95603=CARTESIAN_POINT('Ctrl Pts',(-1.68787509809914,1.66624152231348,16.5296862201383));
#95604=CARTESIAN_POINT('Ctrl Pts',(-1.71846549912924,1.63501193218469,16.5325889019886));
#95605=CARTESIAN_POINT('Ctrl Pts',(-1.74206207247801,1.60984711521785,16.5348401721584));
#95606=CARTESIAN_POINT('Ctrl Pts',(-1.80817422454824,1.53618432548653,16.5412150867873));
#95607=CARTESIAN_POINT('Ctrl Pts',(-1.849273920515,1.48645334095125,16.545262535052));
#95608=CARTESIAN_POINT('Ctrl Pts',(-1.94302570206359,1.36309562775726,16.5548732788437));
#95609=CARTESIAN_POINT('Ctrl Pts',(-1.99359047065856,1.28801258521187,16.5603847697278));
#95610=CARTESIAN_POINT('Ctrl Pts',(-2.11719378615471,1.07968811971746,16.5752535464667));
#95611=CARTESIAN_POINT('Ctrl Pts',(-2.18192304514981,0.94203946141935,16.5846709892642));
#95612=CARTESIAN_POINT('Ctrl Pts',(-2.23943589762864,0.781334409869855,
16.5958143438064));
#95613=CARTESIAN_POINT('Ctrl Pts',(-2.24560219951976,0.763431285058992,
16.5970572451884));
#95614=CARTESIAN_POINT('Ctrl Pts',(-2.2552792524472,0.734203025621577,16.5990897366829));
#95615=CARTESIAN_POINT('Ctrl Pts',(-2.25892068699309,0.722921787321626,
16.5998750219936));
#95616=CARTESIAN_POINT('Ctrl Pts',(-2.26526550212029,0.702749330666586,
16.6012808723589));
#95617=CARTESIAN_POINT('Ctrl Pts',(-2.26800150477372,0.693868566060845,
16.6019003531756));
#95618=CARTESIAN_POINT('Ctrl Pts',(-2.2736728708009,0.675067964194774,16.603213100316));
#95619=CARTESIAN_POINT('Ctrl Pts',(-2.27659565562608,0.665144566690179,
16.6039067628791));
#95620=CARTESIAN_POINT('Ctrl Pts',(-2.28420520425342,0.638670901854381,
16.6057595160973));
#95621=CARTESIAN_POINT('Ctrl Pts',(-2.2887769261295,0.622088491461285,16.6069223144217));
#95622=CARTESIAN_POINT('Ctrl Pts',(-2.29840021455703,0.585640368256932,
16.6094836446329));
#95623=CARTESIAN_POINT('Ctrl Pts',(-2.30337538619074,0.565756106135499,
16.6108845348272));
#95624=CARTESIAN_POINT('Ctrl Pts',(-2.33709238449061,0.423175572073484,
16.6209568971406));
#95625=CARTESIAN_POINT('Ctrl Pts',(-2.35624693458251,0.298533170639224,
16.6299219917352));
#95626=CARTESIAN_POINT('Ctrl Pts',(-2.36542650336594,0.17307662948527,16.639047070016));
#95627=CARTESIAN_POINT('Origin',(0.,0.,-1.84858989190503));
#95628=CARTESIAN_POINT('',(-2.36542646972628,0.173077089235633,17.8377309811821));
#95629=CARTESIAN_POINT('',(-2.3692863196969,0.173352773124932,17.639803316701));
#95630=CARTESIAN_POINT('',(-2.36542649454111,0.173076750093529,-1.84858989190503));
#95631=CARTESIAN_POINT('Ctrl Pts',(-2.36542646972629,0.173077089235462,
17.8377309811821));
#95632=CARTESIAN_POINT('Ctrl Pts',(-2.35433609142309,0.324648129131858,
17.8267093548572));
#95633=CARTESIAN_POINT('Ctrl Pts',(-2.3286947503669,0.474925913114985,17.8154678917761));
#95634=CARTESIAN_POINT('Ctrl Pts',(-2.28012575711333,0.653692848604288,
17.8022638581209));
#95635=CARTESIAN_POINT('Ctrl Pts',(-2.27080606778965,0.685366943566306,
17.7999323289627));
#95636=CARTESIAN_POINT('Ctrl Pts',(-2.25431165770714,0.737388501923027,
17.7961271714833));
#95637=CARTESIAN_POINT('Ctrl Pts',(-2.24751546673184,0.75785035640701,17.7946367544241));
#95638=CARTESIAN_POINT('Ctrl Pts',(-2.23785557246991,0.785660602118027,
17.7926223524087));
#95639=CARTESIAN_POINT('Ctrl Pts',(-2.23523311809341,0.7930908253336,17.7920852604333));
#95640=CARTESIAN_POINT('Ctrl Pts',(-2.23077327396355,0.80552909045965,17.7911881860162));
#95641=CARTESIAN_POINT('Ctrl Pts',(-2.22895594963453,0.810544194819505,
17.7908270397563));
#95642=CARTESIAN_POINT('Ctrl Pts',(-2.22547882620366,0.820039561875361,
17.7901443702398));
#95643=CARTESIAN_POINT('Ctrl Pts',(-2.22382238849385,0.824520996940868,
17.7898226450493));
#95644=CARTESIAN_POINT('Ctrl Pts',(-2.21944722740887,0.836248746821881,
17.7889818519484));
#95645=CARTESIAN_POINT('Ctrl Pts',(-2.21670652829653,0.843486889911999,
17.7884640834377));
#95646=CARTESIAN_POINT('Ctrl Pts',(-2.20706737918103,0.868572247713667,
17.7866732223519));
#95647=CARTESIAN_POINT('Ctrl Pts',(-2.19998820639566,0.886349883081612,
17.7854103741261));
#95648=CARTESIAN_POINT('Ctrl Pts',(-2.1453116973185,1.01896436464643,17.7760234310807));
#95649=CARTESIAN_POINT('Ctrl Pts',(-2.08896038534084,1.13000157716791,17.7683472537538));
#95650=CARTESIAN_POINT('Ctrl Pts',(-1.96871125148398,1.32691025881613,17.7541876848687));
#95651=CARTESIAN_POINT('Ctrl Pts',(-1.90722268800142,1.41386547461939,17.7477078053922));
#95652=CARTESIAN_POINT('Ctrl Pts',(-1.79888601085289,1.54708622654022,17.7370147231516));
#95653=CARTESIAN_POINT('Ctrl Pts',(-1.75559066508366,1.59604733071329,17.7328977553571));
#95654=CARTESIAN_POINT('Ctrl Pts',(-1.69084743149421,1.66343740401887,17.7268984897846));
#95655=CARTESIAN_POINT('Ctrl Pts',(-1.6710043622939,1.68336964181303,17.7250794317993));
#95656=CARTESIAN_POINT('Ctrl Pts',(-1.63512468469334,1.71815094986002,17.721820391858));
#95657=CARTESIAN_POINT('Ctrl Pts',(-1.61922825028689,1.73314028342154,17.7203865462583));
#95658=CARTESIAN_POINT('Ctrl Pts',(-1.59486518331644,1.75548534558101,17.718202696384));
#95659=CARTESIAN_POINT('Ctrl Pts',(-1.58654943297323,1.76300443587321,17.7174596446547));
#95660=CARTESIAN_POINT('Ctrl Pts',(-1.57807502812236,1.7705584678841,17.7167046801618));
#95661=CARTESIAN_POINT('Ctrl Pts',(-1.57796924195418,1.77065274800735,17.7166952562797));
#95662=CARTESIAN_POINT('Ctrl Pts',(-1.57775371135024,1.77084480133748,17.7166760566192));
#95663=CARTESIAN_POINT('Ctrl Pts',(-1.57764396627176,1.77094257382608,17.7166662808104));
#95664=CARTESIAN_POINT('Ctrl Pts',(-1.57742026114263,1.77114183664773,17.7166463545115));
#95665=CARTESIAN_POINT('Ctrl Pts',(-1.57730630039247,1.7712433261778,17.7166362039889));
#95666=CARTESIAN_POINT('Ctrl Pts',(-1.57707388492029,1.77145026719746,17.7166155035019));
#95667=CARTESIAN_POINT('Ctrl Pts',(-1.57695542941263,1.77155571780781,17.7166049535006));
#95668=CARTESIAN_POINT('Ctrl Pts',(-1.57671372063203,1.77177084660838,17.7165834270993));
#95669=CARTESIAN_POINT('Ctrl Pts',(-1.57659046649173,1.7718805238187,17.7165724506587));
#95670=CARTESIAN_POINT('Ctrl Pts',(-1.57633882911922,1.77210439529776,17.7165500419834));
#95671=CARTESIAN_POINT('Ctrl Pts',(-1.57621044492265,1.77221858847584,17.7165386097033));
#95672=CARTESIAN_POINT('Ctrl Pts',(-1.57594818542865,1.77245180792992,17.7165152572364));
#95673=CARTESIAN_POINT('Ctrl Pts',(-1.57581430905966,1.77257083298599,17.7165033369993));
#95674=CARTESIAN_POINT('Ctrl Pts',(-1.57554066900929,1.77281406181197,17.7164789734773));
#95675=CARTESIAN_POINT('Ctrl Pts',(-1.57540090411789,1.77293826422834,17.7164665301352));
#95676=CARTESIAN_POINT('Ctrl Pts',(-1.57511505250619,1.77319222647951,17.7164410818713));
#95677=CARTESIAN_POINT('Ctrl Pts',(-1.57496896443893,1.77332198478818,17.7164280768862));
#95678=CARTESIAN_POINT('Ctrl Pts',(-1.57466998907782,1.77358747452592,17.7164014630098));
#95679=CARTESIAN_POINT('Ctrl Pts',(-1.57451710027174,1.77372320423718,17.7163878540474));
#95680=CARTESIAN_POINT('Ctrl Pts',(-1.57428024895467,1.77393341838099,17.7163667725361));
#95681=CARTESIAN_POINT('Ctrl Pts',(-1.57419629867085,1.77400791665332,17.7163593005636));
#95682=CARTESIAN_POINT('Ctrl Pts',(-1.57400770356189,1.77417525380031,17.7163425152024));
#95683=CARTESIAN_POINT('Ctrl Pts',(-1.57390305583108,1.77426808935831,17.7163332016773));
#95684=CARTESIAN_POINT('Ctrl Pts',(-1.57366747479444,1.77447704180718,17.7163122360133));
#95685=CARTESIAN_POINT('Ctrl Pts',(-1.57353653685349,1.77459315346188,17.7163005836555));
#95686=CARTESIAN_POINT('Ctrl Pts',(-1.57324100163432,1.77485516638854,17.7162742847562));
#95687=CARTESIAN_POINT('Ctrl Pts',(-1.57307639692571,1.77500105924325,17.716259637864));
#95688=CARTESIAN_POINT('Ctrl Pts',(-1.57270364763563,1.77533134274638,17.71622647172));
#95689=CARTESIAN_POINT('Ctrl Pts',(-1.57249549094759,1.77551571966386,17.7162079518969));
#95690=CARTESIAN_POINT('Ctrl Pts',(-1.57202213970447,1.77593484683839,17.7161658406272));
#95691=CARTESIAN_POINT('Ctrl Pts',(-1.57175692502872,1.77616957426928,17.7161422482304));
#95692=CARTESIAN_POINT('Ctrl Pts',(-1.56463521320983,1.78246977917069,17.7155087889948));
#95693=CARTESIAN_POINT('Ctrl Pts',(-1.55774379341371,1.78849549456921,17.7148972734048));
#95694=CARTESIAN_POINT('Ctrl Pts',(-1.54201311578825,1.80209018448958,17.7135045891922));
#95695=CARTESIAN_POINT('Ctrl Pts',(-1.53315274472992,1.8096342545427,17.7127224117717));
#95696=CARTESIAN_POINT('Ctrl Pts',(-1.51006277652303,1.82900266905013,17.710689661714));
#95697=CARTESIAN_POINT('Ctrl Pts',(-1.49574992765401,1.84072607207892,17.7094350325183));
#95698=CARTESIAN_POINT('Ctrl Pts',(-1.39042105029566,1.92495945108253,17.7002393381218));
#95699=CARTESIAN_POINT('Ctrl Pts',(-1.29432948786212,1.990839803525,17.6920380063034));
#95700=CARTESIAN_POINT('Ctrl Pts',(-1.05114855366332,2.13249654360722,17.6717593279395));
#95701=CARTESIAN_POINT('Ctrl Pts',(-0.900212777535253,2.20047013307773,
17.6595330368863));
#95702=CARTESIAN_POINT('Ctrl Pts',(-0.688180678851421,2.27046084061658,
17.6435385405596));
#95703=CARTESIAN_POINT('Ctrl Pts',(-0.632257361532253,2.2866650437756,17.639429155624));
#95704=CARTESIAN_POINT('Ctrl Pts',(-0.56516258737836,2.30345595002304,17.6346702208398));
#95705=CARTESIAN_POINT('Ctrl Pts',(-0.55451723111309,2.30604178539709,17.6339202327329));
#95706=CARTESIAN_POINT('Ctrl Pts',(-0.538005900301467,2.30993156026769,
17.6327652148397));
#95707=CARTESIAN_POINT('Ctrl Pts',(-0.53215241988171,2.31128707994899,17.6323573442527));
#95708=CARTESIAN_POINT('Ctrl Pts',(-0.521304348141874,2.31375582607862,
17.6316044871929));
#95709=CARTESIAN_POINT('Ctrl Pts',(-0.516311338804347,2.31487512587566,
17.6312591694107));
#95710=CARTESIAN_POINT('Ctrl Pts',(-0.504953656398979,2.31738264019071,
17.6304763567351));
#95711=CARTESIAN_POINT('Ctrl Pts',(-0.498586867895889,2.31876079704201,
17.6300394396708));
#95712=CARTESIAN_POINT('Ctrl Pts',(-0.482016193407498,2.3222762832845,17.6289070436771));
#95713=CARTESIAN_POINT('Ctrl Pts',(-0.471803614392826,2.32437262631441,
17.6282138237781));
#95714=CARTESIAN_POINT('Ctrl Pts',(-0.40357841149047,2.33790907062999,17.6236119196753));
#95715=CARTESIAN_POINT('Ctrl Pts',(-0.34516368633506,2.3472447137581,17.6198119929584));
#95716=CARTESIAN_POINT('Ctrl Pts',(-0.216685226020823,2.36287654137471,
17.6116393278272));
#95717=CARTESIAN_POINT('Ctrl Pts',(-0.146567955237341,2.3682603226395,17.6072973634294));
#95718=CARTESIAN_POINT('Ctrl Pts',(0.0195230748374318,2.37360711387456,
17.5970883317019));
#95719=CARTESIAN_POINT('Ctrl Pts',(0.115455206019669,2.37087782733981,17.5912489224489));
#95720=CARTESIAN_POINT('Ctrl Pts',(0.325226749636935,2.35214521247095,17.5782097301718));
#95721=CARTESIAN_POINT('Ctrl Pts',(0.438589678738733,2.33366520341996,17.5709818005324));
#95722=CARTESIAN_POINT('Ctrl Pts',(0.569278799271721,2.30249993995939,17.5621987043796));
#95723=CARTESIAN_POINT('Ctrl Pts',(0.58833839366314,2.29770368431307,17.5609066166919));
#95724=CARTESIAN_POINT('Ctrl Pts',(0.617760143383031,2.28990977160232,17.5588937324179));
#95725=CARTESIAN_POINT('Ctrl Pts',(0.628165464648626,2.28707728319701,17.5581782815323));
#95726=CARTESIAN_POINT('Ctrl Pts',(0.646451802346504,2.28196525640271,17.5569144875278));
#95727=CARTESIAN_POINT('Ctrl Pts',(0.654341042082733,2.27971558794437,17.5563671244791));
#95728=CARTESIAN_POINT('Ctrl Pts',(0.672328591468121,2.27448525751791,17.5551141872217));
#95729=CARTESIAN_POINT('Ctrl Pts',(0.682418983410505,2.27147820734345,17.5544077607304));
#95730=CARTESIAN_POINT('Ctrl Pts',(0.709694355689285,2.26315169626541,17.5524883451438));
#95731=CARTESIAN_POINT('Ctrl Pts',(0.726839089474695,2.25770383036204,17.5512711742375));
#95732=CARTESIAN_POINT('Ctrl Pts',(0.812207946496449,2.22950407674143,17.5451557117674));
#95733=CARTESIAN_POINT('Ctrl Pts',(0.879427727219195,2.20385460875232,17.5401627867531));
#95734=CARTESIAN_POINT('Ctrl Pts',(1.11900388236409,2.09973110811302,17.5217007694263));
#95735=CARTESIAN_POINT('Ctrl Pts',(1.28296330421368,2.00375369913688,17.5077009430674));
#95736=CARTESIAN_POINT('Ctrl Pts',(1.47760950558301,1.85604441957882,17.4900231277926));
#95737=CARTESIAN_POINT('Ctrl Pts',(1.52030845028555,1.82123414166839,17.4860758532282));
#95738=CARTESIAN_POINT('Ctrl Pts',(1.57739753167688,1.77128395627919,17.4807397311835));
#95739=CARTESIAN_POINT('Ctrl Pts',(1.59285578607418,1.75739589706813,17.4792886599954));
#95740=CARTESIAN_POINT('Ctrl Pts',(1.61928142281692,1.73301930254124,17.476800182791));
#95741=CARTESIAN_POINT('Ctrl Pts',(1.63033414825874,1.72262556130442,17.4757568983895));
#95742=CARTESIAN_POINT('Ctrl Pts',(1.64623112028907,1.70738632824647,17.4742537447551));
#95743=CARTESIAN_POINT('Ctrl Pts',(1.65115503163474,1.70262504380405,17.4737877895056));
#95744=CARTESIAN_POINT('Ctrl Pts',(1.65974635176797,1.69424515703345,17.4729742438012));
#95745=CARTESIAN_POINT('Ctrl Pts',(1.66342268553847,1.69063584951031,17.4726259462045));
#95746=CARTESIAN_POINT('Ctrl Pts',(1.67120970125448,1.6829408146612,17.4718878669036));
#95747=CARTESIAN_POINT('Ctrl Pts',(1.67531717888695,1.67885198965874,17.471498335297));
#95748=CARTESIAN_POINT('Ctrl Pts',(1.68645704955735,1.66768111163502,17.4704411691226));
#95749=CARTESIAN_POINT('Ctrl Pts',(1.69345989505657,1.66056955975671,17.4697758173114));
#95750=CARTESIAN_POINT('Ctrl Pts',(1.7260841497601,1.62701784914539,17.4666711688291));
#95751=CARTESIAN_POINT('Ctrl Pts',(1.75113416368911,1.60002596348554,17.4642727995735));
#95752=CARTESIAN_POINT('Ctrl Pts',(1.87960477562636,1.45496304280099,17.4518241095926));
#95753=CARTESIAN_POINT('Ctrl Pts',(1.97175382898818,1.32741451748516,17.4423489501649));
#95754=CARTESIAN_POINT('Ctrl Pts',(2.12486389866136,1.06394511276895,17.4236333799158));
#95755=CARTESIAN_POINT('Ctrl Pts',(2.18698836566015,0.929569025539528,17.4144483322207));
#95756=CARTESIAN_POINT('Ctrl Pts',(2.24303577069241,0.770978917000507,17.403461607158));
#95757=CARTESIAN_POINT('Ctrl Pts',(2.24961292066846,0.751571435560694,17.4021152578435));
#95758=CARTESIAN_POINT('Ctrl Pts',(2.25932101719623,0.721655565094474,17.4000359799522));
#95759=CARTESIAN_POINT('Ctrl Pts',(2.26263205484322,0.711206292794496,17.3993089840294));
#95760=CARTESIAN_POINT('Ctrl Pts',(2.2685354212722,0.692117376723466,17.3979793989934));
#95761=CARTESIAN_POINT('Ctrl Pts',(2.27115113726744,0.683485134105364,17.3973775899567));
#95762=CARTESIAN_POINT('Ctrl Pts',(2.27675644308931,0.664599302680216,17.3960596266192));
#95763=CARTESIAN_POINT('Ctrl Pts',(2.27972612666063,0.654340060825932,17.3953428366152));
#95764=CARTESIAN_POINT('Ctrl Pts',(2.28769182018423,0.626108736586486,17.3933678873121));
#95765=CARTESIAN_POINT('Ctrl Pts',(2.29254516883256,0.6080975483065,17.3921051310474));
#95766=CARTESIAN_POINT('Ctrl Pts',(2.31745450270745,0.511117359469357,17.3852895531852));
#95767=CARTESIAN_POINT('Ctrl Pts',(2.3336414585999,0.431220501594079,17.3796138496288));
#95768=CARTESIAN_POINT('Ctrl Pts',(2.37502849286606,0.154366110544676,17.3597334684906));
#95769=CARTESIAN_POINT('Ctrl Pts',(2.37961487791347,-0.0448013889349336,
17.3449891624996));
#95770=CARTESIAN_POINT('Ctrl Pts',(2.35507670675476,-0.283837818392776,
17.3277399118691));
#95771=CARTESIAN_POINT('Ctrl Pts',(2.3497003325302,-0.325359777074311,17.3247640247835));
#95772=CARTESIAN_POINT('Ctrl Pts',(2.34056005924066,-0.383763281885125,
17.3206256455705));
#95773=CARTESIAN_POINT('Ctrl Pts',(2.33770680830536,-0.40077745205299,17.3194257889684));
#95774=CARTESIAN_POINT('Ctrl Pts',(2.33235686347936,-0.430675860652665,
17.3173291742773));
#95775=CARTESIAN_POINT('Ctrl Pts',(2.32993843519552,-0.443573154713716,
17.3164286586334));
#95776=CARTESIAN_POINT('Ctrl Pts',(2.32617018494521,-0.462787248677799,
17.3150935836234));
#95777=CARTESIAN_POINT('Ctrl Pts',(2.32490144887061,-0.46911941169255,17.3146546543047));
#95778=CARTESIAN_POINT('Ctrl Pts',(2.32258184942387,-0.480455783271049,
17.3138708350069));
#95779=CARTESIAN_POINT('Ctrl Pts',(2.32154065679897,-0.485461829003278,
17.3135254097795));
#95780=CARTESIAN_POINT('Ctrl Pts',(2.31923187143544,-0.496385140240768,
17.3127732263469));
#95781=CARTESIAN_POINT('Ctrl Pts',(2.31795782132636,-0.502300927296729,
17.3123668407005));
#95782=CARTESIAN_POINT('Ctrl Pts',(2.31433689237911,-0.518806770702629,
17.3112355363785));
#95783=CARTESIAN_POINT('Ctrl Pts',(2.31193994951072,-0.529385868586778,
17.3105134041528));
#95784=CARTESIAN_POINT('Ctrl Pts',(2.29827149657482,-0.587848655292425,
17.3065372027048));
#95785=CARTESIAN_POINT('Ctrl Pts',(2.28558404076224,-0.63539305195678,17.3033574358266));
#95786=CARTESIAN_POINT('Ctrl Pts',(2.26157897847777,-0.715282778716147,
17.2980527197474));
#95787=CARTESIAN_POINT('Ctrl Pts',(2.25102375161325,-0.747837669828325,
17.2959020890173));
#95788=CARTESIAN_POINT('Ctrl Pts',(2.17958815624332,-0.952924262141285,
17.2823588543075));
#95789=CARTESIAN_POINT('Ctrl Pts',(2.09962195591142,-1.11815047311524,17.2714208237175));
#95790=CARTESIAN_POINT('Ctrl Pts',(1.95961240145338,-1.33835688619862,17.2550191426764));
#95791=CARTESIAN_POINT('Ctrl Pts',(1.91455304692249,-1.40205725600445,17.2500337920764));
#95792=CARTESIAN_POINT('Ctrl Pts',(1.85541886409564,-1.47747692176913,17.2437568780338));
#95793=CARTESIAN_POINT('Ctrl Pts',(1.84423765095556,-1.49141029679071,17.2425807689984));
#95794=CARTESIAN_POINT('Ctrl Pts',(1.82630183417624,-1.51325073098052,17.2407101865838));
#95795=CARTESIAN_POINT('Ctrl Pts',(1.8196506441849,-1.52124215415385,17.2400198971673));
#95796=CARTESIAN_POINT('Ctrl Pts',(1.80706196498811,-1.53616679964939,17.2387195448843));
#95797=CARTESIAN_POINT('Ctrl Pts',(1.80113655824584,-1.54311000132188,17.2381099847555));
#95798=CARTESIAN_POINT('Ctrl Pts',(1.78774599347641,-1.5586184314928,17.2367379488071));
#95799=CARTESIAN_POINT('Ctrl Pts',(1.78025911305771,-1.56716452063316,17.2359745796424));
#95800=CARTESIAN_POINT('Ctrl Pts',(1.76102248615991,-1.58880692021838,17.2340224906222));
#95801=CARTESIAN_POINT('Ctrl Pts',(1.74918805649212,-1.60182668860903,17.2328302317064));
#95802=CARTESIAN_POINT('Ctrl Pts',(1.67442758937374,-1.68225870267956,17.2253504879774));
#95803=CARTESIAN_POINT('Ctrl Pts',(1.60776739376707,-1.74607622166779,17.2189026160298));
#95804=CARTESIAN_POINT('Ctrl Pts',(1.37835242948756,-1.94140935884335,17.197396409941));
#95805=CARTESIAN_POINT('Ctrl Pts',(1.20192720540499,-2.05530652664814,17.1817923076774));
#95806=CARTESIAN_POINT('Ctrl Pts',(0.987580518264483,-2.15654003360007,
17.1649780500708));
#95807=CARTESIAN_POINT('Ctrl Pts',(0.962081827807614,-2.16803572506896,
17.1630112525459));
#95808=CARTESIAN_POINT('Ctrl Pts',(0.918887297376993,-2.18659710169309,
17.1597420799682));
#95809=CARTESIAN_POINT('Ctrl Pts',(0.901299383690034,-2.19390524625424,
17.1584280696258));
#95810=CARTESIAN_POINT('Ctrl Pts',(0.876660263789917,-2.20379698805432,
17.1566128866317));
#95811=CARTESIAN_POINT('Ctrl Pts',(0.869682518015558,-2.20655992540975,
17.1561016716897));
#95812=CARTESIAN_POINT('Ctrl Pts',(0.857792429938606,-2.21120281111398,
17.1552355262774));
#95813=CARTESIAN_POINT('Ctrl Pts',(0.852886769861896,-2.21309961019504,
17.1548796005022));
#95814=CARTESIAN_POINT('Ctrl Pts',(0.843442786571962,-2.21671510958756,
17.1541972016762));
#95815=CARTESIAN_POINT('Ctrl Pts',(0.838905468569996,-2.21843621210642,
17.153870579638));
#95816=CARTESIAN_POINT('Ctrl Pts',(0.828007306321643,-2.22253190326943,
17.1530889496392));
#95817=CARTESIAN_POINT('Ctrl Pts',(0.821641439425255,-2.22489314535519,
17.1526347302468));
#95818=CARTESIAN_POINT('Ctrl Pts',(0.798496496010837,-2.23336523715348,
17.1509914919503));
#95819=CARTESIAN_POINT('Ctrl Pts',(0.781658158372099,-2.23931407075631,
17.1498116217844));
#95820=CARTESIAN_POINT('Ctrl Pts',(0.60851605554866,-2.29829259239294,17.137823106008));
#95821=CARTESIAN_POINT('Ctrl Pts',(0.447124653813533,-2.33506683080722,
17.127820727477));
#95822=CARTESIAN_POINT('Ctrl Pts',(0.121065654715695,-2.37428081666814,
17.1076880548794));
#95823=CARTESIAN_POINT('Ctrl Pts',(-0.0426254971908174,-2.37698100552649,
17.0976014020263));
#95824=CARTESIAN_POINT('Ctrl Pts',(-0.225905277401668,-2.36105766667142,
17.0855872106768));
#95825=CARTESIAN_POINT('Ctrl Pts',(-0.246501426800852,-2.35899629111795,
17.0842274386187));
#95826=CARTESIAN_POINT('Ctrl Pts',(-0.278002236623175,-2.35542648461675,
17.0821317588908));
#95827=CARTESIAN_POINT('Ctrl Pts',(-0.288928123614085,-2.35411123365992,
17.0814019333868));
#95828=CARTESIAN_POINT('Ctrl Pts',(-0.307998871968717,-2.3516807466931,
17.0801227237711));
#95829=CARTESIAN_POINT('Ctrl Pts',(-0.316147888811791,-2.35059910426449,
17.0795744095148));
#95830=CARTESIAN_POINT('Ctrl Pts',(-0.334542937624182,-2.34806009065543,
17.0783327531875));
#95831=CARTESIAN_POINT('Ctrl Pts',(-0.344785329478392,-2.3465779844528,
17.0776386385551));
#95832=CARTESIAN_POINT('Ctrl Pts',(-0.372463931280955,-2.34238767811711,
17.0757552544318));
#95833=CARTESIAN_POINT('Ctrl Pts',(-0.38987986468718,-2.3395518964928,17.0745619696391));
#95834=CARTESIAN_POINT('Ctrl Pts',(-0.471086991365619,-2.32539727442062,
17.0689582708733));
#95835=CARTESIAN_POINT('Ctrl Pts',(-0.534423281641454,-2.31166299096289,
17.0644720280644));
#95836=CARTESIAN_POINT('Ctrl Pts',(-0.805868774350716,-2.24104922422023,
17.0447256355332));
#95837=CARTESIAN_POINT('Ctrl Pts',(-1.00623010420782,-2.15851843572842,
17.028685532724));
#95838=CARTESIAN_POINT('Ctrl Pts',(-1.22979114553509,-2.02846253828057,
17.0101046096524));
#95839=CARTESIAN_POINT('Ctrl Pts',(-1.26636162998509,-2.00583529196605,
17.0070456527621));
#95840=CARTESIAN_POINT('Ctrl Pts',(-1.32413676887402,-1.9678776936457,17.0022039808885));
#95841=CARTESIAN_POINT('Ctrl Pts',(-1.34573725576179,-1.95316977811418,
17.0003917379912));
#95842=CARTESIAN_POINT('Ctrl Pts',(-1.3740180531115,-1.93322122462922,16.998020786177));
#95843=CARTESIAN_POINT('Ctrl Pts',(-1.38091863397588,-1.92829812153926,
16.9974424108545));
#95844=CARTESIAN_POINT('Ctrl Pts',(-1.39222248376649,-1.92014178025695,
16.9964954065984));
#95845=CARTESIAN_POINT('Ctrl Pts',(-1.39664116528902,-1.91693019110469,
16.9961253318837));
#95846=CARTESIAN_POINT('Ctrl Pts',(-1.40527449272274,-1.91060961224155,
16.9954025501633));
#95847=CARTESIAN_POINT('Ctrl Pts',(-1.40948998778683,-1.90750189134353,
16.9950497646464));
#95848=CARTESIAN_POINT('Ctrl Pts',(-1.41984591751478,-1.89981428358279,
16.9941833415555));
#95849=CARTESIAN_POINT('Ctrl Pts',(-1.42597459533989,-1.89521850960284,
16.9936707991329));
#95850=CARTESIAN_POINT('Ctrl Pts',(-1.44695423188662,-1.87932691456675,
16.9919165774579));
#95851=CARTESIAN_POINT('Ctrl Pts',(-1.46169456980216,-1.86788523184674,
16.9906845928065));
#95852=CARTESIAN_POINT('Ctrl Pts',(-1.59302151266226,-1.76344041181769,
16.9796975738021));
#95853=CARTESIAN_POINT('Ctrl Pts',(-1.70074619987023,-1.65979370056975,
16.9705944473841));
#95854=CARTESIAN_POINT('Ctrl Pts',(-1.91401455416183,-1.41187017630449,
16.9505575010884));
#95855=CARTESIAN_POINT('Ctrl Pts',(-2.01444731264387,-1.26444433988212,
16.9396415779262));
#95856=CARTESIAN_POINT('Ctrl Pts',(-2.10720081892097,-1.08873247820053,
16.9266682741967));
#95857=CARTESIAN_POINT('Ctrl Pts',(-2.116700003558,-1.07014706904861,16.9252972908358));
#95858=CARTESIAN_POINT('Ctrl Pts',(-2.1308470764969,-1.04154246286506,16.9231879185604));
#95859=CARTESIAN_POINT('Ctrl Pts',(-2.13567249460642,-1.03161182338023,
16.9224557380088));
#95860=CARTESIAN_POINT('Ctrl Pts',(-2.14397083083727,-1.01422619344112,
16.9211739599357));
#95861=CARTESIAN_POINT('Ctrl Pts',(-2.14747466637575,-1.00678609907083,
16.9206254469545));
#95862=CARTESIAN_POINT('Ctrl Pts',(-2.15528899086396,-0.989966655850969,
16.9193854105219));
#95863=CARTESIAN_POINT('Ctrl Pts',(-2.15957706202411,-0.980577136772298,
16.9186931265382));
#95864=CARTESIAN_POINT('Ctrl Pts',(-2.17097888841599,-0.955173174320616,
16.9168198601892));
#95865=CARTESIAN_POINT('Ctrl Pts',(-2.17797656337175,-0.939107654890715,
16.9156349359843));
#95866=CARTESIAN_POINT('Ctrl Pts',(-2.20966887322561,-0.864087361306736,
16.9100993817005));
#95867=CARTESIAN_POINT('Ctrl Pts',(-2.23214976807925,-0.80423227683552,
16.9056750172134));
#95868=CARTESIAN_POINT('Ctrl Pts',(-2.31339341021456,-0.55814743750153,
16.8874400430945));
#95869=CARTESIAN_POINT('Ctrl Pts',(-2.35146859172631,-0.365913477462063,
16.8730126545402));
#95870=CARTESIAN_POINT('Ctrl Pts',(-2.36970278055722,-0.114010354654363,
16.8547207567684));
#95871=CARTESIAN_POINT('Ctrl Pts',(-2.37176750132454,-0.0566522349982106,
16.8506032362722));
#95872=CARTESIAN_POINT('Ctrl Pts',(-2.37174026352844,0.032083723484378,
16.844356528475));
#95873=CARTESIAN_POINT('Ctrl Pts',(-2.37110883104935,0.063438111953284,
16.842173191473));
#95874=CARTESIAN_POINT('Ctrl Pts',(-2.36947960879403,0.104177965148921,
16.8393750394647));
#95875=CARTESIAN_POINT('Ctrl Pts',(-2.36904748386543,0.113581211687271,
16.83873188062));
#95876=CARTESIAN_POINT('Ctrl Pts',(-2.36826538448301,0.128643995826007,
16.8377061957126));
#95877=CARTESIAN_POINT('Ctrl Pts',(-2.36795108362451,0.134305161086325,
16.8373217400156));
#95878=CARTESIAN_POINT('Ctrl Pts',(-2.36731020592937,0.14514608704302,16.8365875747979));
#95879=CARTESIAN_POINT('Ctrl Pts',(-2.36698692713815,0.150325929018152,
16.8362376945008));
#95880=CARTESIAN_POINT('Ctrl Pts',(-2.36626168529946,0.16136347921972,16.8354940160912));
#95881=CARTESIAN_POINT('Ctrl Pts',(-2.36585496609515,0.16722086265911,16.83510048246));
#95882=CARTESIAN_POINT('Ctrl Pts',(-2.36542649454112,0.173076750093436,
16.8347081153257));
#95883=CARTESIAN_POINT('',(-2.37247048654875,-0.00211540104443233,16.651410108095));
#95884=CARTESIAN_POINT('Ctrl Pts',(-2.36542650336594,0.173076629485272,
16.639047070016));
#95885=CARTESIAN_POINT('Ctrl Pts',(-2.36968866402696,0.114825970114507,
16.643283930221));
#95886=CARTESIAN_POINT('Ctrl Pts',(-2.37180047394265,0.0563995970809621,
16.6475524590594));
#95887=CARTESIAN_POINT('Ctrl Pts',(-2.37174908437069,-0.00208405537486423,
16.6518242564532));
#95888=CARTESIAN_POINT('Ctrl Pts',(-2.37247048654875,-0.00211540104443233,
16.651410108095));
#95889=CARTESIAN_POINT('Ctrl Pts',(-2.37394798832961,-0.162106932516699,
16.6621578139988));
#95890=CARTESIAN_POINT('Ctrl Pts',(-2.28621603133195,-1.10891487060638,
16.7258694983972));
#95891=CARTESIAN_POINT('Ctrl Pts',(-1.013610398569,-2.61441006592229,16.8425451612904));
#95892=CARTESIAN_POINT('Ctrl Pts',(1.64854813367676,-2.2682228911273,17.0014370967742));
#95893=CARTESIAN_POINT('Ctrl Pts',(2.79962146477649,0.157053133829965,17.1603290322581));
#95894=CARTESIAN_POINT('Ctrl Pts',(1.38451763804013,2.43837178109468,17.3192209677419));
#95895=CARTESIAN_POINT('Ctrl Pts',(-1.29965687630912,2.48464042403432,17.4781129032258));
#95896=CARTESIAN_POINT('Ctrl Pts',(-2.30368038220262,0.984080211399787,
17.5849736862122));
#95897=CARTESIAN_POINT('Ctrl Pts',(-2.36829936334429,0.187155604555285,
17.6388704907039));
#95898=CARTESIAN_POINT('Ctrl Pts',(-2.3692863196969,0.173352773124932,17.639803316701));
#95899=CARTESIAN_POINT('Origin',(0.,0.,-1.84858989190503));
#95900=CARTESIAN_POINT('',(-2.36542649320577,0.173076768343595,18.8389943251842));
#95901=CARTESIAN_POINT('',(-2.36542649880512,0.173076691817703,18.6388842277111));
#95902=CARTESIAN_POINT('',(-2.36542649454111,0.173076750093529,-1.84858989190503));
#95903=CARTESIAN_POINT('',(-2.37174930964901,0.0018096075435597,17.8500526884225));
#95904=CARTESIAN_POINT('Ctrl Pts',(-2.36542649320577,0.173076768343595,
18.8389943251842));
#95905=CARTESIAN_POINT('Ctrl Pts',(-2.3638889171336,0.194090698816365,18.837632151699));
#95906=CARTESIAN_POINT('Ctrl Pts',(-2.36207122772979,0.215085357947287,
18.8362618402781));
#95907=CARTESIAN_POINT('Ctrl Pts',(-2.35813192756486,0.254468710188079,
18.8336719300932));
#95908=CARTESIAN_POINT('Ctrl Pts',(-2.35607472795328,0.272859590989085,
18.8324545545264));
#95909=CARTESIAN_POINT('Ctrl Pts',(-2.35249527673793,0.301790306904119,
18.8305261184804));
#95910=CARTESIAN_POINT('Ctrl Pts',(-2.35111685834559,0.312347448399746,
18.8298195964156));
#95911=CARTESIAN_POINT('Ctrl Pts',(-2.34843925734046,0.331832035124003,
18.8285102563322));
#95912=CARTESIAN_POINT('Ctrl Pts',(-2.34716012425922,0.340762075589015,
18.8279080832585));
#95913=CARTESIAN_POINT('Ctrl Pts',(-2.34420835805375,0.360563759872961,
18.8265680757639));
#95914=CARTESIAN_POINT('Ctrl Pts',(-2.3425109868226,0.371431447812002,18.8258294694569));
#95915=CARTESIAN_POINT('Ctrl Pts',(-2.3374059122059,0.402689768436501,18.8236956815773));
#95916=CARTESIAN_POINT('Ctrl Pts',(-2.33380719354624,0.423047732585077,
18.8222944773178));
#95917=CARTESIAN_POINT('Ctrl Pts',(-2.29987265693084,0.601382122486404,
18.8099154572715));
#95918=CARTESIAN_POINT('Ctrl Pts',(-2.25380989835203,0.755907807660723,
18.7984225642131));
#95919=CARTESIAN_POINT('Ctrl Pts',(-2.12844996080835,1.05975764006811,18.7744782758937));
#95920=CARTESIAN_POINT('Ctrl Pts',(-2.04811593198904,1.20773139538127,18.7620779589741));
#95921=CARTESIAN_POINT('Ctrl Pts',(-1.94282460118863,1.36049291083907,18.7491918731087));
#95922=CARTESIAN_POINT('Ctrl Pts',(-1.93266561689994,1.37488619564203,18.7479772443534));
#95923=CARTESIAN_POINT('Ctrl Pts',(-1.91838940737889,1.3946418162566,18.7463108772995));
#95924=CARTESIAN_POINT('Ctrl Pts',(-1.91440853841083,1.40010130522569,18.7458504588808));
#95925=CARTESIAN_POINT('Ctrl Pts',(-1.90753370488749,1.4094455261716,18.7450626765911));
#95926=CARTESIAN_POINT('Ctrl Pts',(-1.90465109834309,1.41333850198485,18.7447345468374));
#95927=CARTESIAN_POINT('Ctrl Pts',(-1.89860938679805,1.42144581271925,18.7440514048503));
#95928=CARTESIAN_POINT('Ctrl Pts',(-1.8954481478562,1.42565848702899,18.7436965561889));
#95929=CARTESIAN_POINT('Ctrl Pts',(-1.88772550197103,1.43587861131393,18.7428358848511));
#95930=CARTESIAN_POINT('Ctrl Pts',(-1.88314936582983,1.44187496931005,18.7423310842754));
#95931=CARTESIAN_POINT('Ctrl Pts',(-1.86676906325064,1.46312795822798,18.7405421190698));
#95932=CARTESIAN_POINT('Ctrl Pts',(-1.8548070791405,1.47826280349651,18.7392685298721));
#95933=CARTESIAN_POINT('Ctrl Pts',(-1.82475199537688,1.51535057634333,18.7361438005216));
#95934=CARTESIAN_POINT('Ctrl Pts',(-1.8064456849198,1.53712763212333,18.7343056446987));
#95935=CARTESIAN_POINT('Ctrl Pts',(-1.65067474003797,1.71580391305499,18.7191442541905));
#95936=CARTESIAN_POINT('Ctrl Pts',(-1.49344440301926,1.85427954792722,18.7067978965549));
#95937=CARTESIAN_POINT('Ctrl Pts',(-1.2437592428878,2.02156052828421,18.6880401838632));
#95938=CARTESIAN_POINT('Ctrl Pts',(-1.16450860998334,2.06822645262339,18.6822024412626));
#95939=CARTESIAN_POINT('Ctrl Pts',(-1.06711489221767,2.11820040894792,18.6750453824303));
#95940=CARTESIAN_POINT('Ctrl Pts',(-1.05138417137342,2.12605231882062,18.6738900648808));
#95941=CARTESIAN_POINT('Ctrl Pts',(-1.02535002174132,2.13868754009514,18.6719783704234));
#95942=CARTESIAN_POINT('Ctrl Pts',(-1.0150967544948,2.14357309943853,18.6712255580424));
#95943=CARTESIAN_POINT('Ctrl Pts',(-0.996540947123981,2.1522517316632,18.6698631249258));
#95944=CARTESIAN_POINT('Ctrl Pts',(-0.98825080000316,2.15607090050937,18.6692544210438));
#95945=CARTESIAN_POINT('Ctrl Pts',(-0.97046814486707,2.16413904398056,18.6679485996849));
#95946=CARTESIAN_POINT('Ctrl Pts',(-0.960969350282641,2.1683736125749,18.6672510022746));
#95947=CARTESIAN_POINT('Ctrl Pts',(-0.935067165364577,2.17971719827224,
18.6653483420286));
#95948=CARTESIAN_POINT('Ctrl Pts',(-0.918611029799717,2.1867033208726,18.6641391223376));
#95949=CARTESIAN_POINT('Ctrl Pts',(-0.829772870769042,2.22323801136056,
18.6576075080201));
#95950=CARTESIAN_POINT('Ctrl Pts',(-0.756049980422834,2.24937685903972,
18.6521718510515));
#95951=CARTESIAN_POINT('Ctrl Pts',(-0.504848549649827,2.32469640816963,
18.6335892802959));
#95952=CARTESIAN_POINT('Ctrl Pts',(-0.322972581486908,2.3568538006023,18.6199778618305));
#95953=CARTESIAN_POINT('Ctrl Pts',(-0.10956132734833,2.36940466513714,18.6045137407469));
#95954=CARTESIAN_POINT('Ctrl Pts',(-0.0798477853005942,2.37059203524411,
18.6023736754747));
#95955=CARTESIAN_POINT('Ctrl Pts',(0.00190205393253838,2.3723199255449,
18.5965335772806));
#95956=CARTESIAN_POINT('Ctrl Pts',(0.053949897088508,2.37170736490583,18.5928683812466));
#95957=CARTESIAN_POINT('Ctrl Pts',(0.115986763319578,2.36893357367933,18.5885941878057));
#95958=CARTESIAN_POINT('Ctrl Pts',(0.126030993296137,2.36842044483756,18.5879051313908));
#95959=CARTESIAN_POINT('Ctrl Pts',(0.142463822813691,2.36747610623312,18.5867829880303));
#95960=CARTESIAN_POINT('Ctrl Pts',(0.148854351064524,2.36708289652537,18.5863478844971));
#95961=CARTESIAN_POINT('Ctrl Pts',(0.160342521694305,2.36632932030617,18.5855681084475));
#95962=CARTESIAN_POINT('Ctrl Pts',(0.165440634765094,2.36597835457686,18.5852229252734));
#95963=CARTESIAN_POINT('Ctrl Pts',(0.176618234501882,2.36517255741627,18.5844679983444));
#95964=CARTESIAN_POINT('Ctrl Pts',(0.18269710750569,2.36471076373935,18.5840586477392));
#95965=CARTESIAN_POINT('Ctrl Pts',(0.200103776645388,2.3633209088671,18.5828897831624));
#95966=CARTESIAN_POINT('Ctrl Pts',(0.211426968363484,2.36233483860016,18.5821334300941));
#95967=CARTESIAN_POINT('Ctrl Pts',(0.2900251384133,2.35492052133287,18.5769084106021));
#95968=CARTESIAN_POINT('Ctrl Pts',(0.357012785027204,2.34570012523191,18.5725827377564));
#95969=CARTESIAN_POINT('Ctrl Pts',(0.53578938543403,2.31325462333385,18.5611635879967));
#95970=CARTESIAN_POINT('Ctrl Pts',(0.646446452166589,2.28480351850729,18.5542238170749));
#95971=CARTESIAN_POINT('Ctrl Pts',(0.903286424763167,2.19860397318873,18.5376057488124));
#95972=CARTESIAN_POINT('Ctrl Pts',(1.04660607922392,2.13410203459282,18.5278954450568));
#95973=CARTESIAN_POINT('Ctrl Pts',(1.19874285183673,2.04659829603238,18.5164351946238));
#95974=CARTESIAN_POINT('Ctrl Pts',(1.21487033885845,2.03706628188476,18.5152053387258));
#95975=CARTESIAN_POINT('Ctrl Pts',(1.24088980571409,2.02126881070514,18.5131956955289));
#95976=CARTESIAN_POINT('Ctrl Pts',(1.25085148999671,2.01511926612143,18.5124201366882));
#95977=CARTESIAN_POINT('Ctrl Pts',(1.26852755743489,2.00402590907782,18.5110327470355));
#95978=CARTESIAN_POINT('Ctrl Pts',(1.2762596430015,1.99911063421166,18.5104219800391));
#95979=CARTESIAN_POINT('Ctrl Pts',(1.29252471424234,1.98863813149318,18.5091288593763));
#95980=CARTESIAN_POINT('Ctrl Pts',(1.30105075748709,1.98307051709702,18.5084461266104));
#95981=CARTESIAN_POINT('Ctrl Pts',(1.32362166683324,1.96812321239009,18.5066255271191));
#95982=CARTESIAN_POINT('Ctrl Pts',(1.33760243198273,1.95864825944254,18.5054840917558));
#95983=CARTESIAN_POINT('Ctrl Pts',(1.40469829893898,1.91212307094796,18.4999382446258));
#95984=CARTESIAN_POINT('Ctrl Pts',(1.45637741706116,1.87306042551144,18.495457466478));
#95985=CARTESIAN_POINT('Ctrl Pts',(1.6896253317248,1.68126206337177,18.474212476597));
#95986=CARTESIAN_POINT('Ctrl Pts',(1.84917957844107,1.50398767360189,18.4564645970122));
#95987=CARTESIAN_POINT('Ctrl Pts',(2.00454905423034,1.26846572792676,18.4363998746689));
#95988=CARTESIAN_POINT('Ctrl Pts',(2.02825188050805,1.23021021637042,18.4332423289523));
#95989=CARTESIAN_POINT('Ctrl Pts',(2.05615300391422,1.18217773422587,18.4294219550703));
#95990=CARTESIAN_POINT('Ctrl Pts',(2.06139147108046,1.17301943046962,18.4286998462869));
#95991=CARTESIAN_POINT('Ctrl Pts',(2.06950510032962,1.15861232058548,18.4275741088186));
#95992=CARTESIAN_POINT('Ctrl Pts',(2.07242172642968,1.15338721145426,18.4271679222311));
#95993=CARTESIAN_POINT('Ctrl Pts',(2.07779693702528,1.14367135177573,18.4264165873547));
#95994=CARTESIAN_POINT('Ctrl Pts',(2.08026073878041,1.13918371297294,18.4260711192105));
#95995=CARTESIAN_POINT('Ctrl Pts',(2.08584247629389,1.12893848169294,18.4252859429967));
#95996=CARTESIAN_POINT('Ctrl Pts',(2.08895111175834,1.12317593753154,18.4248468271886));
#95997=CARTESIAN_POINT('Ctrl Pts',(2.09843168224074,1.10542608544135,18.4235017395438));
#95998=CARTESIAN_POINT('Ctrl Pts',(2.10472473368632,1.09339662171995,18.4226005855719));
#95999=CARTESIAN_POINT('Ctrl Pts',(2.16852226782995,0.968852595392169,18.4133709330852));
#96000=CARTESIAN_POINT('Ctrl Pts',(2.21705997920133,0.851950012875309,18.4055406039854));
#96001=CARTESIAN_POINT('Ctrl Pts',(2.31718140379656,0.543253732273883,18.3856039291076));
#96002=CARTESIAN_POINT('Ctrl Pts',(2.35444570973427,0.34789444499838,18.3736099783295));
#96003=CARTESIAN_POINT('Ctrl Pts',(2.36873467684687,0.12269059553261,18.3589640701756));
#96004=CARTESIAN_POINT('Ctrl Pts',(2.369999873543,0.0951706222629558,18.3571622495575));
#96005=CARTESIAN_POINT('Ctrl Pts',(2.37113333796937,0.0554401493765309,
18.3545408362035));
#96006=CARTESIAN_POINT('Ctrl Pts',(2.37138715036497,0.0432422278212077,
18.3537332885812));
#96007=CARTESIAN_POINT('Ctrl Pts',(2.37166805975997,0.0217820580899005,
18.3523075073959));
#96008=CARTESIAN_POINT('Ctrl Pts',(2.37173503498008,0.0125205194035137,
18.351690534684));
#96009=CARTESIAN_POINT('Ctrl Pts',(2.37176130605753,-0.00659870758624893,
18.3504133616833));
#96010=CARTESIAN_POINT('Ctrl Pts',(2.37171339413396,-0.0164562099832505,
18.3497529475765));
#96011=CARTESIAN_POINT('Ctrl Pts',(2.37143310872952,-0.0417184759970903,
18.3480553890985));
#96012=CARTESIAN_POINT('Ctrl Pts',(2.37111208597875,-0.0571215946107433,
18.3470154900759));
#96013=CARTESIAN_POINT('Ctrl Pts',(2.36913337438663,-0.121804484884013,
18.3426274909025));
#96014=CARTESIAN_POINT('Ctrl Pts',(2.36608931532903,-0.171026307851277,
18.3392364906479));
#96015=CARTESIAN_POINT('Ctrl Pts',(2.35389718838626,-0.301830408297821,
18.3300797053622));
#96016=CARTESIAN_POINT('Ctrl Pts',(2.34204502355489,-0.383087776122668,
18.3242378358102));
#96017=CARTESIAN_POINT('Ctrl Pts',(2.29645080086922,-0.611865866534978,
18.3073994295363));
#96018=CARTESIAN_POINT('Ctrl Pts',(2.25278015865569,-0.756997764949759,
18.2962254576282));
#96019=CARTESIAN_POINT('Ctrl Pts',(2.17103393654159,-0.957092532381801,
18.2806831696291));
#96020=CARTESIAN_POINT('Ctrl Pts',(2.1440154543891,-1.01617613565392,18.2760803028914));
#96021=CARTESIAN_POINT('Ctrl Pts',(2.10975771976275,-1.08362120020772,18.2708679566668));
#96022=CARTESIAN_POINT('Ctrl Pts',(2.1048476862521,-1.09312797518076,18.2701342590254));
#96023=CARTESIAN_POINT('Ctrl Pts',(2.09680673160502,-1.10844174700714,18.2689544304942));
#96024=CARTESIAN_POINT('Ctrl Pts',(2.09371569281862,-1.11426934649491,18.2685059305135));
#96025=CARTESIAN_POINT('Ctrl Pts',(2.08818062022305,-1.12460037877652,18.2677117951661));
#96026=CARTESIAN_POINT('Ctrl Pts',(2.08574626909357,-1.12910885985711,18.2673655634014));
#96027=CARTESIAN_POINT('Ctrl Pts',(2.08045361637527,-1.1388354617641,18.2666193344661));
#96028=CARTESIAN_POINT('Ctrl Pts',(2.07759028783736,-1.14405072296763,18.2662196623388));
#96029=CARTESIAN_POINT('Ctrl Pts',(2.06953088717731,-1.1586000564742,18.2651057606708));
#96030=CARTESIAN_POINT('Ctrl Pts',(2.06429124999805,-1.16791002641602,18.2643942438386));
#96031=CARTESIAN_POINT('Ctrl Pts',(2.03268795430826,-1.2231866895201,18.2601752815136));
#96032=CARTESIAN_POINT('Ctrl Pts',(2.00485041708913,-1.26829878994666,18.2567551273347));
#96033=CARTESIAN_POINT('Ctrl Pts',(1.90544539733524,-1.41792559909278,18.2453566725837));
#96034=CARTESIAN_POINT('Ctrl Pts',(1.8270274596388,-1.51763330635945,18.2376587423586));
#96035=CARTESIAN_POINT('Ctrl Pts',(1.63224009091363,-1.72819234997147,18.2200698351161));
#96036=CARTESIAN_POINT('Ctrl Pts',(1.51184855445607,-1.83443727092541,18.2101634984347));
#96037=CARTESIAN_POINT('Ctrl Pts',(1.36650586314567,-1.93860989705733,18.1984860934438));
#96038=CARTESIAN_POINT('Ctrl Pts',(1.35120409391995,-1.94930604851172,18.1972603915262));
#96039=CARTESIAN_POINT('Ctrl Pts',(1.3261202848848,-1.96640271907262,18.195256197912));
#96040=CARTESIAN_POINT('Ctrl Pts',(1.31641419575749,-1.97291366270145,18.1944818963411));
#96041=CARTESIAN_POINT('Ctrl Pts',(1.29901603430026,-1.98439897961288,18.1930959068778));
#96042=CARTESIAN_POINT('Ctrl Pts',(1.29134246635504,-1.98940106519379,18.1924852746644));
#96043=CARTESIAN_POINT('Ctrl Pts',(1.27506846347442,-1.99987559335461,18.1911915524305));
#96044=CARTESIAN_POINT('Ctrl Pts',(1.26646135940306,-2.00533727710442,18.1905080781475));
#96045=CARTESIAN_POINT('Ctrl Pts',(1.24345955273348,-2.01972604583219,18.1886833953017));
#96046=CARTESIAN_POINT('Ctrl Pts',(1.2290041969046,-2.02855456359102,18.1875385897122));
#96047=CARTESIAN_POINT('Ctrl Pts',(1.15831671403562,-2.07069361530912,18.1819485304966));
#96048=CARTESIAN_POINT('Ctrl Pts',(1.10082355078082,-2.10182199986388,18.1774254244031));
#96049=CARTESIAN_POINT('Ctrl Pts',(0.822685710882808,-2.23786949286002,
18.1556349719605));
#96050=CARTESIAN_POINT('Ctrl Pts',(0.588035363089336,-2.3106389887493,18.1373162435833));
#96051=CARTESIAN_POINT('Ctrl Pts',(0.308564686573695,-2.35190387428073,
18.1173202162493));
#96052=CARTESIAN_POINT('Ctrl Pts',(0.270555135296414,-2.3565789478467,18.1146430772318));
#96053=CARTESIAN_POINT('Ctrl Pts',(0.22249328839912,-2.36131209826872,18.1113246380363));
#96054=CARTESIAN_POINT('Ctrl Pts',(0.212533795847012,-2.36222934606758,
18.1106405863889));
#96055=CARTESIAN_POINT('Ctrl Pts',(0.196732161749504,-2.36358389592875,
18.1095612999533));
#96056=CARTESIAN_POINT('Ctrl Pts',(0.190893831297306,-2.36406258877249,
18.1091638313948));
#96057=CARTESIAN_POINT('Ctrl Pts',(0.180444484493849,-2.36488038293118,
18.1084548498376));
#96058=CARTESIAN_POINT('Ctrl Pts',(0.175834286165009,-2.36522763004027,
18.1081428932598));
#96059=CARTESIAN_POINT('Ctrl Pts',(0.164783901016678,-2.36602747392307,
18.1073971377854));
#96060=CARTESIAN_POINT('Ctrl Pts',(0.158342854408788,-2.3664672582468,18.1069640609123));
#96061=CARTESIAN_POINT('Ctrl Pts',(0.138815346633409,-2.36772048080911,
18.1056557455279));
#96062=CARTESIAN_POINT('Ctrl Pts',(0.125723587473741,-2.36845172523456,
18.1047849507712));
#96063=CARTESIAN_POINT('Ctrl Pts',(0.0954114528987166,-2.36989276759288,
18.1027820004851));
#96064=CARTESIAN_POINT('Ctrl Pts',(0.0781878569893333,-2.37052352310055,
18.1016537958135));
#96065=CARTESIAN_POINT('Ctrl Pts',(0.0191720720200844,-2.37204083893903,
18.0978172191023));
#96066=CARTESIAN_POINT('Ctrl Pts',(-0.0226379414105889,-2.37201038475446,
18.0951491900336));
#96067=CARTESIAN_POINT('Ctrl Pts',(-0.261989599228159,-2.3655060795045,
18.0800516682263));
#96068=CARTESIAN_POINT('Ctrl Pts',(-0.458111944455925,-2.33546590371927,
18.0683047789183));
#96069=CARTESIAN_POINT('Ctrl Pts',(-0.675253954785322,-2.27376746744674,
18.0541543923723));
#96070=CARTESIAN_POINT('Ctrl Pts',(-0.702123067630764,-2.26561460012877,
18.0523840125398));
#96071=CARTESIAN_POINT('Ctrl Pts',(-0.783901774435791,-2.23920610402609,
18.0469263892053));
#96072=CARTESIAN_POINT('Ctrl Pts',(-0.83828998853264,-2.21941771412418,
18.0431994509407));
#96073=CARTESIAN_POINT('Ctrl Pts',(-0.907584082453756,-2.19129546396012,
18.0382965027672));
#96074=CARTESIAN_POINT('Ctrl Pts',(-0.923202161365873,-2.18476141067499,
18.0371811011504));
#96075=CARTESIAN_POINT('Ctrl Pts',(-0.948108231690302,-2.17402684414751,
18.0353851232423));
#96076=CARTESIAN_POINT('Ctrl Pts',(-0.957441616189827,-2.16993259898191,
18.0347081723703));
#96077=CARTESIAN_POINT('Ctrl Pts',(-0.97488966673664,-2.16214423447773,
18.033435156353));
#96078=CARTESIAN_POINT('Ctrl Pts',(-0.983010480228202,-2.15846425613357,
18.0328395854654));
#96079=CARTESIAN_POINT('Ctrl Pts',(-1.00140600410227,-2.1500029085617,18.0314833819141));
#96080=CARTESIAN_POINT('Ctrl Pts',(-1.01166751802854,-2.14519353837276,
18.0307217924938));
#96081=CARTESIAN_POINT('Ctrl Pts',(-1.04227582173911,-2.13057956678148,
18.0284346657212));
#96082=CARTESIAN_POINT('Ctrl Pts',(-1.06251693991157,-2.12055791471812,
18.0269016278185));
#96083=CARTESIAN_POINT('Ctrl Pts',(-1.10861565377571,-2.09690810564084,
18.0233615794851));
#96084=CARTESIAN_POINT('Ctrl Pts',(-1.13437018156041,-2.08308819571863,
18.0213480693335));
#96085=CARTESIAN_POINT('Ctrl Pts',(-1.22015991875619,-2.03499054916931,
18.014517852893));
#96086=CARTESIAN_POINT('Ctrl Pts',(-1.27894590224819,-1.99856763822727,
18.0096295314601));
#96087=CARTESIAN_POINT('Ctrl Pts',(-1.46611273588913,-1.87095962741856,
17.9933882342957));
#96088=CARTESIAN_POINT('Ctrl Pts',(-1.58701861113946,-1.76956006539772,
17.9817634390738));
#96089=CARTESIAN_POINT('Ctrl Pts',(-1.71401158083338,-1.6394989872607,17.9686229045318));
#96090=CARTESIAN_POINT('Ctrl Pts',(-1.73077686959884,-1.62179040534361,
17.9668677016156));
#96091=CARTESIAN_POINT('Ctrl Pts',(-1.78454590749602,-1.56321245476488,
17.9611786321793));
#96092=CARTESIAN_POINT('Ctrl Pts',(-1.82040153714008,-1.52130754601497,
17.9572892771233));
#96093=CARTESIAN_POINT('Ctrl Pts',(-1.86114012488982,-1.4701904853683,17.9527889696058));
#96094=CARTESIAN_POINT('Ctrl Pts',(-1.86746163794254,-1.46215240930158,
17.9520881949362));
#96095=CARTESIAN_POINT('Ctrl Pts',(-1.87768780031794,-1.44897489227797,
17.9509508809542));
#96096=CARTESIAN_POINT('Ctrl Pts',(-1.88162372574966,-1.44386005939865,
17.9505122348381));
#96097=CARTESIAN_POINT('Ctrl Pts',(-1.88864033420739,-1.43466438320371,
17.9497287165349));
#96098=CARTESIAN_POINT('Ctrl Pts',(-1.89172873236783,-1.43058960194536,
17.9493833109162));
#96099=CARTESIAN_POINT('Ctrl Pts',(-1.89844557917788,-1.42166771892882,
17.9486309320261));
#96100=CARTESIAN_POINT('Ctrl Pts',(-1.90206864829719,-1.41681670634907,
17.948224332804));
#96101=CARTESIAN_POINT('Ctrl Pts',(-1.91232290099519,-1.40297681889011,
17.9470711888568));
#96102=CARTESIAN_POINT('Ctrl Pts',(-1.91890932670062,-1.39395474825456,
17.9463276736002));
#96103=CARTESIAN_POINT('Ctrl Pts',(-1.96213355606657,-1.33385933565691,
17.9414267936992));
#96104=CARTESIAN_POINT('Ctrl Pts',(-1.99679608626379,-1.28138824180711,
17.9373928967893));
#96105=CARTESIAN_POINT('Ctrl Pts',(-2.12094677869681,-1.07615515053145,
17.9222743256585));
#96106=CARTESIAN_POINT('Ctrl Pts',(-2.19532200024861,-0.914928626495204,
17.9116949573022));
#96107=CARTESIAN_POINT('Ctrl Pts',(-2.27011780511127,-0.689508531334165,
17.8969230004817));
#96108=CARTESIAN_POINT('Ctrl Pts',(-2.28696254467658,-0.631394023045678,
17.8931208814061));
#96109=CARTESIAN_POINT('Ctrl Pts',(-2.31307547043486,-0.526451772986574,
17.8862090073252));
#96110=CARTESIAN_POINT('Ctrl Pts',(-2.32318658685537,-0.479867876850167,
17.8831251567669));
#96111=CARTESIAN_POINT('Ctrl Pts',(-2.33476773899723,-0.417500442673414,
17.8789607948591));
#96112=CARTESIAN_POINT('Ctrl Pts',(-2.33749345522159,-0.401959377759127,
17.8779202098518));
#96113=CARTESIAN_POINT('Ctrl Pts',(-2.34168303334647,-0.376586529563042,
17.8762161150517));
#96114=CARTESIAN_POINT('Ctrl Pts',(-2.34324053799955,-0.366770526140564,
17.8755555878879));
#96115=CARTESIAN_POINT('Ctrl Pts',(-2.34605857081241,-0.348259156022767,
17.8743074368661));
#96116=CARTESIAN_POINT('Ctrl Pts',(-2.34733257035951,-0.339565984711979,
17.8737202513871));
#96117=CARTESIAN_POINT('Ctrl Pts',(-2.34980761584553,-0.321997579955538,
17.8725314040962));
#96118=CARTESIAN_POINT('Ctrl Pts',(-2.35100675039044,-0.313122226564666,
17.8719296919819));
#96119=CARTESIAN_POINT('Ctrl Pts',(-2.35364620836122,-0.292715943271395,
17.8705435689204));
#96120=CARTESIAN_POINT('Ctrl Pts',(-2.35505210281333,-0.281180870984554,
17.8697580847151));
#96121=CARTESIAN_POINT('Ctrl Pts',(-2.3600078577577,-0.237872102395406,
17.8668013824221));
#96122=CARTESIAN_POINT('Ctrl Pts',(-2.36299976056252,-0.206039276681309,
17.8646128046373));
#96123=CARTESIAN_POINT('Ctrl Pts',(-2.36965898024622,-0.115595792904657,
17.8583485300874));
#96124=CARTESIAN_POINT('Ctrl Pts',(-2.37179410419742,-0.0569000500529674,
17.8542278766152));
#96125=CARTESIAN_POINT('Ctrl Pts',(-2.37174930964901,0.0018096075435597,
17.8500526884225));
#96126=CARTESIAN_POINT('Ctrl Pts',(-2.37174931191249,0.00180663849497052,
17.8500528995689));
#96127=CARTESIAN_POINT('Ctrl Pts',(-2.37170574199841,0.0590050841321918,
17.8459851842573));
#96128=CARTESIAN_POINT('Ctrl Pts',(-2.36959309700692,0.11613223014051,17.8418717785171));
#96129=CARTESIAN_POINT('Ctrl Pts',(-2.36542646972629,0.173077089235465,
17.8377309811821));
#96130=CARTESIAN_POINT('',(-2.37484677778953,0.00124248804868218,17.651410108095));
#96131=CARTESIAN_POINT('Ctrl Pts',(-2.3692863196969,0.173352773124932,17.639803316701));
#96132=CARTESIAN_POINT('Ctrl Pts',(-2.3733797578211,0.116105017183839,17.6436722471657));
#96133=CARTESIAN_POINT('Ctrl Pts',(-2.37521206853831,0.0586860232060512,
17.6475411776303));
#96134=CARTESIAN_POINT('Ctrl Pts',(-2.37484677778953,0.00124248804868218,
17.651410108095));
#96135=CARTESIAN_POINT('Ctrl Pts',(-2.37174961402095,0.00135310438809495,
17.6531887653657));
#96136=CARTESIAN_POINT('Ctrl Pts',(-2.37183342235333,-0.145547889885166,
17.6625130572248));
#96137=CARTESIAN_POINT('Ctrl Pts',(-2.35826911062213,-0.292155716357493,
17.6713843938006));
#96138=CARTESIAN_POINT('Ctrl Pts',(-2.31386044907917,-0.529285915613408,
17.6862218858644));
#96139=CARTESIAN_POINT('Ctrl Pts',(-2.29098606075038,-0.620865847881408,
17.6920731806637));
#96140=CARTESIAN_POINT('Ctrl Pts',(-2.24645949220594,-0.762602140158466,
17.7015343051946));
#96141=CARTESIAN_POINT('Ctrl Pts',(-2.22842655443409,-0.813791517993269,
17.7050369695526));
#96142=CARTESIAN_POINT('Ctrl Pts',(-2.20279814763335,-0.879281929486418,
17.7096525478088));
#96143=CARTESIAN_POINT('Ctrl Pts',(-2.19678909558774,-0.894189039865554,
17.7107123310204));
#96144=CARTESIAN_POINT('Ctrl Pts',(-2.18675919578312,-0.918359532548057,
17.7124462012953));
#96145=CARTESIAN_POINT('Ctrl Pts',(-2.18282981197231,-0.927660507915268,
17.7131171861059));
#96146=CARTESIAN_POINT('Ctrl Pts',(-2.17514383762062,-0.945534213127708,
17.7144140579433));
#96147=CARTESIAN_POINT('Ctrl Pts',(-2.17139564863548,-0.95411036850187,
17.7150396487939));
#96148=CARTESIAN_POINT('Ctrl Pts',(-2.1626656503379,-0.973767399995322,
17.716481317084));
#96149=CARTESIAN_POINT('Ctrl Pts',(-2.15764929866002,-0.984832553722475,
17.7172985669006));
#96150=CARTESIAN_POINT('Ctrl Pts',(-2.14134410150622,-1.02007623873823,
17.7199202396106));
#96151=CARTESIAN_POINT('Ctrl Pts',(-2.12973248433963,-1.04410226392291,
17.7217357324254));
#96152=CARTESIAN_POINT('Ctrl Pts',(-2.02478481810144,-1.25221547680833,
17.737716554569));
#96153=CARTESIAN_POINT('Ctrl Pts',(-1.90821002238374,-1.42355035905783,
17.752751389025));
#96154=CARTESIAN_POINT('Ctrl Pts',(-1.71500453586684,-1.64043884609838,
17.7739469859592));
#96155=CARTESIAN_POINT('Ctrl Pts',(-1.65571874767782,-1.7002580823744,17.7800605222474));
#96156=CARTESIAN_POINT('Ctrl Pts',(-1.57311335202293,-1.77517905088021,
17.7879658319816));
#96157=CARTESIAN_POINT('Ctrl Pts',(-1.55253462797485,-1.79320457638353,
17.7898885203851));
#96158=CARTESIAN_POINT('Ctrl Pts',(-1.52182776696813,-1.81917666201578,
17.7926843028116));
#96159=CARTESIAN_POINT('Ctrl Pts',(-1.5119401572364,-1.82740265360929,17.7935737000445));
#96160=CARTESIAN_POINT('Ctrl Pts',(-1.49409517025223,-1.84200478761569,
17.7951588209297));
#96161=CARTESIAN_POINT('Ctrl Pts',(-1.48616274465999,-1.84841075555056,
17.7958564562207));
#96162=CARTESIAN_POINT('Ctrl Pts',(-1.47355541088184,-1.85845839926883,
17.7969539275869));
#96163=CARTESIAN_POINT('Ctrl Pts',(-1.46890785781613,-1.86213395811339,
17.7973560951031));
#96164=CARTESIAN_POINT('Ctrl Pts',(-1.46041023718247,-1.86880276720142,
17.7980869777507));
#96165=CARTESIAN_POINT('Ctrl Pts',(-1.45656473732404,-1.87180154137763,
17.7984160763638));
#96166=CARTESIAN_POINT('Ctrl Pts',(-1.44756073402735,-1.87877843748111,
17.7991828157463));
#96167=CARTESIAN_POINT('Ctrl Pts',(-1.44239507312713,-1.88274718202666,
17.7996197938765));
#96168=CARTESIAN_POINT('Ctrl Pts',(-1.42710211263575,-1.89439678432292,
17.8009051399312));
#96169=CARTESIAN_POINT('Ctrl Pts',(-1.41692914736248,-1.90201772480529,
17.8017494483677));
#96170=CARTESIAN_POINT('Ctrl Pts',(-1.31133273741533,-1.97980643553498,
17.8104092834261));
#96171=CARTESIAN_POINT('Ctrl Pts',(-1.21082709036922,-2.04282478133419,
17.817784221682));
#96172=CARTESIAN_POINT('Ctrl Pts',(-0.990213872334371,-2.15912303980801,
17.8331348945922));
#96173=CARTESIAN_POINT('Ctrl Pts',(-0.869556635652998,-2.21047645715894,
17.8410727381015));
#96174=CARTESIAN_POINT('Ctrl Pts',(-0.688828352355133,-2.27029722165716,
17.8529710236549));
#96175=CARTESIAN_POINT('Ctrl Pts',(-0.631697722750983,-2.28685180244383,
17.8567310193342));
#96176=CARTESIAN_POINT('Ctrl Pts',(-0.535842053508748,-2.31076148908148,
17.8630848959532));
#96177=CARTESIAN_POINT('Ctrl Pts',(-0.497446678921503,-2.31933004895306,
17.8656415833285));
#96178=CARTESIAN_POINT('Ctrl Pts',(-0.444826341892124,-2.32970644577635,
17.8691693663205));
#96179=CARTESIAN_POINT('Ctrl Pts',(-0.430770484689626,-2.33234632342885,
17.870113987718));
#96180=CARTESIAN_POINT('Ctrl Pts',(-0.407125635392751,-2.33656611439937,
17.8717072468124));
#96181=CARTESIAN_POINT('Ctrl Pts',(-0.397549126562619,-2.33821452760694,
17.8723536951134));
#96182=CARTESIAN_POINT('Ctrl Pts',(-0.378634806219472,-2.34135071085036,
17.8736328779299));
#96183=CARTESIAN_POINT('Ctrl Pts',(-0.36929768672698,-2.34284158273207,
17.8742655010687));
#96184=CARTESIAN_POINT('Ctrl Pts',(-0.348722073387177,-2.34600086592043,
17.8756622136121));
#96185=CARTESIAN_POINT('Ctrl Pts',(-0.337480057864742,-2.34764442581958,
17.8764270744855));
#96186=CARTESIAN_POINT('Ctrl Pts',(-0.297922266824205,-2.35313768899784,
17.8791247702891));
#96187=CARTESIAN_POINT('Ctrl Pts',(-0.269550109399032,-2.35655623195983,
17.8810710926302));
#96188=CARTESIAN_POINT('Ctrl Pts',(-0.0545725752773576,-2.3785257721283,
17.8959111435252));
#96189=CARTESIAN_POINT('Ctrl Pts',(0.133546535276466,-2.37539491084169,
17.909502949411));
#96190=CARTESIAN_POINT('Ctrl Pts',(0.453012312828874,-2.33199260329422,
17.9330514893249));
#96191=CARTESIAN_POINT('Ctrl Pts',(0.584955895348675,-2.30244322824763,
17.942894599277));
#96192=CARTESIAN_POINT('Ctrl Pts',(0.726757912645861,-2.25769993668585,
17.9531668044338));
#96193=CARTESIAN_POINT('Ctrl Pts',(0.739798290669297,-2.25346057860115,
17.9541083687691));
#96194=CARTESIAN_POINT('Ctrl Pts',(0.759088341637895,-2.24700398390668,
17.9554958426281));
#96195=CARTESIAN_POINT('Ctrl Pts',(0.765366376667241,-2.24487334303957,
17.9559465582791));
#96196=CARTESIAN_POINT('Ctrl Pts',(0.776545830315653,-2.24102690783438,
17.9567475484446));
#96197=CARTESIAN_POINT('Ctrl Pts',(0.781450617482266,-2.2393213173797,17.9570984077864));
#96198=CARTESIAN_POINT('Ctrl Pts',(0.792091450459432,-2.23558185558142,
17.9578583572558));
#96199=CARTESIAN_POINT('Ctrl Pts',(0.797825277406989,-2.23354201387355,
17.958267089846));
#96200=CARTESIAN_POINT('Ctrl Pts',(0.813686405496006,-2.2278304551381,17.9593957808565));
#96201=CARTESIAN_POINT('Ctrl Pts',(0.823796798630394,-2.22411172131955,
17.9601130244233));
#96202=CARTESIAN_POINT('Ctrl Pts',(0.877569478030481,-2.2039164467956,17.9639176446507));
#96203=CARTESIAN_POINT('Ctrl Pts',(0.920767056987352,-2.18622154216185,
17.9669385185713));
#96204=CARTESIAN_POINT('Ctrl Pts',(0.993242380450834,-2.1540039284578,17.9719917511904));
#96205=CARTESIAN_POINT('Ctrl Pts',(1.02279138673865,-2.14013113918767,17.9740476138423));
#96206=CARTESIAN_POINT('Ctrl Pts',(1.21873514837492,-2.04315300665441,17.9877106671746));
#96207=CARTESIAN_POINT('Ctrl Pts',(1.37514242682399,-1.94133397296124,17.9988185881367));
#96208=CARTESIAN_POINT('Ctrl Pts',(1.57848757018939,-1.77193741762053,18.0154474016746));
#96209=CARTESIAN_POINT('Ctrl Pts',(1.63637537325596,-1.71862119660974,18.0204738842507));
#96210=CARTESIAN_POINT('Ctrl Pts',(1.7041748967107,-1.64964018653987,18.0268075306637));
#96211=CARTESIAN_POINT('Ctrl Pts',(1.71669795448427,-1.63660408366716,18.0279974211188));
#96212=CARTESIAN_POINT('Ctrl Pts',(1.7362829143761,-1.6157446370699,18.0298911303832));
#96213=CARTESIAN_POINT('Ctrl Pts',(1.74344395930143,-1.60801500168566,18.0305906771843));
#96214=CARTESIAN_POINT('Ctrl Pts',(1.75680237689437,-1.5934017878899,18.0319092808099));
#96215=CARTESIAN_POINT('Ctrl Pts',(1.76301141502651,-1.58652910323158,18.0325278258428));
#96216=CARTESIAN_POINT('Ctrl Pts',(1.77686932545066,-1.57100819779399,18.0339212462599));
#96217=CARTESIAN_POINT('Ctrl Pts',(1.78449558105185,-1.56234019031363,18.0346970477239));
#96218=CARTESIAN_POINT('Ctrl Pts',(1.80379306368695,-1.5400810291993,18.0366834445101));
#96219=CARTESIAN_POINT('Ctrl Pts',(1.8153739681301,-1.52641289242954,18.0378977143016));
#96220=CARTESIAN_POINT('Ctrl Pts',(1.88821500934869,-1.43844212742857,18.0456800255062));
#96221=CARTESIAN_POINT('Ctrl Pts',(1.94504864105884,-1.36060759097457,18.0524232046689));
#96222=CARTESIAN_POINT('Ctrl Pts',(2.09580226144295,-1.12532579230039,18.0724041803507));
#96223=CARTESIAN_POINT('Ctrl Pts',(2.17640908872627,-0.96019800683005,18.0859923138909));
#96224=CARTESIAN_POINT('Ctrl Pts',(2.25738846686118,-0.730128915946238,
18.1034869742571));
#96225=CARTESIAN_POINT('Ctrl Pts',(2.27535609696793,-0.672046894754203,
18.107783472737));
#96226=CARTESIAN_POINT('Ctrl Pts',(2.29396679330645,-0.602527630298205,
18.1127369032897));
#96227=CARTESIAN_POINT('Ctrl Pts',(2.29678313412631,-0.591701310891322,
18.1135029400769));
#96228=CARTESIAN_POINT('Ctrl Pts',(2.30101931839607,-0.574930862057385,
18.1146808560458));
#96229=CARTESIAN_POINT('Ctrl Pts',(2.30249291764024,-0.569000673234998,
18.1150957007588));
#96230=CARTESIAN_POINT('Ctrl Pts',(2.3051758452213,-0.558022693155453,18.1158604789062));
#96231=CARTESIAN_POINT('Ctrl Pts',(2.3063915151016,-0.55297665725261,18.1162107595499));
#96232=CARTESIAN_POINT('Ctrl Pts',(2.3091145663072,-0.541508536305284,18.1170040379381));
#96233=CARTESIAN_POINT('Ctrl Pts',(2.31061172583991,-0.535084133850368,
18.1174464472306));
#96234=CARTESIAN_POINT('Ctrl Pts',(2.31443114413587,-0.51837979138383,18.1185918281201));
#96235=CARTESIAN_POINT('Ctrl Pts',(2.31671175428307,-0.508090333339361,
18.1192925000824));
#96236=CARTESIAN_POINT('Ctrl Pts',(2.33141200714864,-0.439609539128274,
18.1239256512753));
#96237=CARTESIAN_POINT('Ctrl Pts',(2.3417078219471,-0.380978148627399,18.127748309186));
#96238=CARTESIAN_POINT('Ctrl Pts',(2.37718430487489,-0.122102242138023,
18.1442433433969));
#96239=CARTESIAN_POINT('Ctrl Pts',(2.37895888052462,0.0804969451879324,
18.1562237784904));
#96240=CARTESIAN_POINT('Ctrl Pts',(2.34545712120427,0.361388724791912,18.1739767144192));
#96241=CARTESIAN_POINT('Ctrl Pts',(2.33173527595175,0.441338086820873,18.1791524934653));
#96242=CARTESIAN_POINT('Ctrl Pts',(2.3099482170731,0.538209718041095,18.185653306329));
#96243=CARTESIAN_POINT('Ctrl Pts',(2.30574279252618,0.55595018668948,18.1868532772087));
#96244=CARTESIAN_POINT('Ctrl Pts',(2.29877662231556,0.583897121489828,18.1887593710122));
#96245=CARTESIAN_POINT('Ctrl Pts',(2.29615138086196,0.59413688472647,18.1894611248946));
#96246=CARTESIAN_POINT('Ctrl Pts',(2.29109868314232,0.613311177485965,18.1907816525605));
#96247=CARTESIAN_POINT('Ctrl Pts',(2.28868718634904,0.622249736982913,18.1913998989234));
#96248=CARTESIAN_POINT('Ctrl Pts',(2.2831640110465,0.642255656224311,18.1927896949178));
#96249=CARTESIAN_POINT('Ctrl Pts',(2.28002409030713,0.653314907845404,18.1935621498184));
#96250=CARTESIAN_POINT('Ctrl Pts',(2.27183076997444,0.681394329195688,18.1955342706714));
#96251=CARTESIAN_POINT('Ctrl Pts',(2.26666650422937,0.698381133708327,18.1967375212846));
#96252=CARTESIAN_POINT('Ctrl Pts',(2.23344621786385,0.803400846316708,18.2042415325558));
#96253=CARTESIAN_POINT('Ctrl Pts',(2.20046018506622,0.889778600285362,18.210702981233));
#96254=CARTESIAN_POINT('Ctrl Pts',(2.08577219872466,1.14441384949323,18.2306388479346));
#96255=CARTESIAN_POINT('Ctrl Pts',(1.9891560321356,1.30513486989951,18.2445087855476));
#96256=CARTESIAN_POINT('Ctrl Pts',(1.83718610426479,1.50123049585591,18.2623076229358));
#96257=CARTESIAN_POINT('Ctrl Pts',(1.79782259572171,1.54815412636854,18.2666368495276));
#96258=CARTESIAN_POINT('Ctrl Pts',(1.74915373381788,1.60180675396093,18.2716228436165));
#96259=CARTESIAN_POINT('Ctrl Pts',(1.74156509915752,1.61005424737185,18.2723903291557));
#96260=CARTESIAN_POINT('Ctrl Pts',(1.72974589162321,1.62271827654194,18.2735699903415));
#96261=CARTESIAN_POINT('Ctrl Pts',(1.72555634870324,1.62717262274551,18.273985145115));
#96262=CARTESIAN_POINT('Ctrl Pts',(1.71777914061087,1.63537757820224,18.2747502076607));
#96263=CARTESIAN_POINT('Ctrl Pts',(1.71419641297866,1.63913259313402,18.275100464768));
#96264=CARTESIAN_POINT('Ctrl Pts',(1.70603613173496,1.64762927093074,18.275893326752));
#96265=CARTESIAN_POINT('Ctrl Pts',(1.7014511267994,1.65236362916364,18.2763353457791));
#96266=CARTESIAN_POINT('Ctrl Pts',(1.68949688152212,1.66460475899594,18.2774790410602));
#96267=CARTESIAN_POINT('Ctrl Pts',(1.68209723057876,1.67208182615978,18.2781784288283));
#96268=CARTESIAN_POINT('Ctrl Pts',(1.63280231121122,1.72123405153977,18.2827834234678));
#96269=CARTESIAN_POINT('Ctrl Pts',(1.58940780397776,1.76138418128598,18.2865807272622));
#96270=CARTESIAN_POINT('Ctrl Pts',(1.37892531860329,1.94200879360372,18.3040945560035));
#96271=CARTESIAN_POINT('Ctrl Pts',(1.19446733944039,2.06060523899123,18.3169967842246));
#96272=CARTESIAN_POINT('Ctrl Pts',(0.935589584378949,2.18044893106411,18.3350299043153));
#96273=CARTESIAN_POINT('Ctrl Pts',(0.873639993177372,2.20600028468821,18.3393309334958));
#96274=CARTESIAN_POINT('Ctrl Pts',(0.794507405411819,2.23478249496345,18.3448500248827));
#96275=CARTESIAN_POINT('Ctrl Pts',(0.778255130046074,2.2404940846964,18.3459847576857));
#96276=CARTESIAN_POINT('Ctrl Pts',(0.752140550800908,2.24935319325938,18.3478106821816));
#96277=CARTESIAN_POINT('Ctrl Pts',(0.74231714598531,2.25261413588092,18.3484981163552));
#96278=CARTESIAN_POINT('Ctrl Pts',(0.723635465395617,2.25868016974658,18.3498066991493));
#96279=CARTESIAN_POINT('Ctrl Pts',(0.714781412862605,2.26149771690584,18.3504274238967));
#96280=CARTESIAN_POINT('Ctrl Pts',(0.694603452924602,2.26778843750314,18.3518433447345));
#96281=CARTESIAN_POINT('Ctrl Pts',(0.683269698463124,2.27122893262466,18.3526395940912));
#96282=CARTESIAN_POINT('Ctrl Pts',(0.653783155120678,2.27993923954168,18.3547138306048));
#96283=CARTESIAN_POINT('Ctrl Pts',(0.635592591604018,2.28507710401309,18.3559960669848));
#96284=CARTESIAN_POINT('Ctrl Pts',(0.466303628291112,2.33071444078106,18.3679558813846));
#96285=CARTESIAN_POINT('Ctrl Pts',(0.311636353017043,2.35638157498201,18.3791191057528));
#96286=CARTESIAN_POINT('Ctrl Pts',(0.0439197365305154,2.37398294364994,
18.3986488458375));
#96287=CARTESIAN_POINT('Ctrl Pts',(-0.0681387684765478,2.37341142431974,
18.4068734872944));
#96288=CARTESIAN_POINT('Ctrl Pts',(-0.248866658219189,2.35967574986997,
18.4199261233835));
#96289=CARTESIAN_POINT('Ctrl Pts',(-0.317738240700849,2.3513929360394,18.4248473851097));
#96290=CARTESIAN_POINT('Ctrl Pts',(-0.397548285450235,2.33822299465723,
18.4304180412203));
#96291=CARTESIAN_POINT('Ctrl Pts',(-0.408928318019502,2.33625962949064,
18.4312091689987));
#96292=CARTESIAN_POINT('Ctrl Pts',(-0.426383580456419,2.33311666918466,
18.4324172759056));
#96293=CARTESIAN_POINT('Ctrl Pts',(-0.432469091013121,2.33199632016331,
18.4328374597782));
#96294=CARTESIAN_POINT('Ctrl Pts',(-0.443645570105871,2.32989346368997,
18.4336072243406));
#96295=CARTESIAN_POINT('Ctrl Pts',(-0.448737685132687,2.32891808250796,
18.4339571886052));
#96296=CARTESIAN_POINT('Ctrl Pts',(-0.460205870615151,2.32668237179374,
18.4347436968437));
#96297=CARTESIAN_POINT('Ctrl Pts',(-0.466579974275102,2.32541252957876,
18.4351796952322));
#96298=CARTESIAN_POINT('Ctrl Pts',(-0.482961898297004,2.3220788702843,18.436297475918));
#96299=CARTESIAN_POINT('Ctrl Pts',(-0.492961874081811,2.31997652467836,
18.4369771379888));
#96300=CARTESIAN_POINT('Ctrl Pts',(-0.555002103406856,2.30651423666919,
18.4411790069551));
#96301=CARTESIAN_POINT('Ctrl Pts',(-0.606665530876341,2.29346750884674,
18.4446134298115));
#96302=CARTESIAN_POINT('Ctrl Pts',(-0.673734309713538,2.2741049839767,18.449039157693));
#96303=CARTESIAN_POINT('Ctrl Pts',(-0.689570415980987,2.26935322526014,
18.450081707307));
#96304=CARTESIAN_POINT('Ctrl Pts',(-0.726049490018855,2.25799025185859,
18.4524802958612));
#96305=CARTESIAN_POINT('Ctrl Pts',(-0.74665422786761,2.25126083367592,18.453832899681));
#96306=CARTESIAN_POINT('Ctrl Pts',(-0.890536266017226,2.20207684674148,
18.4632805222851));
#96307=CARTESIAN_POINT('Ctrl Pts',(-1.01022240249457,2.14980222806255,18.471164457647));
#96308=CARTESIAN_POINT('Ctrl Pts',(-1.22879475123163,2.03203355707197,18.4865210031303));
#96309=CARTESIAN_POINT('Ctrl Pts',(-1.32825390427852,1.96845950007973,18.4939385685271));
#96310=CARTESIAN_POINT('Ctrl Pts',(-1.43853270528544,1.88579421903294,18.5029459785705));
#96311=CARTESIAN_POINT('Ctrl Pts',(-1.45434599510926,1.87362586101682,18.5042574889887));
#96312=CARTESIAN_POINT('Ctrl Pts',(-1.47859079955985,1.85447756786646,18.5063004259626));
#96313=CARTESIAN_POINT('Ctrl Pts',(-1.48713094802665,1.84763614893775,18.5070263467968));
#96314=CARTESIAN_POINT('Ctrl Pts',(-1.502082979576,1.83548741739263,18.5083086069133));
#96315=CARTESIAN_POINT('Ctrl Pts',(-1.50851488652366,1.83020495328633,18.508863937658));
#96316=CARTESIAN_POINT('Ctrl Pts',(-1.5231375929359,1.81806601494296,18.5101351258628));
#96317=CARTESIAN_POINT('Ctrl Pts',(-1.53131009555283,1.81118788271092,18.5108518592384));
#96318=CARTESIAN_POINT('Ctrl Pts',(-1.55332166559151,1.79240705627806,18.5127995725726));
#96319=CARTESIAN_POINT('Ctrl Pts',(-1.56707000074492,1.78039962716612,18.51403485321));
#96320=CARTESIAN_POINT('Ctrl Pts',(-1.6353543599066,1.71935820017017,18.5202665286874));
#96321=CARTESIAN_POINT('Ctrl Pts',(-1.6877285317892,1.66797688374222,18.525361263538));
#96322=CARTESIAN_POINT('Ctrl Pts',(-1.87786521957995,1.46330808262911,18.5451209721441));
#96323=CARTESIAN_POINT('Ctrl Pts',(-1.99782268371322,1.29473299503854,18.5604322621519));
#96324=CARTESIAN_POINT('Ctrl Pts',(-2.12415473253877,1.05696110572707,18.5797685628429));
#96325=CARTESIAN_POINT('Ctrl Pts',(-2.15159328520423,0.999924035898249,
18.5842466214546));
#96326=CARTESIAN_POINT('Ctrl Pts',(-2.1812075073074,0.931482444221716,18.5893803660805));
#96327=CARTESIAN_POINT('Ctrl Pts',(-2.18562050561715,0.921080209359811,
18.5901542416944));
#96328=CARTESIAN_POINT('Ctrl Pts',(-2.1923145389544,0.904982131750435,18.5913415977056));
#96329=CARTESIAN_POINT('Ctrl Pts',(-2.19464802215909,0.899308488508613,
18.5917581175134));
#96330=CARTESIAN_POINT('Ctrl Pts',(-2.19891436730815,0.88881977189486,18.5925244399729));
#96331=CARTESIAN_POINT('Ctrl Pts',(-2.20085343388057,0.884007435045523,
18.592874601297));
#96332=CARTESIAN_POINT('Ctrl Pts',(-2.20521029979314,0.873091457819205,
18.5936656653581));
#96333=CARTESIAN_POINT('Ctrl Pts',(-2.20761855625226,0.866984124853753,
18.5941059935295));
#96334=CARTESIAN_POINT('Ctrl Pts',(-2.21378881175248,0.851143957703621,
18.5952423940668));
#96335=CARTESIAN_POINT('Ctrl Pts',(-2.21751204585688,0.841396028139503,
18.5959362259058));
#96336=CARTESIAN_POINT('Ctrl Pts',(-2.24128487900333,0.777901528986282,
18.600421923511));
#96337=CARTESIAN_POINT('Ctrl Pts',(-2.25944515932818,0.723462175274785,
18.6041117966285));
#96338=CARTESIAN_POINT('Ctrl Pts',(-2.2795056542623,0.655166123527973,18.6086117407948));
#96339=CARTESIAN_POINT('Ctrl Pts',(-2.28328091117517,0.641885480345634,
18.6094808178627));
#96340=CARTESIAN_POINT('Ctrl Pts',(-2.32790527061401,0.479528318939938,
18.6200410194997));
#96341=CARTESIAN_POINT('Ctrl Pts',(-2.35416628279363,0.3269692411613,18.6293285405642));
#96342=CARTESIAN_POINT('Ctrl Pts',(-2.36542649880509,0.173076691818106,
18.6388842277111));
#96343=CARTESIAN_POINT('Origin',(0.,0.,-1.84858989190503));
#96344=CARTESIAN_POINT('',(-2.36542647001695,0.17307708526301,19.8356128877059));
#96345=CARTESIAN_POINT('',(-2.36542650053005,0.173076668243166,19.6378399312857));
#96346=CARTESIAN_POINT('',(-2.36542649454111,0.173076750093529,-1.84858989190503));
#96347=CARTESIAN_POINT('Ctrl Pts',(-2.3654264700169,0.173077085263749,19.8356128877059));
#96348=CARTESIAN_POINT('Ctrl Pts',(-2.35323422706518,0.33970719786897,19.8252325324572));
#96349=CARTESIAN_POINT('Ctrl Pts',(-2.323456168924,0.504766661904006,19.815190742496));
#96350=CARTESIAN_POINT('Ctrl Pts',(-2.26083942397636,0.718962231332386,
19.8012072448235));
#96351=CARTESIAN_POINT('Ctrl Pts',(-2.24332976957548,0.771862980924048,
19.7976761047838));
#96352=CARTESIAN_POINT('Ctrl Pts',(-2.21098346100693,0.859155500580385,
19.7916802044054));
#96353=CARTESIAN_POINT('Ctrl Pts',(-2.19716537539688,0.893901616588215,
19.78924755419));
#96354=CARTESIAN_POINT('Ctrl Pts',(-2.17708906651077,0.941102902069325,
19.7858722520732));
#96355=CARTESIAN_POINT('Ctrl Pts',(-2.17153337343339,0.953852331342261,
19.7849533765998));
#96356=CARTESIAN_POINT('Ctrl Pts',(-2.16197831514997,0.975263467969434,
19.7833977367547));
#96357=CARTESIAN_POINT('Ctrl Pts',(-2.15803818302342,0.983951352043978,
19.7827630115038));
#96358=CARTESIAN_POINT('Ctrl Pts',(-2.15013218985068,1.00110792256907,19.7815025070584));
#96359=CARTESIAN_POINT('Ctrl Pts',(-2.1461684422494,1.00957739654596,19.7808768098936));
#96360=CARTESIAN_POINT('Ctrl Pts',(-2.13638790779684,1.03015789058932,19.7793478669117));
#96361=CARTESIAN_POINT('Ctrl Pts',(-2.13051815385665,1.04224323228562,19.7784427942912));
#96362=CARTESIAN_POINT('Ctrl Pts',(-2.11042269333423,1.08273894564482,19.7753851844087));
#96363=CARTESIAN_POINT('Ctrl Pts',(-2.09572939555262,1.1109121020342,19.7732163972922));
#96364=CARTESIAN_POINT('Ctrl Pts',(-1.98336292460144,1.31619807793784,19.757096227552));
#96365=CARTESIAN_POINT('Ctrl Pts',(-1.86397128286467,1.48043384994926,19.7423295411214));
#96366=CARTESIAN_POINT('Ctrl Pts',(-1.71097780090446,1.64261525099771,19.7260650070205));
#96367=CARTESIAN_POINT('Ctrl Pts',(-1.69651988910732,1.65754341741345,19.7245510264689));
#96368=CARTESIAN_POINT('Ctrl Pts',(-1.63506840018614,1.71934722836924,19.7182165956811));
#96369=CARTESIAN_POINT('Ctrl Pts',(-1.58631056620238,1.76443294678743,19.7134311699763));
#96370=CARTESIAN_POINT('Ctrl Pts',(-1.51782271026867,1.82262557554497,19.7070879531499));
#96371=CARTESIAN_POINT('Ctrl Pts',(-1.49969739047633,1.83756839330913,19.7054430630328));
#96372=CARTESIAN_POINT('Ctrl Pts',(-1.4723661563832,1.8594268915841,19.7030161586475));
#96373=CARTESIAN_POINT('Ctrl Pts',(-1.46332759545993,1.86654837193496,19.7022220745988));
#96374=CARTESIAN_POINT('Ctrl Pts',(-1.44693101487991,1.87927492481491,19.7007973363327));
#96375=CARTESIAN_POINT('Ctrl Pts',(-1.43959141859806,1.88490322284688,19.7001652028588));
#96376=CARTESIAN_POINT('Ctrl Pts',(-1.42769341910421,1.89391705161524,19.6991497543746));
#96377=CARTESIAN_POINT('Ctrl Pts',(-1.42315554701653,1.89732933042263,19.6987646224744));
#96378=CARTESIAN_POINT('Ctrl Pts',(-1.41462592675644,1.90369540827246,19.698044811519));
#96379=CARTESIAN_POINT('Ctrl Pts',(-1.41063720057052,1.90665293355087,19.6977098826646));
#96380=CARTESIAN_POINT('Ctrl Pts',(-1.40130213395993,1.91352928646954,19.6969298878984));
#96381=CARTESIAN_POINT('Ctrl Pts',(-1.39594862480298,1.9174382494427,19.6964855065237));
#96382=CARTESIAN_POINT('Ctrl Pts',(-1.38162925115415,1.92780204449874,19.6953044800833));
#96383=CARTESIAN_POINT('Ctrl Pts',(-1.37263442467525,1.93421685917467,19.6945704895389));
#96384=CARTESIAN_POINT('Ctrl Pts',(-1.30177863356973,1.98400566207694,19.6888471842528));
#96385=CARTESIAN_POINT('Ctrl Pts',(-1.23791484721852,2.02446919527554,19.6840362285206));
#96386=CARTESIAN_POINT('Ctrl Pts',(-1.00899498516731,2.15461872577638,19.6675691896541));
#96387=CARTESIAN_POINT('Ctrl Pts',(-0.83532658605038,2.22770900132511,19.6563638300093));
#96388=CARTESIAN_POINT('Ctrl Pts',(-0.579110865355982,2.30131233274503,
19.6396149862796));
#96389=CARTESIAN_POINT('Ctrl Pts',(-0.502341968516801,2.31927970216971,
19.6345791240251));
#96390=CARTESIAN_POINT('Ctrl Pts',(-0.40719884366394,2.33660185294187,19.6282456666917));
#96391=CARTESIAN_POINT('Ctrl Pts',(-0.389535231438675,2.33961137619871,
19.6270661088356));
#96392=CARTESIAN_POINT('Ctrl Pts',(-0.361559503302609,2.34405228860277,
19.6251912892799));
#96393=CARTESIAN_POINT('Ctrl Pts',(-0.351268907604851,2.34561645517582,
19.6245002442858));
#96394=CARTESIAN_POINT('Ctrl Pts',(-0.331936701295934,2.34842487286597,
19.6231992329643));
#96395=CARTESIAN_POINT('Ctrl Pts',(-0.322897528017077,2.34968477450544,
19.6225897746515));
#96396=CARTESIAN_POINT('Ctrl Pts',(-0.302606160096279,2.35239373489734,
19.6212189773812));
#96397=CARTESIAN_POINT('Ctrl Pts',(-0.291350450806926,2.35381428306019,
19.6204567520999));
#96398=CARTESIAN_POINT('Ctrl Pts',(-0.262668181947738,2.35722530314698,
19.6185095399311));
#96399=CARTESIAN_POINT('Ctrl Pts',(-0.245229194411968,2.35910328661205,
19.6173210442405));
#96400=CARTESIAN_POINT('Ctrl Pts',(-0.137358437550926,2.36951077568546,
19.609939787628));
#96401=CARTESIAN_POINT('Ctrl Pts',(-0.0465307437459041,2.3730317704547,
19.6035916103679));
#96402=CARTESIAN_POINT('Ctrl Pts',(0.251430474564564,2.36746975878224,19.5823334496865));
#96403=CARTESIAN_POINT('Ctrl Pts',(0.457169261931409,2.33647476600093,19.5668819448654));
#96404=CARTESIAN_POINT('Ctrl Pts',(0.699444633034538,2.26671469785821,19.5489626290743));
#96405=CARTESIAN_POINT('Ctrl Pts',(0.742278385510339,2.25305165749233,19.5458102274945));
#96406=CARTESIAN_POINT('Ctrl Pts',(0.794313791440348,2.23480814019125,19.5420209193307));
#96407=CARTESIAN_POINT('Ctrl Pts',(0.803904809947787,2.23137600793186,19.5413241943613));
#96408=CARTESIAN_POINT('Ctrl Pts',(0.818960282448285,2.2258787556836,19.5402335360746));
#96409=CARTESIAN_POINT('Ctrl Pts',(0.824439586028089,2.22385510996247,19.5398372341574));
#96410=CARTESIAN_POINT('Ctrl Pts',(0.83472823035326,2.22001200056672,19.5390943538715));
#96411=CARTESIAN_POINT('Ctrl Pts',(0.839539078235053,2.21819715939314,19.5387475241839));
#96412=CARTESIAN_POINT('Ctrl Pts',(0.850562871952614,2.21399754938837,19.5379539554359));
#96413=CARTESIAN_POINT('Ctrl Pts',(0.856771713545251,2.21160226565256,19.5375078501455));
#96414=CARTESIAN_POINT('Ctrl Pts',(0.873344260857463,2.20512854519738,19.5363191770899));
#96415=CARTESIAN_POINT('Ctrl Pts',(0.883689614038453,2.20100312967401,19.535579318406));
#96416=CARTESIAN_POINT('Ctrl Pts',(0.966042088881135,2.16748918948094,19.5297041745093));
#96417=CARTESIAN_POINT('Ctrl Pts',(1.03660154027528,2.13464441296786,19.5247579032972));
#96418=CARTESIAN_POINT('Ctrl Pts',(1.26976673603639,2.0118134185979,19.5082970901789));
#96419=CARTESIAN_POINT('Ctrl Pts',(1.42336782128133,1.906234338101,19.4972034770522));
#96420=CARTESIAN_POINT('Ctrl Pts',(1.62209518680712,1.73209763430365,19.480599576103));
#96421=CARTESIAN_POINT('Ctrl Pts',(1.67850192112975,1.67749345068799,19.4755845088593));
#96422=CARTESIAN_POINT('Ctrl Pts',(1.74432053590521,1.60712918115199,19.4692743279309));
#96423=CARTESIAN_POINT('Ctrl Pts',(1.75639725739358,1.59392188702392,19.468096184289));
#96424=CARTESIAN_POINT('Ctrl Pts',(1.77525655535978,1.57282245330248,19.4662231021776));
#96425=CARTESIAN_POINT('Ctrl Pts',(1.78213880719684,1.5650199912335,19.4655323669739));
#96426=CARTESIAN_POINT('Ctrl Pts',(1.79496182886096,1.55028816677097,19.4642316262527));
#96427=CARTESIAN_POINT('Ctrl Pts',(1.80091438683262,1.54336927997675,19.4636221265878));
#96428=CARTESIAN_POINT('Ctrl Pts',(1.81418051243925,1.52776830562045,19.4622508233453));
#96429=CARTESIAN_POINT('Ctrl Pts',(1.821471939502,1.51906777109398,19.4614881305742));
#96430=CARTESIAN_POINT('Ctrl Pts',(1.83988392743178,1.49677440589022,19.4595389256816));
#96431=CARTESIAN_POINT('Ctrl Pts',(1.85091632151539,1.4831099859008,19.4583488924076));
#96432=CARTESIAN_POINT('Ctrl Pts',(1.91841767960669,1.39757835045672,19.4509274359899));
#96433=CARTESIAN_POINT('Ctrl Pts',(1.97083781475041,1.32262848766791,19.444538577251));
#96434=CARTESIAN_POINT('Ctrl Pts',(2.1279305802648,1.06786792929575,19.4231832461695));
#96435=CARTESIAN_POINT('Ctrl Pts',(2.21330423888941,0.877327039506695,19.4076739070152));
#96436=CARTESIAN_POINT('Ctrl Pts',(2.28108809074832,0.650143787249741,19.3908366525989));
#96437=CARTESIAN_POINT('Ctrl Pts',(2.28891590403338,0.622024096419955,19.3887819696381));
#96438=CARTESIAN_POINT('Ctrl Pts',(2.30114636235901,0.574726216142021,19.385382527452));
#96439=CARTESIAN_POINT('Ctrl Pts',(2.30583288043755,0.555625409614157,19.384024970706));
#96440=CARTESIAN_POINT('Ctrl Pts',(2.31200065555246,0.529064080399357,19.382160332651));
#96441=CARTESIAN_POINT('Ctrl Pts',(2.3136842836461,0.521652060381731,19.3816424879022));
#96442=CARTESIAN_POINT('Ctrl Pts',(2.3164766239762,0.509079532060504,19.3807684603905));
#96443=CARTESIAN_POINT('Ctrl Pts',(2.31760378524778,0.503923224353551,19.3804112395059));
#96444=CARTESIAN_POINT('Ctrl Pts',(2.31972972099569,0.494039902027675,19.3797289642144));
#96445=CARTESIAN_POINT('Ctrl Pts',(2.32073127351936,0.489313560459673,19.3794037466331));
#96446=CARTESIAN_POINT('Ctrl Pts',(2.3230889870294,0.478017386294966,19.3786289098032));
#96447=CARTESIAN_POINT('Ctrl Pts',(2.32443174008037,0.471444749385867,19.3781800486682));
#96448=CARTESIAN_POINT('Ctrl Pts',(2.32913603649639,0.447908952094694,19.3765795020276));
#96449=CARTESIAN_POINT('Ctrl Pts',(2.33234002527015,0.430914325105343,19.3754363476759));
#96450=CARTESIAN_POINT('Ctrl Pts',(2.36521876131017,0.24539536965729,19.3630787464496));
#96451=CARTESIAN_POINT('Ctrl Pts',(2.37676259289263,0.0741408232858691,
19.3527362204046));
#96452=CARTESIAN_POINT('Ctrl Pts',(2.36341513740825,-0.252327964506718,
19.332696214678));
#96453=CARTESIAN_POINT('Ctrl Pts',(2.34178353180174,-0.406744094267162,
19.3230683148398));
#96454=CARTESIAN_POINT('Ctrl Pts',(2.29997836458666,-0.579473342540759,
19.3114789476771));
#96455=CARTESIAN_POINT('Ctrl Pts',(2.2944599293526,-0.600952086304352,19.3100236207595));
#96456=CARTESIAN_POINT('Ctrl Pts',(2.28567375401478,-0.633262543399366,
19.3078114533882));
#96457=CARTESIAN_POINT('Ctrl Pts',(2.28262825904641,-0.644153849746004,
19.3070618093151));
#96458=CARTESIAN_POINT('Ctrl Pts',(2.27698524163552,-0.663791771619905,
19.3057027815364));
#96459=CARTESIAN_POINT('Ctrl Pts',(2.27441490293912,-0.672546022200261,
19.3050942942144));
#96460=CARTESIAN_POINT('Ctrl Pts',(2.26879692706143,-0.691279566124195,
19.3037863624069));
#96461=CARTESIAN_POINT('Ctrl Pts',(2.2657338280945,-0.701253983206915,19.3030864225291));
#96462=CARTESIAN_POINT('Ctrl Pts',(2.25733452090882,-0.727975170529574,
19.3012015829373));
#96463=CARTESIAN_POINT('Ctrl Pts',(2.25187789131268,-0.744683101544696,
19.3000127511698));
#96464=CARTESIAN_POINT('Ctrl Pts',(2.22483190791318,-0.824480022631643,
19.294284174069));
#96465=CARTESIAN_POINT('Ctrl Pts',(2.20077602588636,-0.886694804547859,
19.2896636893009));
#96466=CARTESIAN_POINT('Ctrl Pts',(2.09676334990071,-1.12528456208013,19.2713207105903));
#96467=CARTESIAN_POINT('Ctrl Pts',(1.99795744969515,-1.29260541247844,19.2570083941157));
#96468=CARTESIAN_POINT('Ctrl Pts',(1.84564809411906,-1.49061935623535,19.2389247049613));
#96469=CARTESIAN_POINT('Ctrl Pts',(1.80977044175354,-1.53398004786865,19.2348896480655));
#96470=CARTESIAN_POINT('Ctrl Pts',(1.75837717564129,-1.59177635755103,19.2294469920694));
#96471=CARTESIAN_POINT('Ctrl Pts',(1.74416224446116,-1.60733954083286,19.2279747010726));
#96472=CARTESIAN_POINT('Ctrl Pts',(1.71924647937187,-1.63389867852809,19.2254535015569));
#96473=CARTESIAN_POINT('Ctrl Pts',(1.70864313758474,-1.64498389295039,19.2243985145924));
#96474=CARTESIAN_POINT('Ctrl Pts',(1.69312908157624,-1.66089111879631,19.2228816977405));
#96475=CARTESIAN_POINT('Ctrl Pts',(1.68830402886305,-1.66579557705312,19.2224136297586));
#96476=CARTESIAN_POINT('Ctrl Pts',(1.67982574648213,-1.67433870755467,19.2215976921519));
#96477=CARTESIAN_POINT('Ctrl Pts',(1.67618190253589,-1.67798655473388,19.2212491020098));
#96478=CARTESIAN_POINT('Ctrl Pts',(1.66842847112013,-1.68569804503254,19.220511813399));
#96479=CARTESIAN_POINT('Ctrl Pts',(1.66431591594802,-1.68975856145586,19.2201233567907));
#96480=CARTESIAN_POINT('Ctrl Pts',(1.65311371666262,-1.70073843977101,19.219072167911));
#96481=CARTESIAN_POINT('Ctrl Pts',(1.64599539693776,-1.70762857865914,19.2184116749844));
#96482=CARTESIAN_POINT('Ctrl Pts',(1.61276929722372,-1.7393887910815,19.2153619560181));
#96483=CARTESIAN_POINT('Ctrl Pts',(1.58613810319798,-1.76370758314151,19.2130119297252));
#96484=CARTESIAN_POINT('Ctrl Pts',(1.37309442202791,-1.94952200625935,19.1948382814933));
#96485=CARTESIAN_POINT('Ctrl Pts',(1.16306635384933,-2.0816657986593,19.180431777314));
#96486=CARTESIAN_POINT('Ctrl Pts',(0.896647951783794,-2.19615434743124,
19.1620858363049));
#96487=CARTESIAN_POINT('Ctrl Pts',(0.856423127097393,-2.2121506614815,19.1593193701576));
#96488=CARTESIAN_POINT('Ctrl Pts',(0.786758936108575,-2.23766932286812,
19.1545173117106));
#96489=CARTESIAN_POINT('Ctrl Pts',(0.757528998682597,-2.24773292300983,
19.1524992912835));
#96490=CARTESIAN_POINT('Ctrl Pts',(0.715822501933081,-2.26118618199805,
19.149611583108));
#96491=CARTESIAN_POINT('Ctrl Pts',(0.703501243442268,-2.26504984344146,
19.1487574656509));
#96492=CARTESIAN_POINT('Ctrl Pts',(0.682207905543772,-2.27153644102507,
19.1472793851924));
#96493=CARTESIAN_POINT('Ctrl Pts',(0.673250647471314,-2.27420733238551,
19.1466570058537));
#96494=CARTESIAN_POINT('Ctrl Pts',(0.656069858292932,-2.2792199347792,19.1454619593861));
#96495=CARTESIAN_POINT('Ctrl Pts',(0.647848976926148,-2.2815702640576,19.1448895846303));
#96496=CARTESIAN_POINT('Ctrl Pts',(0.628521422363691,-2.28698308253088,
19.1435425282315));
#96497=CARTESIAN_POINT('Ctrl Pts',(0.61740486850121,-2.29000917428923,19.1427666768551));
#96498=CARTESIAN_POINT('Ctrl Pts',(0.578946718868338,-2.30017767361133,
19.1400786300085));
#96499=CARTESIAN_POINT('Ctrl Pts',(0.551500726367081,-2.30691210532085,
19.1381533613131));
#96500=CARTESIAN_POINT('Ctrl Pts',(0.346650282882144,-2.35331183911892,
19.1237264707463));
#96501=CARTESIAN_POINT('Ctrl Pts',(0.165363106866224,-2.37294604550088,
19.1105722474374));
#96502=CARTESIAN_POINT('Ctrl Pts',(-0.158489839592776,-2.37071398866252,
19.0869132045793));
#96503=CARTESIAN_POINT('Ctrl Pts',(-0.300274715566463,-2.35695745070675,
19.0765235020582));
#96504=CARTESIAN_POINT('Ctrl Pts',(-0.452482285816575,-2.32822239836764,
19.0658374058627));
#96505=CARTESIAN_POINT('Ctrl Pts',(-0.464958590656073,-2.32576294628314,
19.0649650991082));
#96506=CARTESIAN_POINT('Ctrl Pts',(-0.483660835030993,-2.32191966245373,
19.0636635453347));
#96507=CARTESIAN_POINT('Ctrl Pts',(-0.48990170641114,-2.3206109201495,19.0632302368633));
#96508=CARTESIAN_POINT('Ctrl Pts',(-0.500650000530844,-2.31831165628882,
19.0624858150292));
#96509=CARTESIAN_POINT('Ctrl Pts',(-0.505159866614682,-2.31733313728532,
19.0621740277182));
#96510=CARTESIAN_POINT('Ctrl Pts',(-0.515442562472784,-2.31507062519926,
19.0614644359696));
#96511=CARTESIAN_POINT('Ctrl Pts',(-0.521213457382012,-2.3137782021312,
19.0610671194011));
#96512=CARTESIAN_POINT('Ctrl Pts',(-0.536967421617674,-2.31018808522019,
19.0599848580806));
#96513=CARTESIAN_POINT('Ctrl Pts',(-0.546940680980112,-2.30784724407641,
19.0593023261981));
#96514=CARTESIAN_POINT('Ctrl Pts',(-0.596805472431441,-2.29580198803152,
19.0559014046275));
#96515=CARTESIAN_POINT('Ctrl Pts',(-0.636458236015943,-2.2851269011834,
19.053234321735));
#96516=CARTESIAN_POINT('Ctrl Pts',(-0.907081331865152,-2.20467935926936,
19.0351635044363));
#96517=CARTESIAN_POINT('Ctrl Pts',(-1.12651865824161,-2.10104499769973,
19.0210362521405));
#96518=CARTESIAN_POINT('Ctrl Pts',(-1.38054059284589,-1.92964911561629,
19.0016442512426));
#96519=CARTESIAN_POINT('Ctrl Pts',(-1.43299081159047,-1.89102462986639,
18.9974598435712));
#96520=CARTESIAN_POINT('Ctrl Pts',(-1.49698083985673,-1.83970993713107,
18.9920821122248));
#96521=CARTESIAN_POINT('Ctrl Pts',(-1.51006545585992,-1.82898512349717,
18.9909674577762));
#96522=CARTESIAN_POINT('Ctrl Pts',(-1.53084486924783,-1.81157828226521,
18.9891723981157));
#96523=CARTESIAN_POINT('Ctrl Pts',(-1.5386134475841,-1.80498491402518,18.9884956116562));
#96524=CARTESIAN_POINT('Ctrl Pts',(-1.55328527459743,-1.79236905787066,
18.9872064273893));
#96525=CARTESIAN_POINT('Ctrl Pts',(-1.56019660449998,-1.78635621731257,
18.9865944356143));
#96526=CARTESIAN_POINT('Ctrl Pts',(-1.57585174922727,-1.7725761223244,18.9851973090798));
#96527=CARTESIAN_POINT('Ctrl Pts',(-1.5845732374067,-1.76478397877312,18.984411140988));
#96528=CARTESIAN_POINT('Ctrl Pts',(-1.60708548293363,-1.74436917616835,
18.9823611553451));
#96529=CARTESIAN_POINT('Ctrl Pts',(-1.62078503102436,-1.73164760284145,
18.9810931664466));
#96530=CARTESIAN_POINT('Ctrl Pts',(-1.74669958483512,-1.61191852321592,
18.9692438249788));
#96531=CARTESIAN_POINT('Ctrl Pts',(-1.84829611080618,-1.49433098502667,
18.9581849903403));
#96532=CARTESIAN_POINT('Ctrl Pts',(-2.00162157045803,-1.27710773386986,
18.9388346698566));
#96533=CARTESIAN_POINT('Ctrl Pts',(-2.05913226282864,-1.18214548026865,
18.9306851298374));
#96534=CARTESIAN_POINT('Ctrl Pts',(-2.14283194294092,-1.01916676607044,
18.9174739851719));
#96535=CARTESIAN_POINT('Ctrl Pts',(-2.17291820085267,-0.953340673476525,
18.9123327896251));
#96536=CARTESIAN_POINT('Ctrl Pts',(-2.20426368555865,-0.875530051789763,
18.9065555376872));
#96537=CARTESIAN_POINT('Ctrl Pts',(-2.20849820304283,-0.864793020247135,
18.9057648215134));
#96538=CARTESIAN_POINT('Ctrl Pts',(-2.21486286283677,-0.84830311903016,
18.904560804249));
#96539=CARTESIAN_POINT('Ctrl Pts',(-2.21704927240024,-0.842572376030845,
18.9041442770434));
#96540=CARTESIAN_POINT('Ctrl Pts',(-2.22101587408609,-0.83205327074183,
18.9033832891466));
#96541=CARTESIAN_POINT('Ctrl Pts',(-2.22280282413186,-0.827267649808519,
18.9030384390758));
#96542=CARTESIAN_POINT('Ctrl Pts',(-2.22677950991498,-0.816511795892212,
18.9022664011495));
#96543=CARTESIAN_POINT('Ctrl Pts',(-2.22896070176143,-0.810538519138946,
18.9018397235281));
#96544=CARTESIAN_POINT('Ctrl Pts',(-2.234481083762,-0.79522993152708,18.9007513393234));
#96545=CARTESIAN_POINT('Ctrl Pts',(-2.23778585189174,-0.785882209569662,
18.9000916112971));
#96546=CARTESIAN_POINT('Ctrl Pts',(-2.25726177810717,-0.729674359324691,
18.8961521952245));
#96547=CARTESIAN_POINT('Ctrl Pts',(-2.27202052389178,-0.682333486275215,
18.892948617959));
#96548=CARTESIAN_POINT('Ctrl Pts',(-2.28912447805736,-0.620735896634144,
18.8888844770757));
#96549=CARTESIAN_POINT('Ctrl Pts',(-2.29283783531148,-0.606876103692446,
18.8879767352116));
#96550=CARTESIAN_POINT('Ctrl Pts',(-2.34630924864452,-0.399799242755879,
18.8745026788418));
#96551=CARTESIAN_POINT('Ctrl Pts',(-2.37161967530902,-0.201087963350939,
18.8626479715626));
#96552=CARTESIAN_POINT('Ctrl Pts',(-2.37178741181482,0.0567324659326155,
18.846463663737));
#96553=CARTESIAN_POINT('Ctrl Pts',(-2.36967752226244,0.114978290712743,
18.8427604081577));
#96554=CARTESIAN_POINT('Ctrl Pts',(-2.36542649320577,0.173076768343595,
18.8389943251842));
#96555=CARTESIAN_POINT('Ctrl Pts',(-2.36542649880509,0.173076691818108,
18.6388842277111));
#96556=CARTESIAN_POINT('Ctrl Pts',(-2.36960585386229,0.115957751674473,
18.6424309278243));
#96557=CARTESIAN_POINT('Ctrl Pts',(-2.37171871494586,0.0586549215548028,
18.6460114842864));
#96558=CARTESIAN_POINT('Ctrl Pts',(-2.37178256024484,-0.0597406771378477,
18.6535160827396));
#96559=CARTESIAN_POINT('Ctrl Pts',(-2.36946063533492,-0.120734203229363,
18.6574407824453));
#96560=CARTESIAN_POINT('Ctrl Pts',(-2.36345772608295,-0.198918322189068,
18.6625793557217));
#96561=CARTESIAN_POINT('Ctrl Pts',(-2.36193456230257,-0.216254522369614,
18.6637255319754));
#96562=CARTESIAN_POINT('Ctrl Pts',(-2.35919764343389,-0.243910801448145,
18.6655655206083));
#96563=CARTESIAN_POINT('Ctrl Pts',(-2.35810658974592,-0.254242611277065,
18.666255471001));
#96564=CARTESIAN_POINT('Ctrl Pts',(-2.35601563001911,-0.272870357030803,
18.6675041972383));
#96565=CARTESIAN_POINT('Ctrl Pts',(-2.35503969215494,-0.281168856620004,
18.6680622086428));
#96566=CARTESIAN_POINT('Ctrl Pts',(-2.35263813537177,-0.300699274452836,
18.6693796079774));
#96567=CARTESIAN_POINT('Ctrl Pts',(-2.35117591036786,-0.311926402276078,
18.6701401391712));
#96568=CARTESIAN_POINT('Ctrl Pts',(-2.34666817821891,-0.344703022866579,
18.6723700923827));
#96569=CARTESIAN_POINT('Ctrl Pts',(-2.34340644515367,-0.366221094842173,
18.6738462953658));
#96570=CARTESIAN_POINT('Ctrl Pts',(-2.31108293187759,-0.561304856341472,
18.687344773823));
#96571=CARTESIAN_POINT('Ctrl Pts',(-2.26308943834641,-0.731142571251129,
18.6999894688802));
#96572=CARTESIAN_POINT('Ctrl Pts',(-2.14053998927671,-1.03225041046977,
18.7237172458917));
#96573=CARTESIAN_POINT('Ctrl Pts',(-2.07138847780926,-1.16482197330694,
18.7346757068148));
#96574=CARTESIAN_POINT('Ctrl Pts',(-1.98005013023606,-1.30573736461901,
18.7463535578338));
#96575=CARTESIAN_POINT('Ctrl Pts',(-1.96968079490732,-1.32132744044284,
18.747645614633));
#96576=CARTESIAN_POINT('Ctrl Pts',(-1.9552001193874,-1.34254948116033,18.7494028038583));
#96577=CARTESIAN_POINT('Ctrl Pts',(-1.95124729590324,-1.34828802915066,
18.749877790829));
#96578=CARTESIAN_POINT('Ctrl Pts',(-1.94444664697418,-1.35806838691302,
18.7506869246753));
#96579=CARTESIAN_POINT('Ctrl Pts',(-1.94161139842078,-1.36211882195922,
18.7510219013372));
#96580=CARTESIAN_POINT('Ctrl Pts',(-1.93569838185847,-1.37051017954972,
18.7517155832062));
#96581=CARTESIAN_POINT('Ctrl Pts',(-1.93261865242142,-1.37484963640894,
18.7520741376405));
#96582=CARTESIAN_POINT('Ctrl Pts',(-1.92514136975313,-1.38531064372476,
18.7529381674868));
#96583=CARTESIAN_POINT('Ctrl Pts',(-1.92072913869028,-1.39142173795563,
18.7534426447906));
#96584=CARTESIAN_POINT('Ctrl Pts',(-1.90518273612611,-1.41273918312857,
18.7552018758767));
#96585=CARTESIAN_POINT('Ctrl Pts',(-1.89389615638716,-1.4278342557352,18.7564466238072));
#96586=CARTESIAN_POINT('Ctrl Pts',(-1.82316225612422,-1.52012162712957,
18.7640616808848));
#96587=CARTESIAN_POINT('Ctrl Pts',(-1.75917805844449,-1.59373383438171,
18.770159399917));
#96588=CARTESIAN_POINT('Ctrl Pts',(-1.68030220458323,-1.6739200493627,18.7771050937606));
#96589=CARTESIAN_POINT('Ctrl Pts',(-1.66966376996903,-1.68453160617613,
18.7780308315554));
#96590=CARTESIAN_POINT('Ctrl Pts',(-1.51234417014642,-1.83849919379218,
18.7915717218202));
#96591=CARTESIAN_POINT('Ctrl Pts',(-1.34779376538526,-1.96232197187314,
18.8039547586385));
#96592=CARTESIAN_POINT('Ctrl Pts',(-1.14602435727059,-2.07666716795414,
18.8190159738905));
#96593=CARTESIAN_POINT('Ctrl Pts',(-1.12245284164,-2.08950182492433,18.8207720839803));
#96594=CARTESIAN_POINT('Ctrl Pts',(-1.0878775203179,-2.10757416154482,18.8233456088109));
#96595=CARTESIAN_POINT('Ctrl Pts',(-1.07704256239913,-2.11313171739394,
18.8241517408364));
#96596=CARTESIAN_POINT('Ctrl Pts',(-1.05780105502936,-2.12281479923587,
18.8255829665949));
#96597=CARTESIAN_POINT('Ctrl Pts',(-1.04941190390112,-2.12697446987693,
18.8262068492024));
#96598=CARTESIAN_POINT('Ctrl Pts',(-1.03193706308321,-2.13551063245499,
18.8275062759891));
#96599=CARTESIAN_POINT('Ctrl Pts',(-1.02284766825667,-2.13987906330876,
18.8281820851467));
#96600=CARTESIAN_POINT('Ctrl Pts',(-0.999251037581454,-2.15103508910312,
18.8299364826471));
#96601=CARTESIAN_POINT('Ctrl Pts',(-0.9847026112443,-2.15773384273846,18.8310181098449));
#96602=CARTESIAN_POINT('Ctrl Pts',(-0.921073066539403,-2.18625423359942,
18.8357494281989));
#96603=CARTESIAN_POINT('Ctrl Pts',(-0.871329977319599,-2.20655079836367,
18.8394504281182));
#96604=CARTESIAN_POINT('Ctrl Pts',(-0.733812991353957,-2.2572863752599,
18.8496962696139));
#96605=CARTESIAN_POINT('Ctrl Pts',(-0.644878152731193,-2.28428372151262,
18.8563411367774));
#96606=CARTESIAN_POINT('Ctrl Pts',(-0.449086783957416,-2.33137207037752,
18.8709415087171));
#96607=CARTESIAN_POINT('Ctrl Pts',(-0.341960694182375,-2.34947587670341,
18.8789139601156));
#96608=CARTESIAN_POINT('Ctrl Pts',(-0.211356979913292,-2.36242307796204,
18.8884367504633));
#96609=CARTESIAN_POINT('Ctrl Pts',(-0.188709467621251,-2.36433993965945,
18.8900806435221));
#96610=CARTESIAN_POINT('Ctrl Pts',(-0.144643633172765,-2.36743241347858,
18.8932611980413));
#96611=CARTESIAN_POINT('Ctrl Pts',(-0.123229842556786,-2.36864359223355,
18.8947985445297));
#96612=CARTESIAN_POINT('Ctrl Pts',(-0.0535526134322616,-2.37163708928384,
18.89976859173));
#96613=CARTESIAN_POINT('Ctrl Pts',(-0.00524690536728323,-2.3722359971031,
18.9031641156925));
#96614=CARTESIAN_POINT('Ctrl Pts',(0.0539314152003348,-2.37116173408091,
18.9072368714703));
#96615=CARTESIAN_POINT('Ctrl Pts',(0.0648143623579783,-2.37088921644014,
18.9079822380623));
#96616=CARTESIAN_POINT('Ctrl Pts',(0.081803807107464,-2.37034671545087,
18.9091397905149));
#96617=CARTESIAN_POINT('Ctrl Pts',(0.0879116174798878,-2.37012804801061,
18.9095547174014));
#96618=CARTESIAN_POINT('Ctrl Pts',(0.0992048811247318,-2.36968001930408,
18.9103195708558));
#96619=CARTESIAN_POINT('Ctrl Pts',(0.104390396130632,-2.36945724765325,
18.9106698451967));
#96620=CARTESIAN_POINT('Ctrl Pts',(0.116163107028454,-2.36891276476409,
18.9114630129342));
#96621=CARTESIAN_POINT('Ctrl Pts',(0.122749712598003,-2.36858060137621,
18.9119053185701));
#96622=CARTESIAN_POINT('Ctrl Pts',(0.142849447040167,-2.36748290055367,
18.9132508501642));
#96623=CARTESIAN_POINT('Ctrl Pts',(0.156357775466462,-2.36662914634799,
18.9141493223036));
#96624=CARTESIAN_POINT('Ctrl Pts',(0.300900624114397,-2.3562507208666,18.9237080823717));
#96625=CARTESIAN_POINT('Ctrl Pts',(0.430955604850893,-2.33596799301929,
18.9318298448764));
#96626=CARTESIAN_POINT('Ctrl Pts',(0.745155705811506,-2.25981372510544,
18.9516778417322));
#96627=CARTESIAN_POINT('Ctrl Pts',(0.925437117947199,-2.19216148062066,
18.9633216823021));
#96628=CARTESIAN_POINT('Ctrl Pts',(1.120297736124,-2.09067138269913,18.9775732889336));
#96629=CARTESIAN_POINT('Ctrl Pts',(1.14477142330908,-2.07737144721192,18.9793941266265));
#96630=CARTESIAN_POINT('Ctrl Pts',(1.17895076413854,-2.05800967793005,18.9819838009365));
#96631=CARTESIAN_POINT('Ctrl Pts',(1.18885610893811,-2.05230355533512,18.9827399340325));
#96632=CARTESIAN_POINT('Ctrl Pts',(1.20689403523592,-2.04173813095045,18.9841274225775));
#96633=CARTESIAN_POINT('Ctrl Pts',(1.21503953459712,-2.03690125744204,18.9847579574094));
#96634=CARTESIAN_POINT('Ctrl Pts',(1.23146198743714,-2.02701589253636,18.9860373950893));
#96635=CARTESIAN_POINT('Ctrl Pts',(1.23973739360127,-2.0219651938576,18.9866863699388));
#96636=CARTESIAN_POINT('Ctrl Pts',(1.26005055058218,-2.00939595543441,18.9882900287777));
#96637=CARTESIAN_POINT('Ctrl Pts',(1.27205209400526,-2.00181990963255,18.9892468194956));
#96638=CARTESIAN_POINT('Ctrl Pts',(1.3164001960882,-1.97326505529228,18.9928176640518));
#96639=CARTESIAN_POINT('Ctrl Pts',(1.34830018952424,-1.95160722210424,18.9954568533656));
#96640=CARTESIAN_POINT('Ctrl Pts',(1.42672009400098,-1.89552515993178,19.0021283868771));
#96641=CARTESIAN_POINT('Ctrl Pts',(1.4725325732193,-1.86015933209813,19.0061945277994));
#96642=CARTESIAN_POINT('Ctrl Pts',(1.60863985601224,-1.74690783626517,19.0187990021559));
#96643=CARTESIAN_POINT('Ctrl Pts',(1.69439032680061,-1.66386479894757,19.0274988529642));
#96644=CARTESIAN_POINT('Ctrl Pts',(1.85513170142364,-1.4828317884799,19.0451801493841));
#96645=CARTESIAN_POINT('Ctrl Pts',(1.92947686536043,-1.38471265401808,19.0541345733921));
#96646=CARTESIAN_POINT('Ctrl Pts',(2.00627662577104,-1.26507789468366,19.0640264443602));
#96647=CARTESIAN_POINT('Ctrl Pts',(2.01646992189924,-1.2487662280536,19.0653543167582));
#96648=CARTESIAN_POINT('Ctrl Pts',(2.03052734570979,-1.2256499975811,19.0672050916567));
#96649=CARTESIAN_POINT('Ctrl Pts',(2.03455763301484,-1.21894809593416,19.0677380517976));
#96650=CARTESIAN_POINT('Ctrl Pts',(2.04127502980425,-1.20765170541397,19.0686301578468));
#96651=CARTESIAN_POINT('Ctrl Pts',(2.04397992874673,-1.20306792896309,19.0689904401363));
#96652=CARTESIAN_POINT('Ctrl Pts',(2.04946456349759,-1.19370166418243,19.0697230816299));
#96653=CARTESIAN_POINT('Ctrl Pts',(2.05224303413521,-1.18891849617883,19.0700953592895));
#96654=CARTESIAN_POINT('Ctrl Pts',(2.05927616241807,-1.17671277037519,19.071040708387));
#96655=CARTESIAN_POINT('Ctrl Pts',(2.06350748505046,-1.16927675161346,19.071612295602));
#96656=CARTESIAN_POINT('Ctrl Pts',(2.08051541374976,-1.13900757518601,19.0739221230864));
#96657=CARTESIAN_POINT('Ctrl Pts',(2.09295460169205,-1.11598558235589,19.0756401315038));
#96658=CARTESIAN_POINT('Ctrl Pts',(2.12477794819871,-1.05468354674276,19.0801259700997));
#96659=CARTESIAN_POINT('Ctrl Pts',(2.1435094401328,-1.01607403925689,19.0828616548797));
#96660=CARTESIAN_POINT('Ctrl Pts',(2.24875445073026,-0.783259698496598,
19.0989549504641));
#96661=CARTESIAN_POINT('Ctrl Pts',(2.30988531194409,-0.578647529580843,
19.1115481072305));
#96662=CARTESIAN_POINT('Ctrl Pts',(2.35334942230048,-0.302389102565685,
19.1292140576278));
#96663=CARTESIAN_POINT('Ctrl Pts',(2.36095547297555,-0.235755413113114,
19.1335151208604));
#96664=CARTESIAN_POINT('Ctrl Pts',(2.36700870509727,-0.150966454101397,
19.1390821079322));
#96665=CARTESIAN_POINT('Ctrl Pts',(2.36808470633828,-0.133025840973636,
19.140265262001));
#96666=CARTESIAN_POINT('Ctrl Pts',(2.3694668286772,-0.104573230352077,19.1421506941763));
#96667=CARTESIAN_POINT('Ctrl Pts',(2.36990712491347,-0.0940681982777818,
19.1428487645939));
#96668=CARTESIAN_POINT('Ctrl Pts',(2.37057132597695,-0.0752275191216445,
19.1441043841442));
#96669=CARTESIAN_POINT('Ctrl Pts',(2.37082115024523,-0.0668929119218101,
19.1446611114527));
#96670=CARTESIAN_POINT('Ctrl Pts',(2.37130222529585,-0.0474138224384436,
19.1459653218307));
#96671=CARTESIAN_POINT('Ctrl Pts',(2.37149886862469,-0.0362687604916444,
19.1467138762243));
#96672=CARTESIAN_POINT('Ctrl Pts',(2.37183853270492,-0.00420425298295702,
19.1488744386249));
#96673=CARTESIAN_POINT('Ctrl Pts',(2.37178334471784,0.0167157921117499,
19.150292598664));
#96674=CARTESIAN_POINT('Ctrl Pts',(2.3688273780653,0.202992601673781,19.1629996234797));
#96675=CARTESIAN_POINT('Ctrl Pts',(2.34891567886943,0.367591883083198,19.174834131301));
#96676=CARTESIAN_POINT('Ctrl Pts',(2.27593733976225,0.686702966076191,19.1986951394924));
#96677=CARTESIAN_POINT('Ctrl Pts',(2.22372148604837,0.840549176717783,19.2106419894999));
#96678=CARTESIAN_POINT('Ctrl Pts',(2.14868564190265,1.00432836779843,19.2231611152709));
#96679=CARTESIAN_POINT('Ctrl Pts',(2.14096083079876,1.02069203435124,19.2244092094301));
#96680=CARTESIAN_POINT('Ctrl Pts',(2.1300394736735,1.0431573663133,19.2261173166618));
#96681=CARTESIAN_POINT('Ctrl Pts',(2.12700274607811,1.04933539513049,19.2265864839681));
#96682=CARTESIAN_POINT('Ctrl Pts',(2.12174885205832,1.05990758724572,19.2273882645834));
#96683=CARTESIAN_POINT('Ctrl Pts',(2.11954484977422,1.0643081864028,19.2277216759355));
#96684=CARTESIAN_POINT('Ctrl Pts',(2.11492146784913,1.07346809490425,19.2284149500984));
#96685=CARTESIAN_POINT('Ctrl Pts',(2.11249969904126,1.07822613037188,19.2287746485647));
#96686=CARTESIAN_POINT('Ctrl Pts',(2.10657728251937,1.08976531998421,19.2296460683405));
#96687=CARTESIAN_POINT('Ctrl Pts',(2.10305989129882,1.0965379143184,19.2301567486535));
#96688=CARTESIAN_POINT('Ctrl Pts',(2.09046457048215,1.12050615022578,19.231961717272));
#96689=CARTESIAN_POINT('Ctrl Pts',(2.08120763434184,1.13760757581048,19.2332452939246));
#96690=CARTESIAN_POINT('Ctrl Pts',(2.05779695554892,1.17961443592142,19.2363924265068));
#96691=CARTESIAN_POINT('Ctrl Pts',(2.04340005809985,1.20438153795247,19.2382428803413));
#96692=CARTESIAN_POINT('Ctrl Pts',(1.9202798697087,1.4076200712671,19.2534368949746));
#96693=CARTESIAN_POINT('Ctrl Pts',(1.7888471003349,1.57127770350817,19.2658063500539));
#96694=CARTESIAN_POINT('Ctrl Pts',(1.57206888208808,1.77820637888635,19.284520110327));
#96695=CARTESIAN_POINT('Ctrl Pts',(1.50295663019337,1.83699126730792,19.2902815955152));
#96696=CARTESIAN_POINT('Ctrl Pts',(1.4165512462419,1.90233891104908,19.297364011117));
#96697=CARTESIAN_POINT('Ctrl Pts',(1.40232869095856,1.91284734893101,19.2985259672059));
#96698=CARTESIAN_POINT('Ctrl Pts',(1.3786857315032,1.92991071927386,19.3004520596908));
#96699=CARTESIAN_POINT('Ctrl Pts',(1.36933272425729,1.9365581873643,19.3012126168562));
#96700=CARTESIAN_POINT('Ctrl Pts',(1.35234826184569,1.94844500163773,19.3025914346006));
#96701=CARTESIAN_POINT('Ctrl Pts',(1.34473362532725,1.95370806889323,19.3032087728965));
#96702=CARTESIAN_POINT('Ctrl Pts',(1.32834474694658,1.96489449257834,19.3045358068088));
#96703=CARTESIAN_POINT('Ctrl Pts',(1.31956129249625,1.97080392803043,19.3052460117351));
#96704=CARTESIAN_POINT('Ctrl Pts',(1.29548507654745,1.98676910116397,19.3071901969432));
#96705=CARTESIAN_POINT('Ctrl Pts',(1.2801152756355,1.99670676194119,19.3084285538078));
#96706=CARTESIAN_POINT('Ctrl Pts',(1.1950882629761,2.05029747795338,19.3152656418944));
#96707=CARTESIAN_POINT('Ctrl Pts',(1.12332058878302,2.09047930759519,19.320989837225));
#96708=CARTESIAN_POINT('Ctrl Pts',(0.860833226062364,2.22001905152122,19.3417736551214));
#96709=CARTESIAN_POINT('Ctrl Pts',(0.660513824287204,2.28762388462553,19.3574606796617));
#96710=CARTESIAN_POINT('Ctrl Pts',(0.404380602763094,2.3375675237912,19.3760821309725));
#96711=CARTESIAN_POINT('Ctrl Pts',(0.354540247288059,2.34564441116114,19.3796348894492));
#96712=CARTESIAN_POINT('Ctrl Pts',(0.294495923733967,2.35341698054325,19.3838020314702));
#96713=CARTESIAN_POINT('Ctrl Pts',(0.284507502669724,2.35464537103996,19.384491503903));
#96714=CARTESIAN_POINT('Ctrl Pts',(0.268102744439084,2.35655693942311,19.3856174245552));
#96715=CARTESIAN_POINT('Ctrl Pts',(0.261691026148367,2.3572775610152,19.3860558699821));
#96716=CARTESIAN_POINT('Ctrl Pts',(0.250123689809365,2.35852985213008,19.3868438589733));
#96717=CARTESIAN_POINT('Ctrl Pts',(0.244969232779565,2.35907079167362,19.3871939075083));
#96718=CARTESIAN_POINT('Ctrl Pts',(0.23361661373494,2.360224593243,19.3879625016301));
#96719=CARTESIAN_POINT('Ctrl Pts',(0.227417803490441,2.36082993832145,19.388380623408));
#96720=CARTESIAN_POINT('Ctrl Pts',(0.209528703472811,2.36250578633685,19.3895829963485));
#96721=CARTESIAN_POINT('Ctrl Pts',(0.197832548232664,2.36351394433449,19.390363855012));
#96722=CARTESIAN_POINT('Ctrl Pts',(0.111694493764132,2.37029475925463,19.3960790336162));
#96723=CARTESIAN_POINT('Ctrl Pts',(0.0370159239255071,2.37263677720445,
19.4008389510381));
#96724=CARTESIAN_POINT('Ctrl Pts',(-0.202184964010994,2.36883847254191,
19.4158134530331));
#96725=CARTESIAN_POINT('Ctrl Pts',(-0.365998432568143,2.34911136622944,
19.4256854104883));
#96726=CARTESIAN_POINT('Ctrl Pts',(-0.623700839572435,2.2904457886415,19.4421285496156));
#96727=CARTESIAN_POINT('Ctrl Pts',(-0.719441000451815,2.26219926962089,
19.448443855865));
#96728=CARTESIAN_POINT('Ctrl Pts',(-0.830070648555137,2.22182508104026,
19.4561397668617));
#96729=CARTESIAN_POINT('Ctrl Pts',(-0.846957936076613,2.21544266393317,
19.4573256330484));
#96730=CARTESIAN_POINT('Ctrl Pts',(-0.874562108324556,2.20464814710041,
19.4592831938697));
#96731=CARTESIAN_POINT('Ctrl Pts',(-0.885322637395361,2.20034909809023,
19.460051101131));
#96732=CARTESIAN_POINT('Ctrl Pts',(-0.904630071332128,2.19247083218566,
19.4614378467492));
#96733=CARTESIAN_POINT('Ctrl Pts',(-0.913188376840121,2.188920030553,19.4620557146923));
#96734=CARTESIAN_POINT('Ctrl Pts',(-0.921884193083915,2.18525230275268,
19.4626868015243));
#96735=CARTESIAN_POINT('Ctrl Pts',(-0.92204282604314,2.18518537407842,19.4626983152102));
#96736=CARTESIAN_POINT('Ctrl Pts',(-0.922346631466237,2.18505715686209,
19.4627203677528));
#96737=CARTESIAN_POINT('Ctrl Pts',(-0.922491805121438,2.18499587112084,
19.4627309065144));
#96738=CARTESIAN_POINT('Ctrl Pts',(-0.9227698706679,2.18487845179058,19.4627510942486));
#96739=CARTESIAN_POINT('Ctrl Pts',(-0.922902763550764,2.1848223205427,19.4627607431415));
#96740=CARTESIAN_POINT('Ctrl Pts',(-0.923157339105347,2.18471476564036,
19.4627792284981));
#96741=CARTESIAN_POINT('Ctrl Pts',(-0.923279022605258,2.18466334394298,
19.4627880648951));
#96742=CARTESIAN_POINT('Ctrl Pts',(-0.923512153708541,2.18456480313434,
19.4628049956431));
#96743=CARTESIAN_POINT('Ctrl Pts',(-0.923623602006379,2.18451768565913,
19.4628130899383));
#96744=CARTESIAN_POINT('Ctrl Pts',(-0.923837148880787,2.18442738426728,
19.4628286005348));
#96745=CARTESIAN_POINT('Ctrl Pts',(-0.923939248037813,2.18438420172008,
19.4628360167893));
#96746=CARTESIAN_POINT('Ctrl Pts',(-0.924134902921061,2.18430143387371,
19.4628502296128));
#96747=CARTESIAN_POINT('Ctrl Pts',(-0.924228459140427,2.18426184971825,
19.462857026143));
#96748=CARTESIAN_POINT('Ctrl Pts',(-0.924407762068903,2.18418597207209,
19.4628700526178));
#96749=CARTESIAN_POINT('Ctrl Pts',(-0.924493509197177,2.1841496795371,19.4628762825303));
#96750=CARTESIAN_POINT('Ctrl Pts',(-0.924657862316789,2.18408010554611,
19.4628882241481));
#96751=CARTESIAN_POINT('Ctrl Pts',(-0.924736468648707,2.18404682489586,
19.4628939358259));
#96752=CARTESIAN_POINT('Ctrl Pts',(-0.924887149132199,2.18398301962184,
19.4629048850696));
#96753=CARTESIAN_POINT('Ctrl Pts',(-0.924959223556996,2.18395249567917,
19.4629101226115));
#96754=CARTESIAN_POINT('Ctrl Pts',(-0.925097395246018,2.1838939710897,19.4629201637881));
#96755=CARTESIAN_POINT('Ctrl Pts',(-0.925163492758077,2.18386597100659,
19.462924967404));
#96756=CARTESIAN_POINT('Ctrl Pts',(-0.925330229361803,2.18379532948391,
19.462937085426));
#96757=CARTESIAN_POINT('Ctrl Pts',(-0.925430866752822,2.18375268409855,
19.4629443999654));
#96758=CARTESIAN_POINT('Ctrl Pts',(-0.925630249183668,2.1836681789592,19.4629588923997));
#96759=CARTESIAN_POINT('Ctrl Pts',(-0.925728994335965,2.18362631946232,
19.462966070286));
#96760=CARTESIAN_POINT('Ctrl Pts',(-0.925924639110301,2.18354336715959,
19.4629802927676));
#96761=CARTESIAN_POINT('Ctrl Pts',(-0.926021538843426,2.18350227459836,
19.4629873373549));
#96762=CARTESIAN_POINT('Ctrl Pts',(-0.926213538302597,2.18342083773069,
19.4630012965003));
#96763=CARTESIAN_POINT('Ctrl Pts',(-0.926308638126264,2.18338049366213,
19.4630082110502));
#96764=CARTESIAN_POINT('Ctrl Pts',(-0.926497081956118,2.18330053586517,
19.4630219132879));
#96765=CARTESIAN_POINT('Ctrl Pts',(-0.926590426071098,2.18326092235805,
19.463028700969));
#96766=CARTESIAN_POINT('Ctrl Pts',(-0.936804601029095,2.17892544334773,
19.463771485232));
#96767=CARTESIAN_POINT('Ctrl Pts',(-0.946895289193552,2.17455932372564,
19.4645098683679));
#96768=CARTESIAN_POINT('Ctrl Pts',(-0.975676854756248,2.16186757175691,
19.4666292988969));
#96769=CARTESIAN_POINT('Ctrl Pts',(-0.994290451729112,2.1533701898398,19.4680161922149));
#96770=CARTESIAN_POINT('Ctrl Pts',(-1.03609773427408,2.13362693034339,19.4711689141561));
#96771=CARTESIAN_POINT('Ctrl Pts',(-1.05922239361368,2.12224179187999,19.472939394091));
#96772=CARTESIAN_POINT('Ctrl Pts',(-1.13312783338187,2.08434655753697,19.4786855659897));
#96773=CARTESIAN_POINT('Ctrl Pts',(-1.18313208579832,2.05637467735449,19.4827096826433));
#96774=CARTESIAN_POINT('Ctrl Pts',(-1.34789701557225,1.9562069269485,19.496430628623));
#96775=CARTESIAN_POINT('Ctrl Pts',(-1.45746398793284,1.87599691445871,19.5063566201135));
#96776=CARTESIAN_POINT('Ctrl Pts',(-1.64794564657305,1.70974644259325,19.5248002727797));
#96777=CARTESIAN_POINT('Ctrl Pts',(-1.73048844658271,1.6261532402266,19.5332973220643));
#96778=CARTESIAN_POINT('Ctrl Pts',(-1.81479087967416,1.52705445754513,19.5422756807723));
#96779=CARTESIAN_POINT('Ctrl Pts',(-1.82298972662788,1.51725730452842,19.5431522655787));
#96780=CARTESIAN_POINT('Ctrl Pts',(-1.83525806332084,1.50235432429424,19.5444685024982));
#96781=CARTESIAN_POINT('Ctrl Pts',(-1.83938612578529,1.49729735108902,19.5449121867768));
#96782=CARTESIAN_POINT('Ctrl Pts',(-1.84675626641251,1.48819227625998,19.5457056655387));
#96783=CARTESIAN_POINT('Ctrl Pts',(-1.85000597951484,1.4841505436037,19.5460559992093));
#96784=CARTESIAN_POINT('Ctrl Pts',(-1.857089269066,1.47528150057555,19.5468206271378));
#96785=CARTESIAN_POINT('Ctrl Pts',(-1.86091728860406,1.47044989931184,19.5472345271177));
#96786=CARTESIAN_POINT('Ctrl Pts',(-1.87179400487539,1.45661116132722,19.5484126680337));
#96787=CARTESIAN_POINT('Ctrl Pts',(-1.87879656764788,1.44756773330525,19.5491737248964));
#96788=CARTESIAN_POINT('Ctrl Pts',(-1.92607970393777,1.38558300980043,19.5543329012951));
#96789=CARTESIAN_POINT('Ctrl Pts',(-1.96418711655136,1.33101245336678,19.5585929418024));
#96790=CARTESIAN_POINT('Ctrl Pts',(-2.07840825189903,1.15183306441105,19.5719554566838));
#96791=CARTESIAN_POINT('Ctrl Pts',(-2.14533942665075,1.02177488207393,19.5807552380452));
#96792=CARTESIAN_POINT('Ctrl Pts',(-2.22354038883136,0.827689724622768,
19.5936650268779));
#96793=CARTESIAN_POINT('Ctrl Pts',(-2.24482944561364,0.768076948163438,
19.5975994103254));
#96794=CARTESIAN_POINT('Ctrl Pts',(-2.28379299174548,0.643442580024122,
19.6058471351649));
#96795=CARTESIAN_POINT('Ctrl Pts',(-2.30113161261755,0.578377694243966,
19.6101649591812));
#96796=CARTESIAN_POINT('Ctrl Pts',(-2.31956902568924,0.495097419101356,
19.6157509306108));
#96797=CARTESIAN_POINT('Ctrl Pts',(-2.32325877702115,0.477483554385752,
19.6169355980639));
#96798=CARTESIAN_POINT('Ctrl Pts',(-2.32878712481555,0.449510008111972,
19.6188228898157));
#96799=CARTESIAN_POINT('Ctrl Pts',(-2.3307578939416,0.439176904965135,19.6195212920108));
#96800=CARTESIAN_POINT('Ctrl Pts',(-2.33416737018052,0.420630799270693,
19.6207772011715));
#96801=CARTESIAN_POINT('Ctrl Pts',(-2.33563163988689,0.412422624268697,
19.6213338839945));
#96802=CARTESIAN_POINT('Ctrl Pts',(-2.33855590238336,0.395515061029755,
19.6224823656931));
#96803=CARTESIAN_POINT('Ctrl Pts',(-2.34001070242373,0.386814918227326,
19.6230743202251));
#96804=CARTESIAN_POINT('Ctrl Pts',(-2.34315544535991,0.367341184528241,
19.6244015793265));
#96805=CARTESIAN_POINT('Ctrl Pts',(-2.34481967442248,0.35656370325153,19.6251376861328));
#96806=CARTESIAN_POINT('Ctrl Pts',(-2.34880486843972,0.329520425336842,
19.6269887985295));
#96807=CARTESIAN_POINT('Ctrl Pts',(-2.35103121423866,0.31324148301411,19.628106753869));
#96808=CARTESIAN_POINT('Ctrl Pts',(-2.35828550765783,0.25575535628729,19.6320680853066));
#96809=CARTESIAN_POINT('Ctrl Pts',(-2.36239902303451,0.214452987595711,
19.6349387342668));
#96810=CARTESIAN_POINT('Ctrl Pts',(-2.36542650053005,0.173076668243166,
19.6378399312857));
#96811=CARTESIAN_POINT('Origin',(0.,0.,-1.84858989190503));
#96812=CARTESIAN_POINT('',(-2.3654264754702,0.173077010733998,20.8359749974364));
#96813=CARTESIAN_POINT('',(-2.36542650966497,0.173076543396847,20.6413652673669));
#96814=CARTESIAN_POINT('',(-2.36542649454111,0.173076750093529,-1.84858989190503));
#96815=CARTESIAN_POINT('',(-2.37174975346702,-0.0010814014724484,19.8466119453452));
#96816=CARTESIAN_POINT('Ctrl Pts',(-2.3654264754702,0.173077010733998,20.8359749974364));
#96817=CARTESIAN_POINT('Ctrl Pts',(-2.35906927455258,0.259960250146641,
20.8296422157243));
#96818=CARTESIAN_POINT('Ctrl Pts',(-2.34792654946133,0.346475014108061,
20.8233719415871));
#96819=CARTESIAN_POINT('Ctrl Pts',(-2.32859917105788,0.450753822994609,
20.8159958757342));
#96820=CARTESIAN_POINT('Ctrl Pts',(-2.32494449007119,0.469240111977688,
20.8146954084924));
#96821=CARTESIAN_POINT('Ctrl Pts',(-2.31948832425912,0.495208164514945,
20.8128805280791));
#96822=CARTESIAN_POINT('Ctrl Pts',(-2.31787028340761,0.502727128830011,
20.8123564483484));
#96823=CARTESIAN_POINT('Ctrl Pts',(-2.31508770824918,0.515358570198658,
20.8114785537713));
#96824=CARTESIAN_POINT('Ctrl Pts',(-2.31394275441837,0.520475248111737,
20.8111236410527));
#96825=CARTESIAN_POINT('Ctrl Pts',(-2.31157221070702,0.530906510228892,
20.8104015748021));
#96826=CARTESIAN_POINT('Ctrl Pts',(-2.31034524259327,0.536220728326226,
20.810034502292));
#96827=CARTESIAN_POINT('Ctrl Pts',(-2.30717339198383,0.549745574775442,
20.8091021816128));
#96828=CARTESIAN_POINT('Ctrl Pts',(-2.30520298505307,0.557950231474603,
20.8085383798383));
#96829=CARTESIAN_POINT('Ctrl Pts',(-2.29702814398103,0.591207124766822,
20.8062596244083));
#96830=CARTESIAN_POINT('Ctrl Pts',(-2.2904584936035,0.616168957468834,20.8045644019244));
#96831=CARTESIAN_POINT('Ctrl Pts',(-2.22920453016805,0.83437179189627,20.7898388695554));
#96832=CARTESIAN_POINT('Ctrl Pts',(-2.15058191588978,1.02007361119127,20.7778968074392));
#96833=CARTESIAN_POINT('Ctrl Pts',(-1.99014054526828,1.29554627669857,20.758187094471));
#96834=CARTESIAN_POINT('Ctrl Pts',(-1.9232945957011,1.39285024101216,20.7507732273953));
#96835=CARTESIAN_POINT('Ctrl Pts',(-1.83792938887508,1.49918482565912,20.7418666647132));
#96836=CARTESIAN_POINT('Ctrl Pts',(-1.82619257781649,1.51345968459105,20.7406531936883));
#96837=CARTESIAN_POINT('Ctrl Pts',(-1.80679931842709,1.53649261593003,20.73866505213));
#96838=CARTESIAN_POINT('Ctrl Pts',(-1.79924298996926,1.54533426505339,20.7378944597733));
#96839=CARTESIAN_POINT('Ctrl Pts',(-1.78562401180971,1.56103450953162,20.7365125881501));
#96840=CARTESIAN_POINT('Ctrl Pts',(-1.77958606911388,1.56791430571702,20.7359023405736));
#96841=CARTESIAN_POINT('Ctrl Pts',(-1.76671853144158,1.58240584967211,20.7346067804124));
#96842=CARTESIAN_POINT('Ctrl Pts',(-1.75987924614014,1.59000870303565,20.7339210680778));
#96843=CARTESIAN_POINT('Ctrl Pts',(-1.74148193689602,1.61019584987692,20.7320840564289));
#96844=CARTESIAN_POINT('Ctrl Pts',(-1.72983691286378,1.62269967636549,20.7309290738201));
#96845=CARTESIAN_POINT('Ctrl Pts',(-1.67173016327922,1.68375540155034,20.7252027804125));
#96846=CARTESIAN_POINT('Ctrl Pts',(-1.62335880857015,1.73043884528232,20.7205489395811));
#96847=CARTESIAN_POINT('Ctrl Pts',(-1.45060856863031,1.88353672878001,20.7042874639698));
#96848=CARTESIAN_POINT('Ctrl Pts',(-1.31725079592528,1.97909402131459,20.6922926552741));
#96849=CARTESIAN_POINT('Ctrl Pts',(-1.07793968154945,2.11560094712487,20.6722069828031));
#96850=CARTESIAN_POINT('Ctrl Pts',(-0.976919177969611,2.16410640602832,
20.6641171364737));
#96851=CARTESIAN_POINT('Ctrl Pts',(-0.861075649258256,2.20995630069271,
20.6555209075231));
#96852=CARTESIAN_POINT('Ctrl Pts',(-0.849274572321439,2.21451819665596,
20.6546528650766));
#96853=CARTESIAN_POINT('Ctrl Pts',(-0.831404539800097,2.22126228314383,
20.6533505452796));
#96854=CARTESIAN_POINT('Ctrl Pts',(-0.825362496542031,2.22351442341369,
20.6529122984383));
#96855=CARTESIAN_POINT('Ctrl Pts',(-0.81451341350607,2.22750804715898,20.6521292040489));
#96856=CARTESIAN_POINT('Ctrl Pts',(-0.809709878643328,2.22925864694746,
20.6517838256317));
#96857=CARTESIAN_POINT('Ctrl Pts',(-0.799201015227734,2.23305004713406,
20.6510311691658));
#96858=CARTESIAN_POINT('Ctrl Pts',(-0.793493521826344,2.23508451935296,
20.6506242672763));
#96859=CARTESIAN_POINT('Ctrl Pts',(-0.777222111719395,2.24081438339896,
20.6494693979082));
#96860=CARTESIAN_POINT('Ctrl Pts',(-0.766639571371292,2.2444569703462,20.6487244741959));
#96861=CARTESIAN_POINT('Ctrl Pts',(-0.695987644065285,2.26821786440349,
20.6437896873907));
#96862=CARTESIAN_POINT('Ctrl Pts',(-0.635152638383065,2.28599953161763,
20.6397252639053));
#96863=CARTESIAN_POINT('Ctrl Pts',(-0.37141131917774,2.35174476863999,20.6225982372617));
#96864=CARTESIAN_POINT('Ctrl Pts',(-0.163381961725513,2.37528247478567,
20.6102413128642));
#96865=CARTESIAN_POINT('Ctrl Pts',(0.11672035919401,2.36996032203786,20.5925869933682));
#96866=CARTESIAN_POINT('Ctrl Pts',(0.188278919168975,2.36535093343878,20.5879969017559));
#96867=CARTESIAN_POINT('Ctrl Pts',(0.277378099973835,2.35554291938324,20.5821281350748));
#96868=CARTESIAN_POINT('Ctrl Pts',(0.295218844093893,2.35337350626273,20.5809453477241));
#96869=CARTESIAN_POINT('Ctrl Pts',(0.323465733506921,2.3496124695966,20.5790597551683));
#96870=CARTESIAN_POINT('Ctrl Pts',(0.3338891467691,2.34815392800814,20.578361155657));
#96871=CARTESIAN_POINT('Ctrl Pts',(0.352419489143528,2.34543511363328,20.5771140876956));
#96872=CARTESIAN_POINT('Ctrl Pts',(0.36053028958553,2.34420205527712,20.5765664899889));
#96873=CARTESIAN_POINT('Ctrl Pts',(0.379291805892951,2.34125013179166,20.575295674811));
#96874=CARTESIAN_POINT('Ctrl Pts',(0.389937448119666,2.339500637635,20.5745714957796));
#96875=CARTESIAN_POINT('Ctrl Pts',(0.41996260869426,2.3343557055748,20.5725200644883));
#96876=CARTESIAN_POINT('Ctrl Pts',(0.439311957437699,2.3307917358935,20.5711874907284));
#96877=CARTESIAN_POINT('Ctrl Pts',(0.571773642710384,2.30468553098584,20.5619901144981));
#96878=CARTESIAN_POINT('Ctrl Pts',(0.683137386115929,2.2741627751318,20.5538703865256));
#96879=CARTESIAN_POINT('Ctrl Pts',(0.905400110717562,2.19544210067263,20.5368944548262));
#96880=CARTESIAN_POINT('Ctrl Pts',(1.01574079824913,2.14662140507074,20.5280453296828));
#96881=CARTESIAN_POINT('Ctrl Pts',(1.21195892616301,2.04127533204025,20.5118360253846));
#96882=CARTESIAN_POINT('Ctrl Pts',(1.29882140538037,1.98713803687843,20.5044731720221));
#96883=CARTESIAN_POINT('Ctrl Pts',(1.39218300474642,1.92020409852209,20.4965473446824));
#96884=CARTESIAN_POINT('Ctrl Pts',(1.40238000334442,1.91276962610964,20.4956815754885));
#96885=CARTESIAN_POINT('Ctrl Pts',(1.41769162355744,1.90141789464161,20.4943819857503));
#96886=CARTESIAN_POINT('Ctrl Pts',(1.42285021956747,1.89756075126635,20.4939442197611));
#96887=CARTESIAN_POINT('Ctrl Pts',(1.43207484402695,1.8906046223241,20.4931616351831));
#96888=CARTESIAN_POINT('Ctrl Pts',(1.43614660729585,1.8875134756641,20.4928162888128));
#96889=CARTESIAN_POINT('Ctrl Pts',(1.44502702284024,1.88072638798975,20.4920632948543));
#96890=CARTESIAN_POINT('Ctrl Pts',(1.44983149845559,1.87702516536037,20.491656025981));
#96891=CARTESIAN_POINT('Ctrl Pts',(1.46348184788285,1.86642566852043,20.4904990632767));
#96892=CARTESIAN_POINT('Ctrl Pts',(1.47229320199399,1.85948289450991,20.4897524306007));
#96893=CARTESIAN_POINT('Ctrl Pts',(1.53100774530896,1.81254064043229,20.484775983401));
#96894=CARTESIAN_POINT('Ctrl Pts',(1.57932980252574,1.77059519894959,20.4806740538275));
#96895=CARTESIAN_POINT('Ctrl Pts',(1.7825895915519,1.57920576902224,20.4630891451906));
#96896=CARTESIAN_POINT('Ctrl Pts',(1.91847068255332,1.41102724016807,20.4503510646682));
#96897=CARTESIAN_POINT('Ctrl Pts',(2.06353987079851,1.17100553976515,20.4326163050924));
#96898=CARTESIAN_POINT('Ctrl Pts',(2.09495308212083,1.11383173663211,20.4284291288387));
#96899=CARTESIAN_POINT('Ctrl Pts',(2.1318374261876,1.03960564498066,20.4229994969871));
#96900=CARTESIAN_POINT('Ctrl Pts',(2.1395284123607,1.0236839616395,20.4218352670797));
#96901=CARTESIAN_POINT('Ctrl Pts',(2.15144089151315,0.998302270361539,20.4199792806134));
#96902=CARTESIAN_POINT('Ctrl Pts',(2.15577977170574,0.988897822215872,20.4192915960795));
#96903=CARTESIAN_POINT('Ctrl Pts',(2.16345130160985,0.971979469540694,20.4180543250497));
#96904=CARTESIAN_POINT('Ctrl Pts',(2.16680677065702,0.964476043945466,20.417505534867));
#96905=CARTESIAN_POINT('Ctrl Pts',(2.17455904611944,0.946895922492694,20.4162195496063));
#96906=CARTESIAN_POINT('Ctrl Pts',(2.17892489492178,0.936805864786943,20.4154813094975));
#96907=CARTESIAN_POINT('Ctrl Pts',(2.1912878093185,0.907679528996994,20.413349628599));
#96908=CARTESIAN_POINT('Ctrl Pts',(2.19910647662195,0.88856910139725,20.4119501835738));
#96909=CARTESIAN_POINT('Ctrl Pts',(2.26481621799933,0.721779644783481,20.399726110056));
#96910=CARTESIAN_POINT('Ctrl Pts',(2.30799520922596,0.568768999435616,20.3884016590865));
#96911=CARTESIAN_POINT('Ctrl Pts',(2.36525079026029,0.244685088851014,20.3644364943913));
#96912=CARTESIAN_POINT('Ctrl Pts',(2.37672272697818,0.0740247741490599,
20.3518315184729));
#96913=CARTESIAN_POINT('Ctrl Pts',(2.36908472454218,-0.113740156497965,
20.3387835171047));
#96914=CARTESIAN_POINT('Ctrl Pts',(2.36818900036583,-0.131073102270997,
20.3375871595422));
#96915=CARTESIAN_POINT('Ctrl Pts',(2.36668273439652,-0.155100057815818,
20.3359414593089));
#96916=CARTESIAN_POINT('Ctrl Pts',(2.36623391596791,-0.16180312401547,20.3354837121452));
#96917=CARTESIAN_POINT('Ctrl Pts',(2.3654131937711,-0.173325850829405,20.3346992974161));
#96918=CARTESIAN_POINT('Ctrl Pts',(2.36505502871858,-0.17814640059247,20.3343718782056));
#96919=CARTESIAN_POINT('Ctrl Pts',(2.36427513419983,-0.188225890041623,
20.333688862687));
#96920=CARTESIAN_POINT('Ctrl Pts',(2.36385059213733,-0.193484559306545,
20.3333334362796));
#96921=CARTESIAN_POINT('Ctrl Pts',(2.36277258846945,-0.206304021010512,
20.3324691292034));
#96922=CARTESIAN_POINT('Ctrl Pts',(2.36210037067516,-0.213863266508053,
20.3319612915524));
#96923=CARTESIAN_POINT('Ctrl Pts',(2.35956311497801,-0.24092258496678,20.3301495121948));
#96924=CARTESIAN_POINT('Ctrl Pts',(2.35749273268513,-0.260403269760521,
20.3288565057438));
#96925=CARTESIAN_POINT('Ctrl Pts',(2.35175534908219,-0.308687161605983,
20.3256748958064));
#96926=CARTESIAN_POINT('Ctrl Pts',(2.34780029798639,-0.337453569321867,
20.3237998958705));
#96927=CARTESIAN_POINT('Ctrl Pts',(2.3112031329413,-0.571676667139665,20.3086480735083));
#96928=CARTESIAN_POINT('Ctrl Pts',(2.25218535280696,-0.772109749905612,
20.2963329124854));
#96929=CARTESIAN_POINT('Ctrl Pts',(2.13063902886255,-1.0459197527264,20.2776323969683));
#96930=CARTESIAN_POINT('Ctrl Pts',(2.08870920028371,-1.12732499737327,20.2718191207217));
#96931=CARTESIAN_POINT('Ctrl Pts',(2.03325350200847,-1.22122348757576,20.2646890642057));
#96932=CARTESIAN_POINT('Ctrl Pts',(2.0241534182703,-1.2362481635703,20.2635347699027));
#96933=CARTESIAN_POINT('Ctrl Pts',(2.00889847146728,-1.26081476942052,20.2616244223404));
#96934=CARTESIAN_POINT('Ctrl Pts',(2.00284037568124,-1.27041622052866,20.2608719248443));
#96935=CARTESIAN_POINT('Ctrl Pts',(1.99178793756484,-1.28765763323158,20.2595098310332));
#96936=CARTESIAN_POINT('Ctrl Pts',(1.98681795296427,-1.29531300712061,20.2589011495377));
#96937=CARTESIAN_POINT('Ctrl Pts',(1.97608881722333,-1.31163229529747,20.2575951225793));
#96938=CARTESIAN_POINT('Ctrl Pts',(1.97031661808154,-1.32028735892578,20.2568972956639));
#96939=CARTESIAN_POINT('Ctrl Pts',(1.95446228495629,-1.34372444840439,20.2549933638179));
#96940=CARTESIAN_POINT('Ctrl Pts',(1.94426968524244,-1.35843055653313,20.25378309262));
#96941=CARTESIAN_POINT('Ctrl Pts',(1.88851668075994,-1.43695922447999,20.247234351778));
#96942=CARTESIAN_POINT('Ctrl Pts',(1.83998356905705,-1.49860103601939,20.2417819080904));
#96943=CARTESIAN_POINT('Ctrl Pts',(1.66668429209244,-1.69757401982479,20.2230829528693));
#96944=CARTESIAN_POINT('Ctrl Pts',(1.52889849982726,-1.8226488896822,20.2093639836792));
#96945=CARTESIAN_POINT('Ctrl Pts',(1.35750560841799,-1.94499602308788,20.1941397102244));
#96946=CARTESIAN_POINT('Ctrl Pts',(1.336797225773,-1.95928666939635,20.1923287640153));
#96947=CARTESIAN_POINT('Ctrl Pts',(1.27035869997588,-2.00359140540216,20.1866165934868));
#96948=CARTESIAN_POINT('Ctrl Pts',(1.22381204774047,-2.03235698783164,20.1827585995803));
#96949=CARTESIAN_POINT('Ctrl Pts',(1.16744848050704,-2.06454988057956,20.1782898329272));
#96950=CARTESIAN_POINT('Ctrl Pts',(1.15855601276231,-2.06955312537316,20.1775906349952));
#96951=CARTESIAN_POINT('Ctrl Pts',(1.14399242168159,-2.07762387457363,20.176455361126));
#96952=CARTESIAN_POINT('Ctrl Pts',(1.13834070442529,-2.08072585128843,20.17601719062));
#96953=CARTESIAN_POINT('Ctrl Pts',(1.12818450280728,-2.08624637277283,20.1752341772116));
#96954=CARTESIAN_POINT('Ctrl Pts',(1.12368480130221,-2.08867342330638,20.1748888039305));
#96955=CARTESIAN_POINT('Ctrl Pts',(1.11383423901974,-2.09394557579926,20.17413609411));
#96956=CARTESIAN_POINT('Ctrl Pts',(1.1084803173339,-2.09678472299646,20.1737291341348));
#96957=CARTESIAN_POINT('Ctrl Pts',(1.09320453468374,-2.10481050200625,20.1725739335356));
#96958=CARTESIAN_POINT('Ctrl Pts',(1.0832565831071,-2.10994753288132,20.1718287394263));
#96959=CARTESIAN_POINT('Ctrl Pts',(1.01669624306915,-2.14372384502187,20.1668873993031));
#96960=CARTESIAN_POINT('Ctrl Pts',(0.958984929635194,-2.17015500306125,
20.1628170759069));
#96961=CARTESIAN_POINT('Ctrl Pts',(0.706475735500689,-2.2737572008258,20.1456202483129));
#96962=CARTESIAN_POINT('Ctrl Pts',(0.50299071127396,-2.32724963424059,20.133205352057));
#96963=CARTESIAN_POINT('Ctrl Pts',(0.224954368997793,-2.36211628032176,
20.1155380103127));
#96964=CARTESIAN_POINT('Ctrl Pts',(0.154442925865272,-2.36777187445222,
20.1110080427819));
#96965=CARTESIAN_POINT('Ctrl Pts',(0.0659145624144746,-2.37090135402565,
20.1052077250694));
#96966=CARTESIAN_POINT('Ctrl Pts',(0.0480338915409297,-2.37133099254882,
20.104030536922));
#96967=CARTESIAN_POINT('Ctrl Pts',(0.0196461015713497,-2.37169189668111,
20.1021518827972));
#96968=CARTESIAN_POINT('Ctrl Pts',(0.00914110871235234,-2.37175564849506,
20.1014545696869));
#96969=CARTESIAN_POINT('Ctrl Pts',(-0.0104810265275968,-2.37174436524865,
20.1001479721044));
#96970=CARTESIAN_POINT('Ctrl Pts',(-0.01959801657848,-2.37168655174857,
20.0995392389858));
#96971=CARTESIAN_POINT('Ctrl Pts',(-0.0399263932461271,-2.3714404218185,
20.0981781430179));
#96972=CARTESIAN_POINT('Ctrl Pts',(-0.0511371737527683,-2.37122516287566,
20.0974249493329));
#96973=CARTESIAN_POINT('Ctrl Pts',(-0.0840421049860365,-2.37035989682129,
20.095206465772));
#96974=CARTESIAN_POINT('Ctrl Pts',(-0.105728859911678,-2.36949160566055,
20.0937343889457));
#96975=CARTESIAN_POINT('Ctrl Pts',(-0.307051995570714,-2.35866177259903,
20.0799725003353));
#96976=CARTESIAN_POINT('Ctrl Pts',(-0.484983840982608,-2.32858995708623,
20.0670287493638));
#96977=CARTESIAN_POINT('Ctrl Pts',(-0.797578245764926,-2.23835703353013,
20.0432718636491));
#96978=CARTESIAN_POINT('Ctrl Pts',(-0.933389327795246,-2.18521523082703,
20.0325932447577));
#96979=CARTESIAN_POINT('Ctrl Pts',(-1.08029044275168,-2.11152178335929,
20.0211633130528));
#96980=CARTESIAN_POINT('Ctrl Pts',(-1.09699861610564,-2.10288986265206,
20.019865500233));
#96981=CARTESIAN_POINT('Ctrl Pts',(-1.1203878652371,-2.09045166099273,20.0180536680637));
#96982=CARTESIAN_POINT('Ctrl Pts',(-1.12715527504981,-2.08681051023429,
20.0175300244356));
#96983=CARTESIAN_POINT('Ctrl Pts',(-1.13850898893608,-2.08063039049961,
20.0166526498844));
#96984=CARTESIAN_POINT('Ctrl Pts',(-1.14310474561318,-2.07810901595188,
20.0162978239329));
#96985=CARTESIAN_POINT('Ctrl Pts',(-1.15237068977889,-2.07298539231441,
20.0155831248039));
#96986=CARTESIAN_POINT('Ctrl Pts',(-1.1570404929592,-2.07038255946035,20.015223291175));
#96987=CARTESIAN_POINT('Ctrl Pts',(-1.1688137279455,-2.06376817532079,20.0143168989306));
#96988=CARTESIAN_POINT('Ctrl Pts',(-1.17590540991095,-2.05973568303437,
20.013771666033));
#96989=CARTESIAN_POINT('Ctrl Pts',(-1.19131162786577,-2.05086985319753,
20.01258847824));
#96990=CARTESIAN_POINT('Ctrl Pts',(-1.19961789868764,-2.04602234937336,
20.0119513903899));
#96991=CARTESIAN_POINT('Ctrl Pts',(-1.22357324515061,-2.03184607732286,
20.0101157392803));
#96992=CARTESIAN_POINT('Ctrl Pts',(-1.23914498680597,-2.02238713301143,
20.0089246404658));
#96993=CARTESIAN_POINT('Ctrl Pts',(-1.29307089353859,-1.98877350686875,
20.0048016369158));
#96994=CARTESIAN_POINT('Ctrl Pts',(-1.33084242878452,-1.96369838785343,
20.0019169766822));
#96995=CARTESIAN_POINT('Ctrl Pts',(-1.4612361776655,-1.87164303417996,19.9918841940544));
#96996=CARTESIAN_POINT('Ctrl Pts',(-1.54971705749849,-1.79906609074472,
19.9849333703448));
#96997=CARTESIAN_POINT('Ctrl Pts',(-1.74642457542066,-1.61239349936576,
19.9682992231747));
#96998=CARTESIAN_POINT('Ctrl Pts',(-1.84921241213584,-1.49339044585526,
19.958584140688));
#96999=CARTESIAN_POINT('Ctrl Pts',(-1.9502762685528,-1.3498042216479,19.9471185908959));
#97000=CARTESIAN_POINT('Ctrl Pts',(-1.96087599576264,-1.334359118298,19.9458888207482));
#97001=CARTESIAN_POINT('Ctrl Pts',(-1.9778007370199,-1.30906048384905,19.9438792900351));
#97002=CARTESIAN_POINT('Ctrl Pts',(-1.98423782947643,-1.29928262263194,
19.943103757135));
#97003=CARTESIAN_POINT('Ctrl Pts',(-1.99558339030224,-1.28176789620188,
19.9417163963934));
#97004=CARTESIAN_POINT('Ctrl Pts',(-2.00051994371233,-1.27404943316137,
19.9411056321996));
#97005=CARTESIAN_POINT('Ctrl Pts',(-2.01084849603477,-1.25769236519591,
19.939812499231));
#97006=CARTESIAN_POINT('Ctrl Pts',(-2.01622981576902,-1.24904727046751,
19.9391297512506));
#97007=CARTESIAN_POINT('Ctrl Pts',(-2.0303882163845,-1.22597186790908,19.9373090679843));
#97008=CARTESIAN_POINT('Ctrl Pts',(-2.03906697404138,-1.21148222426534,
19.9361675634791));
#97009=CARTESIAN_POINT('Ctrl Pts',(-2.08027738414806,-1.14098182861809,
19.9306208137242));
#97010=CARTESIAN_POINT('Ctrl Pts',(-2.11065723825525,-1.08375188078543,
19.9261391719099));
#97011=CARTESIAN_POINT('Ctrl Pts',(-2.2412729061114,-0.81131763799426,19.9048835935862));
#97012=CARTESIAN_POINT('Ctrl Pts',(-2.31115947940311,-0.583138513754106,
19.8871247096919));
#97013=CARTESIAN_POINT('Ctrl Pts',(-2.35169250939148,-0.31021276020117,
19.8675049846224));
#97014=CARTESIAN_POINT('Ctrl Pts',(-2.35643240577609,-0.271875588474613,
19.8647896616793));
#97015=CARTESIAN_POINT('Ctrl Pts',(-2.36166248848164,-0.218995348799627,
19.8611147194343));
#97016=CARTESIAN_POINT('Ctrl Pts',(-2.36295832113581,-0.20454014620526,
19.8601173638172));
#97017=CARTESIAN_POINT('Ctrl Pts',(-2.36465478774715,-0.183439609711855,
19.8586728946492));
#97018=CARTESIAN_POINT('Ctrl Pts',(-2.36516023135868,-0.17680338903282,
19.8582202431059));
#97019=CARTESIAN_POINT('Ctrl Pts',(-2.36599573028966,-0.165188265492498,
19.85743095722));
#97020=CARTESIAN_POINT('Ctrl Pts',(-2.3663380164592,-0.160210338443474,
19.8570936487721));
#97021=CARTESIAN_POINT('Ctrl Pts',(-2.36697882313379,-0.150440561584785,
19.8564335459404));
#97022=CARTESIAN_POINT('Ctrl Pts',(-2.36727850320949,-0.145648896402515,
19.8561106840891));
#97023=CARTESIAN_POINT('Ctrl Pts',(-2.36790409929548,-0.135133651120503,
19.8554040571721));
#97024=CARTESIAN_POINT('Ctrl Pts',(-2.36822381866285,-0.129409711999625,
19.8550206345085));
#97025=CARTESIAN_POINT('Ctrl Pts',(-2.3689612473943,-0.115288173676648,
19.8540775939886));
#97026=CARTESIAN_POINT('Ctrl Pts',(-2.369355066575,-0.106889327244002,19.8535192466475));
#97027=CARTESIAN_POINT('Ctrl Pts',(-2.37105288670264,-0.0660385161150878,
19.8508150476696));
#97028=CARTESIAN_POINT('Ctrl Pts',(-2.37173494361115,-0.033562651862194,
19.848700587004));
#97029=CARTESIAN_POINT('Ctrl Pts',(-2.37174975346702,-0.0010814014724484,
19.8466119453452));
#97030=CARTESIAN_POINT('Ctrl Pts',(-2.37174975209625,-0.00108440369412818,
19.8466121383971));
#97031=CARTESIAN_POINT('Ctrl Pts',(-2.3717763463339,0.0570810902993918,
19.8428719200797));
#97032=CARTESIAN_POINT('Ctrl Pts',(-2.36966322473608,0.115173800467578,
19.8392200188351));
#97033=CARTESIAN_POINT('Ctrl Pts',(-2.3654264700169,0.173077085263747,19.8356128877059));
#97034=CARTESIAN_POINT('',(-2.37174882624039,-0.00199382054561831,19.6502626448933));
#97035=CARTESIAN_POINT('Ctrl Pts',(-2.36542650053005,0.173076668243166,
19.6378399312857));
#97036=CARTESIAN_POINT('Ctrl Pts',(-2.36968866610404,0.114825954841437,
19.6419243157527));
#97037=CARTESIAN_POINT('Ctrl Pts',(-2.37179834147902,0.0564287005146955,
19.646069626348));
#97038=CARTESIAN_POINT('Ctrl Pts',(-2.37174915967572,-0.00199651634874111,
19.6502622558783));
#97039=CARTESIAN_POINT('Ctrl Pts',(-2.3717491619083,-0.00199386240332,19.6502620654296));
#97040=CARTESIAN_POINT('Ctrl Pts',(-2.37157024597321,-0.214818838888831,
19.6655345118503));
#97041=CARTESIAN_POINT('Ctrl Pts',(-2.34274834294621,-0.42664617522283,
19.6814441245475));
#97042=CARTESIAN_POINT('Ctrl Pts',(-2.27897125142913,-0.657415288275099,
19.6982202130785));
#97043=CARTESIAN_POINT('Ctrl Pts',(-2.27145876365937,-0.682920245629553,
19.700064711527));
#97044=CARTESIAN_POINT('Ctrl Pts',(-2.26094848674177,-0.716508247645402,
19.7024761970154));
#97045=CARTESIAN_POINT('Ctrl Pts',(-2.25833362045104,-0.724707798489459,
19.7030634928898));
#97046=CARTESIAN_POINT('Ctrl Pts',(-2.25396140539591,-0.738164457410525,
19.7040248194749));
#97047=CARTESIAN_POINT('Ctrl Pts',(-2.25223018619591,-0.743429871076609,
19.7044003391736));
#97048=CARTESIAN_POINT('Ctrl Pts',(-2.24880291172266,-0.753731894933052,
19.7051337494477));
#97049=CARTESIAN_POINT('Ctrl Pts',(-2.24710836549643,-0.758768937049329,
19.7054917205684));
#97050=CARTESIAN_POINT('Ctrl Pts',(-2.24289145036374,-0.77116569612999,
19.7063712964613));
#97051=CARTESIAN_POINT('Ctrl Pts',(-2.24034974256688,-0.77851886571668,
19.7068917715871));
#97052=CARTESIAN_POINT('Ctrl Pts',(-2.23147938372618,-0.803777628514846,
19.7086757827665));
#97053=CARTESIAN_POINT('Ctrl Pts',(-2.22497168537623,-0.82162021142403,
19.7099292899358));
#97054=CARTESIAN_POINT('Ctrl Pts',(-2.16803549896793,-0.972086260010119,
19.7204586171915));
#97055=CARTESIAN_POINT('Ctrl Pts',(-2.10600646113119,-1.10003544548114,
19.7291482806169));
#97056=CARTESIAN_POINT('Ctrl Pts',(-1.98923896046088,-1.29433813444706,
19.7430412670856));
#97057=CARTESIAN_POINT('Ctrl Pts',(-1.94171517372129,-1.36459677578765,
19.7482265955425));
#97058=CARTESIAN_POINT('Ctrl Pts',(-1.8496851272839,-1.48608187577362,19.7577048312356));
#97059=CARTESIAN_POINT('Ctrl Pts',(-1.80655057654368,-1.53822896025964,
19.7619615526537));
#97060=CARTESIAN_POINT('Ctrl Pts',(-1.74189580169375,-1.60991679148301,
19.7681536546521));
#97061=CARTESIAN_POINT('Ctrl Pts',(-1.72215289817705,-1.63101880514636,
19.7700213476072));
#97062=CARTESIAN_POINT('Ctrl Pts',(-1.68646510480953,-1.66779285865292,
19.7733617853692));
#97063=CARTESIAN_POINT('Ctrl Pts',(-1.67067470383039,-1.68361027173912,
19.7748279824724));
#97064=CARTESIAN_POINT('Ctrl Pts',(-1.64648225985331,-1.70716860182,19.7770582042093));
#97065=CARTESIAN_POINT('Ctrl Pts',(-1.63824365054816,-1.71507615013399,
19.7778149414612));
#97066=CARTESIAN_POINT('Ctrl Pts',(-1.62983804483503,-1.7230281579756,19.7785843577324));
#97067=CARTESIAN_POINT('Ctrl Pts',(-1.6297277015848,-1.72313252660832,19.7785944576605));
#97068=CARTESIAN_POINT('Ctrl Pts',(-1.62950312059339,-1.72334490662582,
19.7786150130485));
#97069=CARTESIAN_POINT('Ctrl Pts',(-1.62938888213956,-1.72345291724976,
19.7786254685406));
#97070=CARTESIAN_POINT('Ctrl Pts',(-1.62915626121533,-1.723672812797,19.7786467577939));
#97071=CARTESIAN_POINT('Ctrl Pts',(-1.62903787795685,-1.72378469688487,
19.7786575915911));
#97072=CARTESIAN_POINT('Ctrl Pts',(-1.62879669677707,-1.72401259032688,
19.7786796621126));
#97073=CARTESIAN_POINT('Ctrl Pts',(-1.62867389798456,-1.72412859875975,
19.7786908988767));
#97074=CARTESIAN_POINT('Ctrl Pts',(-1.62842359172832,-1.72436501331894,
19.778713802114));
#97075=CARTESIAN_POINT('Ctrl Pts',(-1.62829608330105,-1.72448541842551,
19.7787254686311));
#97076=CARTESIAN_POINT('Ctrl Pts',(-1.62209645605825,-1.73033837225139,
19.7792926802221));
#97077=CARTESIAN_POINT('Ctrl Pts',(-1.61599418539465,-1.73603876251197,
19.779849595243));
#97078=CARTESIAN_POINT('Ctrl Pts',(-1.60220846672796,-1.74878092174392,
19.7811047058551));
#97079=CARTESIAN_POINT('Ctrl Pts',(-1.59450849113973,-1.75580447338948,
19.7818036600613));
#97080=CARTESIAN_POINT('Ctrl Pts',(-1.57371699991801,-1.77451992132172,
19.7836855900221));
#97081=CARTESIAN_POINT('Ctrl Pts',(-1.56054178135121,-1.78611742803415,
19.7848724818437));
#97082=CARTESIAN_POINT('Ctrl Pts',(-1.49976134871859,-1.83843361895336,
19.7903234447539));
#97083=CARTESIAN_POINT('Ctrl Pts',(-1.45068720200129,-1.87739916933862,
19.7946579870328));
#97084=CARTESIAN_POINT('Ctrl Pts',(-1.22466864717369,-2.04270431775677,
19.8143484130582));
#97085=CARTESIAN_POINT('Ctrl Pts',(-1.03240154395743,-2.14629325745103,
19.8305104174073));
#97086=CARTESIAN_POINT('Ctrl Pts',(-0.788312453771228,-2.23732580172646,
19.8492283164366));
#97087=CARTESIAN_POINT('Ctrl Pts',(-0.747439717222321,-2.25131019765726,
19.8523016111626));
#97088=CARTESIAN_POINT('Ctrl Pts',(-0.681109336855299,-2.27199894799178,
19.8571688566933));
#97089=CARTESIAN_POINT('Ctrl Pts',(-0.655883468557604,-2.27940917129099,
19.8589924177495));
#97090=CARTESIAN_POINT('Ctrl Pts',(-0.622276294826786,-2.2886772878218,
19.8613809652386));
#97091=CARTESIAN_POINT('Ctrl Pts',(-0.61400182677619,-2.29091101471607,
19.8619657898102));
#97092=CARTESIAN_POINT('Ctrl Pts',(-0.600364010182595,-2.29451340196958,
19.8629241190917));
#97093=CARTESIAN_POINT('Ctrl Pts',(-0.59500774595686,-2.29590820382869,
19.8632990950955));
#97094=CARTESIAN_POINT('Ctrl Pts',(-0.584493682788414,-2.29860686044341,
19.8640323267075));
#97095=CARTESIAN_POINT('Ctrl Pts',(-0.579336312819429,-2.29991212912285,
19.8643906581024));
#97096=CARTESIAN_POINT('Ctrl Pts',(-0.566598663785245,-2.30309031169753,
19.8652724713485));
#97097=CARTESIAN_POINT('Ctrl Pts',(-0.559013355726528,-2.3049431884749,
19.8657948103287));
#97098=CARTESIAN_POINT('Ctrl Pts',(-0.532783196890197,-2.31121337441078,
19.8675919088273));
#97099=CARTESIAN_POINT('Ctrl Pts',(-0.514093456859698,-2.31544232760589,
19.8688564415791));
#97100=CARTESIAN_POINT('Ctrl Pts',(-0.362564046464306,-2.34780381257082,
19.8789954247396));
#97101=CARTESIAN_POINT('Ctrl Pts',(-0.22756450719299,-2.36471144317895,
19.8873347877119));
#97102=CARTESIAN_POINT('Ctrl Pts',(0.0370700351081663,-2.37496686942844,
19.9035705859503));
#97103=CARTESIAN_POINT('Ctrl Pts',(0.166167912273642,-2.36943603931554,
19.9114447013755));
#97104=CARTESIAN_POINT('Ctrl Pts',(0.36117711351004,-2.34506057236381,19.9238642227435));
#97105=CARTESIAN_POINT('Ctrl Pts',(0.427789053874646,-2.33382800857599,
19.9281989334918));
#97106=CARTESIAN_POINT('Ctrl Pts',(0.510717960794892,-2.31617431853829,
19.9337559505278));
#97107=CARTESIAN_POINT('Ctrl Pts',(0.527569133832011,-2.31239423371589,
19.9348934915524));
#97108=CARTESIAN_POINT('Ctrl Pts',(0.55446062538462,-2.3060526464199,19.9367228673396));
#97109=CARTESIAN_POINT('Ctrl Pts',(0.564528263053351,-2.30360874012265,
19.9374109190566));
#97110=CARTESIAN_POINT('Ctrl Pts',(0.583592422531735,-2.29884846080211,
19.9387199882216));
#97111=CARTESIAN_POINT('Ctrl Pts',(0.592592000944862,-2.2965450305942,19.9393405772122));
#97112=CARTESIAN_POINT('Ctrl Pts',(0.613018741624507,-2.29118877059502,
19.9407552317265));
#97113=CARTESIAN_POINT('Ctrl Pts',(0.62443699166633,-2.28810323077901,19.9415503434307));
#97114=CARTESIAN_POINT('Ctrl Pts',(0.653988318800632,-2.27987993963632,
19.9436196637802));
#97115=CARTESIAN_POINT('Ctrl Pts',(0.672083788168037,-2.27461130880577,
19.944898088465));
#97116=CARTESIAN_POINT('Ctrl Pts',(0.839093423625611,-2.22381835273104,
19.9568046770135));
#97117=CARTESIAN_POINT('Ctrl Pts',(0.983219217450222,-2.16395667493931,
19.9679138515918));
#97118=CARTESIAN_POINT('Ctrl Pts',(1.21777542597114,-2.03824011660773,19.9872827240615));
#97119=CARTESIAN_POINT('Ctrl Pts',(1.31137035335171,-1.97932012397947,19.9953994744278));
#97120=CARTESIAN_POINT('Ctrl Pts',(1.4581938113858,-1.87189105104362,20.0085129619603));
#97121=CARTESIAN_POINT('Ctrl Pts',(1.51393849280968,-1.82710092110257,20.013590960981));
#97122=CARTESIAN_POINT('Ctrl Pts',(1.57630593589758,-1.7721717894522,20.0193150920411));
#97123=CARTESIAN_POINT('Ctrl Pts',(1.58497507123793,-1.76442265128377,20.0201117409757));
#97124=CARTESIAN_POINT('Ctrl Pts',(1.59818240755923,-1.75244102637643,20.0213264812243));
#97125=CARTESIAN_POINT('Ctrl Pts',(1.60276141752954,-1.74825410037618,20.0217478309889));
#97126=CARTESIAN_POINT('Ctrl Pts',(1.61113591430251,-1.74053612441792,20.0225187081789));
#97127=CARTESIAN_POINT('Ctrl Pts',(1.61493624558862,-1.7370106097964,20.0228686270573));
#97128=CARTESIAN_POINT('Ctrl Pts',(1.6234606947411,-1.72905043765951,20.0236537635251));
#97129=CARTESIAN_POINT('Ctrl Pts',(1.6281782101814,-1.72460887210978,20.0240884443763));
#97130=CARTESIAN_POINT('Ctrl Pts',(1.6402409499946,-1.7131581264285,20.0252005756559));
#97131=CARTESIAN_POINT('Ctrl Pts',(1.64755956986613,-1.70612092569312,20.02587594176));
#97132=CARTESIAN_POINT('Ctrl Pts',(1.69212893107081,-1.66271112590344,20.029994382324));
#97133=CARTESIAN_POINT('Ctrl Pts',(1.72822208605996,-1.62516398832108,20.0333536445523));
#97134=CARTESIAN_POINT('Ctrl Pts',(1.78255766821713,-1.56478001647894,20.0385080836743));
#97135=CARTESIAN_POINT('Ctrl Pts',(1.8016616277813,-1.54274554940053,20.040340601405));
#97136=CARTESIAN_POINT('Ctrl Pts',(1.94640058823581,-1.36944735245991,20.0544339077607));
#97137=CARTESIAN_POINT('Ctrl Pts',(2.05318893108956,-1.20344539758727,20.0661572551653));
#97138=CARTESIAN_POINT('Ctrl Pts',(2.15743320750219,-0.986226268891222,
20.0813870848865));
#97139=CARTESIAN_POINT('Ctrl Pts',(2.17547525944371,-0.945762828016393,
20.0842161700404));
#97140=CARTESIAN_POINT('Ctrl Pts',(2.20440890858809,-0.875656764595192,
20.0891225334243));
#97141=CARTESIAN_POINT('Ctrl Pts',(2.21586125735014,-0.84625772678302,20.0911813543414));
#97142=CARTESIAN_POINT('Ctrl Pts',(2.23124374411759,-0.804314473095703,
20.0941246538844));
#97143=CARTESIAN_POINT('Ctrl Pts',(2.23566161305553,-0.79195173939036,20.0949929083142));
#97144=CARTESIAN_POINT('Ctrl Pts',(2.24309499112943,-0.770592590154836,
20.0964945255721));
#97145=CARTESIAN_POINT('Ctrl Pts',(2.24615960361072,-0.761613491117937,
20.0971262474087));
#97146=CARTESIAN_POINT('Ctrl Pts',(2.25192125198599,-0.744394986849645,
20.0983386414704));
#97147=CARTESIAN_POINT('Ctrl Pts',(2.25462715309951,-0.736158691209482,
20.0989190093652));
#97148=CARTESIAN_POINT('Ctrl Pts',(2.26086899036562,-0.716802362847696,
20.1002840480392));
#97149=CARTESIAN_POINT('Ctrl Pts',(2.26436811312505,-0.70567078638689,20.1010699138073));
#97150=CARTESIAN_POINT('Ctrl Pts',(2.27614968476158,-0.667200619179409,
20.1037890290716));
#97151=CARTESIAN_POINT('Ctrl Pts',(2.2840200066732,-0.639739430066774,20.1057356087649));
#97152=CARTESIAN_POINT('Ctrl Pts',(2.33724176262188,-0.440518410633928,
20.1199033881569));
#97153=CARTESIAN_POINT('Ctrl Pts',(2.36365571946768,-0.264317348793432,
20.1327433523245));
#97154=CARTESIAN_POINT('Ctrl Pts',(2.37393935773052,0.0162985479320983,
20.1532532163247));
#97155=CARTESIAN_POINT('Ctrl Pts',(2.37098132276801,0.119598232651939,20.1608004580911));
#97156=CARTESIAN_POINT('Ctrl Pts',(2.35840848356111,0.253099708535496,20.170339260319));
#97157=CARTESIAN_POINT('Ctrl Pts',(2.35491622382643,0.283760133985833,20.1725146488013));
#97158=CARTESIAN_POINT('Ctrl Pts',(2.34810159740941,0.33472322850215,20.1760959358623));
#97159=CARTESIAN_POINT('Ctrl Pts',(2.34511173893536,0.355065847022341,20.1775162070948));
#97160=CARTESIAN_POINT('Ctrl Pts',(2.34062296809238,0.383070540873555,20.1794563221296));
#97161=CARTESIAN_POINT('Ctrl Pts',(2.33935031660775,0.390767217915297,20.1799879542716));
#97162=CARTESIAN_POINT('Ctrl Pts',(2.337137206279,0.40375314069712,20.1808821015825));
#97163=CARTESIAN_POINT('Ctrl Pts',(2.33621671836057,0.409045677780673,20.1812457245516));
#97164=CARTESIAN_POINT('Ctrl Pts',(2.33442484523708,0.419145043980085,20.1819380236679));
#97165=CARTESIAN_POINT('Ctrl Pts',(2.33355658329321,0.423952355379567,20.1822668797209));
#97166=CARTESIAN_POINT('Ctrl Pts',(2.33121669153173,0.436682650978163,20.1831360093288));
#97167=CARTESIAN_POINT('Ctrl Pts',(2.32971950818885,0.444600965429108,20.1836748475911));
#97168=CARTESIAN_POINT('Ctrl Pts',(2.32423851386881,0.47280079726762,20.1855880375521));
#97169=CARTESIAN_POINT('Ctrl Pts',(2.32002984352498,0.493038396420186,20.1869503292901));
#97170=CARTESIAN_POINT('Ctrl Pts',(2.25841851529484,0.771018120938335,20.205547222769));
#97171=CARTESIAN_POINT('Ctrl Pts',(2.15862529872752,1.01750198262787,20.2208522071533));
#97172=CARTESIAN_POINT('Ctrl Pts',(1.98527877126335,1.2993539626881,20.2417719577173));
#97173=CARTESIAN_POINT('Ctrl Pts',(1.94793322235289,1.35469826046254,20.2460576299516));
#97174=CARTESIAN_POINT('Ctrl Pts',(1.89808883523727,1.42223517987368,20.251559425109));
#97175=CARTESIAN_POINT('Ctrl Pts',(1.88772103548177,1.43596775714638,20.2526928688641));
#97176=CARTESIAN_POINT('Ctrl Pts',(1.8708814949395,1.45777485837654,20.2545172091411));
#97177=CARTESIAN_POINT('Ctrl Pts',(1.86450460563408,1.46592212467353,20.255204359837));
#97178=CARTESIAN_POINT('Ctrl Pts',(1.85229950074898,1.48130718342552,20.2565127203402));
#97179=CARTESIAN_POINT('Ctrl Pts',(1.84648164104521,1.48855297426195,20.2571335083828));
#97180=CARTESIAN_POINT('Ctrl Pts',(1.83314674959439,1.50496230215366,20.2585500152574));
#97181=CARTESIAN_POINT('Ctrl Pts',(1.82560335630937,1.51410399676119,20.2593467906327));
#97182=CARTESIAN_POINT('Ctrl Pts',(1.80583613011872,1.53769704103044,20.2614233014497));
#97183=CARTESIAN_POINT('Ctrl Pts',(1.79350745971684,1.55205904349492,20.262707301507));
#97184=CARTESIAN_POINT('Ctrl Pts',(1.67840705571719,1.68293979311044,20.2745964962048));
#97185=CARTESIAN_POINT('Ctrl Pts',(1.56461055004067,1.78922140004199,20.2856802486314));
#97186=CARTESIAN_POINT('Ctrl Pts',(1.35229044790468,1.95168138706883,20.3051373627429));
#97187=CARTESIAN_POINT('Ctrl Pts',(1.25860253412578,2.01337279297222,20.3133709755619));
#97188=CARTESIAN_POINT('Ctrl Pts',(1.09971187038921,2.10255942266117,20.3264975827861));
#97189=CARTESIAN_POINT('Ctrl Pts',(1.03701839440196,2.13417836872652,20.3314808547102));
#97190=CARTESIAN_POINT('Ctrl Pts',(0.962448187286882,2.1677236073271,20.3371122926824));
#97191=CARTESIAN_POINT('Ctrl Pts',(0.951852924571789,2.17239687320872,20.3379056388596));
#97192=CARTESIAN_POINT('Ctrl Pts',(0.935537801807546,2.17945072325493,20.339116411483));
#97193=CARTESIAN_POINT('Ctrl Pts',(0.929842320872545,2.18188672809922,20.3395370642063));
#97194=CARTESIAN_POINT('Ctrl Pts',(0.91936265629075,2.18632048116515,20.340307275231));
#97195=CARTESIAN_POINT('Ctrl Pts',(0.914581480845411,2.18832485159819,20.340657220278));
#97196=CARTESIAN_POINT('Ctrl Pts',(0.903799031219766,2.19280357276485,20.3414431725301));
#97197=CARTESIAN_POINT('Ctrl Pts',(0.897794157648528,2.19526896998961,20.3418786377283));
#97198=CARTESIAN_POINT('Ctrl Pts',(0.880100683417117,2.20244856756057,20.3431553793116));
#97199=CARTESIAN_POINT('Ctrl Pts',(0.868384312822484,2.20709438137374,20.343992676773));
#97200=CARTESIAN_POINT('Ctrl Pts',(0.7710684135213,2.2447874859237,20.3508844868521));
#97201=CARTESIAN_POINT('Ctrl Pts',(0.683643107167049,2.27293945758212,20.3566765698928));
#97202=CARTESIAN_POINT('Ctrl Pts',(0.427301384596625,2.33934794636473,20.3731121459505));
#97203=CARTESIAN_POINT('Ctrl Pts',(0.25556560849099,2.3642805980477,20.3834963568574));
#97204=CARTESIAN_POINT('Ctrl Pts',(0.00637389640235237,2.37296892818386,
20.3991811390228));
#97205=CARTESIAN_POINT('Ctrl Pts',(-0.0699722647303788,2.37194522724757,
20.404062511011));
#97206=CARTESIAN_POINT('Ctrl Pts',(-0.16401617465828,2.36613986579056,20.4102335537611));
#97207=CARTESIAN_POINT('Ctrl Pts',(-0.181888095085075,2.36483315725268,
20.4114132549643));
#97208=CARTESIAN_POINT('Ctrl Pts',(-0.210208415970183,2.36243958434211,
20.4132944442971));
#97209=CARTESIAN_POINT('Ctrl Pts',(-0.220667600881361,2.36148558574624,
20.4139917575508));
#97210=CARTESIAN_POINT('Ctrl Pts',(-0.240342362625392,2.35955917054005,
20.4153084425433));
#97211=CARTESIAN_POINT('Ctrl Pts',(-0.24955927623352,2.35860214830596,20.4159273184167));
#97212=CARTESIAN_POINT('Ctrl Pts',(-0.27029748853394,2.35632591307525,20.4173245444541));
#97213=CARTESIAN_POINT('Ctrl Pts',(-0.281815127435365,2.3549761711269,20.4181038424357));
#97214=CARTESIAN_POINT('Ctrl Pts',(-0.311265727558613,2.35130573926824,
20.4201051837135));
#97215=CARTESIAN_POINT('Ctrl Pts',(-0.329182616076211,2.34886436524211,
20.4213309965651));
#97216=CARTESIAN_POINT('Ctrl Pts',(-0.446469897195048,2.33151439157166,
20.4294112379196));
#97217=CARTESIAN_POINT('Ctrl Pts',(-0.544821428572625,2.31051061879522,
20.4364569984638));
#97218=CARTESIAN_POINT('Ctrl Pts',(-0.814036385168842,2.23487113355375,
20.4564871634325));
#97219=CARTESIAN_POINT('Ctrl Pts',(-0.980474737241934,2.16701785997372,
20.4697753173988));
#97220=CARTESIAN_POINT('Ctrl Pts',(-1.19056418310103,2.05216656974204,20.4869449614003));
#97221=CARTESIAN_POINT('Ctrl Pts',(-1.24233316641792,2.02124725077275,20.4912052658111));
#97222=CARTESIAN_POINT('Ctrl Pts',(-1.30223098621361,1.98230096870914,20.4961226529638));
#97223=CARTESIAN_POINT('Ctrl Pts',(-1.31154666811942,1.97614979738926,20.4968870687436));
#97224=CARTESIAN_POINT('Ctrl Pts',(-1.32588983854891,1.96653285618694,20.4980630317081));
#97225=CARTESIAN_POINT('Ctrl Pts',(-1.33094780090554,1.96311316327842,20.4984775292433));
#97226=CARTESIAN_POINT('Ctrl Pts',(-1.34028162276164,1.95674990227554,20.499241989747));
#97227=CARTESIAN_POINT('Ctrl Pts',(-1.34456099803503,1.9538118465842,20.4995922975427));
#97228=CARTESIAN_POINT('Ctrl Pts',(-1.35426213006472,1.9471044518167,20.5003860457769));
#97229=CARTESIAN_POINT('Ctrl Pts',(-1.35967780893578,1.94332650930587,20.5008288948324));
#97230=CARTESIAN_POINT('Ctrl Pts',(-1.37371402847236,1.93344753311428,20.5019761759846));
#97231=CARTESIAN_POINT('Ctrl Pts',(-1.38230983837189,1.92731136984549,20.5026782958483));
#97232=CARTESIAN_POINT('Ctrl Pts',(-1.43943555768982,1.88595308517009,20.5073433275271));
#97233=CARTESIAN_POINT('Ctrl Pts',(-1.48666035210265,1.84895542669313,20.5111946861712));
#97234=CARTESIAN_POINT('Ctrl Pts',(-1.58533791335619,1.76541949579703,20.5193539173349));
#97235=CARTESIAN_POINT('Ctrl Pts',(-1.63625405648837,1.71833523658822,20.5236358174434));
#97236=CARTESIAN_POINT('Ctrl Pts',(-1.77145566899804,1.58184154136373,20.5354399724279));
#97237=CARTESIAN_POINT('Ctrl Pts',(-1.85096499141975,1.48802057772727,20.5429036350827));
#97238=CARTESIAN_POINT('Ctrl Pts',(-1.95735022198074,1.3406904690135,20.5542655098095));
#97239=CARTESIAN_POINT('Ctrl Pts',(-1.99005426526717,1.29164781189407,20.5579930054323));
#97240=CARTESIAN_POINT('Ctrl Pts',(-2.04135038360049,1.2081447202317,20.5642970916508));
#97241=CARTESIAN_POINT('Ctrl Pts',(-2.06097722185571,1.17434988770958,20.5668372652006));
#97242=CARTESIAN_POINT('Ctrl Pts',(-2.08661689510833,1.12757771650778,20.5703458204976));
#97243=CARTESIAN_POINT('Ctrl Pts',(-2.09336122326067,1.11500688237109,20.5712881089498));
#97244=CARTESIAN_POINT('Ctrl Pts',(-2.10450476105194,1.093778797105,20.5728785414911));
#97245=CARTESIAN_POINT('Ctrl Pts',(-2.10896500963325,1.08515387371081,20.5735245135664));
#97246=CARTESIAN_POINT('Ctrl Pts',(-2.11766643368586,1.06807137091467,20.5748036194338));
#97247=CARTESIAN_POINT('Ctrl Pts',(-2.12191021405711,1.05961531544192,20.5754366468689));
#97248=CARTESIAN_POINT('Ctrl Pts',(-2.13114861729148,1.0409290249592,20.5768353093216));
#97249=CARTESIAN_POINT('Ctrl Pts',(-2.13612038152753,1.03068781487539,20.5776017238098));
#97250=CARTESIAN_POINT('Ctrl Pts',(-2.15337433947967,0.994485711985041,
20.5803107456412));
#97251=CARTESIAN_POINT('Ctrl Pts',(-2.16525811169484,0.968338814954784,
20.5822669909664));
#97252=CARTESIAN_POINT('Ctrl Pts',(-2.25034662993263,0.771722757072405,
20.5969811003242));
#97253=CARTESIAN_POINT('Ctrl Pts',(-2.30378432406054,0.593436784887765,
20.6104203007494));
#97254=CARTESIAN_POINT('Ctrl Pts',(-2.34974818616782,0.332069520135731,
20.6298043678859));
#97255=CARTESIAN_POINT('Ctrl Pts',(-2.35959834086284,0.252729769170749,
20.6356362497434));
#97256=CARTESIAN_POINT('Ctrl Pts',(-2.36542650966497,0.173076543396847,
20.6413652673669));
#97257=CARTESIAN_POINT('Origin',(0.,0.,-1.84858989190503));
#97258=CARTESIAN_POINT('',(-2.36542649448459,0.173076750866022,21.8391485779751));
#97259=CARTESIAN_POINT('',(-2.36542651121823,0.173076522168564,21.6404818371561));
#97260=CARTESIAN_POINT('',(-2.36542649454111,0.173076750093529,-1.84858989190503));
#97261=CARTESIAN_POINT('Ctrl Pts',(-2.36542649448459,0.173076750866022,
21.8391485779751));
#97262=CARTESIAN_POINT('Ctrl Pts',(-2.36468712736919,0.183181623734164,
21.8384536730529));
#97263=CARTESIAN_POINT('Ctrl Pts',(-2.36388300950187,0.193281761835121,
21.837756770496));
#97264=CARTESIAN_POINT('Ctrl Pts',(-2.36044576508709,0.233218801663289,
21.8349918553977));
#97265=CARTESIAN_POINT('Ctrl Pts',(-2.35731236789479,0.263008521156516,
21.8329088847253));
#97266=CARTESIAN_POINT('Ctrl Pts',(-2.32574312133706,0.516832612027184,
21.8149835579103));
#97267=CARTESIAN_POINT('Ctrl Pts',(-2.26600391909561,0.735792982116718,
21.7981782907456));
#97268=CARTESIAN_POINT('Ctrl Pts',(-2.15110529057982,1.00097132946833,21.777423661427));
#97269=CARTESIAN_POINT('Ctrl Pts',(-2.1236485197876,1.05797739941211,21.772947313464));
#97270=CARTESIAN_POINT('Ctrl Pts',(-2.08868923669694,1.12369946214713,21.7678233704948));
#97271=CARTESIAN_POINT('Ctrl Pts',(-2.08336570408184,1.13353895576957,21.7670572616316));
#97272=CARTESIAN_POINT('Ctrl Pts',(-2.07505218050508,1.14864842841117,21.7658828249079));
#97273=CARTESIAN_POINT('Ctrl Pts',(-2.0721113740882,1.15394506774771,21.7654715062615));
#97274=CARTESIAN_POINT('Ctrl Pts',(-2.06665135091455,1.16369085067634,21.7647154685142));
#97275=CARTESIAN_POINT('Ctrl Pts',(-2.06413805587836,1.16814309458145,21.7643703948227));
#97276=CARTESIAN_POINT('Ctrl Pts',(-2.05842180800591,1.17819324209875,21.7635921342977));
#97277=CARTESIAN_POINT('Ctrl Pts',(-2.05521041191576,1.18378622252947,21.7631594971263));
#97278=CARTESIAN_POINT('Ctrl Pts',(-2.04562884991697,1.20031699201036,21.7618819662574));
#97279=CARTESIAN_POINT('Ctrl Pts',(-2.03919377030269,1.211217180222,21.7610411204126));
#97280=CARTESIAN_POINT('Ctrl Pts',(-1.97193122046302,1.3230955189846,21.752421134258));
#97281=CARTESIAN_POINT('Ctrl Pts',(-1.90373366457773,1.41947201691655,21.7450792182251));
#97282=CARTESIAN_POINT('Ctrl Pts',(-1.74468269032294,1.61203654189652,21.729705624385));
#97283=CARTESIAN_POINT('Ctrl Pts',(-1.65239815888481,1.70650489198943,21.7217146101116));
#97284=CARTESIAN_POINT('Ctrl Pts',(-1.50769483927149,1.83183131191092,21.7097508455015));
#97285=CARTESIAN_POINT('Ctrl Pts',(-1.46119471909068,1.86913318817856,21.7059825366025));
#97286=CARTESIAN_POINT('Ctrl Pts',(-1.3817869590987,1.9280577899961,21.6996224881377));
#97287=CARTESIAN_POINT('Ctrl Pts',(-1.34965675315427,1.95068408503323,21.6970683611582));
#97288=CARTESIAN_POINT('Ctrl Pts',(-1.30805831461342,1.97845813913366,21.6937781314321));
#97289=CARTESIAN_POINT('Ctrl Pts',(-1.29909562485786,1.98435473488713,21.6930701912888));
#97290=CARTESIAN_POINT('Ctrl Pts',(-1.28280179228545,1.99491682326788,21.6917847443266));
#97291=CARTESIAN_POINT('Ctrl Pts',(-1.27548438889214,1.99960324572541,21.691208026188));
#97292=CARTESIAN_POINT('Ctrl Pts',(-1.26059784638463,2.00902235444399,21.690035793993));
#97293=CARTESIAN_POINT('Ctrl Pts',(-1.25302741631526,2.01375272592525,21.6894402067113));
#97294=CARTESIAN_POINT('Ctrl Pts',(-1.23661769465289,2.02387795468546,21.6881502753306));
#97295=CARTESIAN_POINT('Ctrl Pts',(-1.22776944418407,2.02925786537913,21.6874553971709));
#97296=CARTESIAN_POINT('Ctrl Pts',(-1.20359517971738,2.04374030764256,21.6855585507539));
#97297=CARTESIAN_POINT('Ctrl Pts',(-1.18820158302909,2.05272812848332,21.6843524442027));
#97298=CARTESIAN_POINT('Ctrl Pts',(-1.11046477410924,2.09694873827737,21.6782691685758));
#97299=CARTESIAN_POINT('Ctrl Pts',(-1.04665583652984,2.12951536658619,21.6732981136789));
#97300=CARTESIAN_POINT('Ctrl Pts',(-0.791632461300696,2.24544079790653,
21.6535027198239));
#97301=CARTESIAN_POINT('Ctrl Pts',(-0.591240610592655,2.3063174538201,21.6379999090804));
#97302=CARTESIAN_POINT('Ctrl Pts',(-0.323013246548215,2.35050509894705,
21.6184764021275));
#97303=CARTESIAN_POINT('Ctrl Pts',(-0.260107701516837,2.35829544555292,
21.613991873548));
#97304=CARTESIAN_POINT('Ctrl Pts',(-0.185806635859397,2.36448709258617,
21.6088598331498));
#97305=CARTESIAN_POINT('Ctrl Pts',(-0.174646861916907,2.36533756640409,
21.6080933887107));
#97306=CARTESIAN_POINT('Ctrl Pts',(-0.157436429618534,2.36652668418171,
21.6069185488095));
#97307=CARTESIAN_POINT('Ctrl Pts',(-0.151389983332795,2.36692117556907,
21.6065071593911));
#97308=CARTESIAN_POINT('Ctrl Pts',(-0.140239001274649,2.36760579992453,
21.6057510561521));
#97309=CARTESIAN_POINT('Ctrl Pts',(-0.135135064576743,2.36790259862969,
21.6054059872618));
#97310=CARTESIAN_POINT('Ctrl Pts',(-0.12359180289652,2.3685364056116,21.604627818832));
#97311=CARTESIAN_POINT('Ctrl Pts',(-0.117152047630164,2.36886365979163,
21.6041952683868));
#97312=CARTESIAN_POINT('Ctrl Pts',(-0.0980734690518432,2.3697552007801,
21.6029182324184));
#97313=CARTESIAN_POINT('Ctrl Pts',(-0.0854311269601467,2.37024464076233,
21.6020777901016));
#97314=CARTESIAN_POINT('Ctrl Pts',(0.0396632502390338,2.37408539162219,
21.5938135032376));
#97315=CARTESIAN_POINT('Ctrl Pts',(0.152231820966934,2.36953315482627,21.5867874075629));
#97316=CARTESIAN_POINT('Ctrl Pts',(0.311289197405841,2.35171323335402,21.5769222534212));
#97317=CARTESIAN_POINT('Ctrl Pts',(0.358343429449025,2.34500451835959,21.574012227221));
#97318=CARTESIAN_POINT('Ctrl Pts',(0.57778800212076,2.30695764947052,21.5603663607412));
#97319=CARTESIAN_POINT('Ctrl Pts',(0.746537563479894,2.25799975039015,21.5496052531584));
#97320=CARTESIAN_POINT('Ctrl Pts',(0.928084954148645,2.18273060458787,21.5367789929547));
#97321=CARTESIAN_POINT('Ctrl Pts',(0.947709979687433,2.17428156400196,21.5353760319599));
#97322=CARTESIAN_POINT('Ctrl Pts',(0.977392396780473,2.16102437327209,21.5332276411493));
#97323=CARTESIAN_POINT('Ctrl Pts',(0.98753482649677,2.1564084025092,21.532488786251));
#97324=CARTESIAN_POINT('Ctrl Pts',(1.00591197088979,2.14788785084186,21.5311412002221));
#97325=CARTESIAN_POINT('Ctrl Pts',(1.01415747266829,2.14400693319998,21.5305332956394));
#97326=CARTESIAN_POINT('Ctrl Pts',(1.03190825303541,2.13552684843694,21.5292174341529));
#97327=CARTESIAN_POINT('Ctrl Pts',(1.04140556040252,2.13091154569335,21.5285089260731));
#97328=CARTESIAN_POINT('Ctrl Pts',(1.0671179251063,2.11820344018102,21.5265783866353));
#97329=CARTESIAN_POINT('Ctrl Pts',(1.08327127962135,2.10998810018982,21.525352091696));
#97330=CARTESIAN_POINT('Ctrl Pts',(1.16472122348156,2.06738211916254,21.5190987095369));
#97331=CARTESIAN_POINT('Ctrl Pts',(1.22847483901889,2.03014577377484,21.5139717186042));
#97332=CARTESIAN_POINT('Ctrl Pts',(1.46347324126149,1.87776496753466,21.4941577576237));
#97333=CARTESIAN_POINT('Ctrl Pts',(1.62117283861821,1.74342607558306,21.4788234782505));
#97334=CARTESIAN_POINT('Ctrl Pts',(1.8018167435931,1.54358070660903,21.4594781839303));
#97335=CARTESIAN_POINT('Ctrl Pts',(1.84227489054645,1.4950618167598,21.4550091023024));
#97336=CARTESIAN_POINT('Ctrl Pts',(1.88756475763463,1.43611364358557,21.4498923563373));
#97337=CARTESIAN_POINT('Ctrl Pts',(1.89431505230589,1.42719781621834,21.4491265488468));
#97338=CARTESIAN_POINT('Ctrl Pts',(1.90462424015947,1.41337937452946,21.4479524754598));
#97339=CARTESIAN_POINT('Ctrl Pts',(1.90822771988776,1.4085104627563,21.4475412216012));
#97340=CARTESIAN_POINT('Ctrl Pts',(1.91483834649784,1.39950645215011,21.4467852447925));
#97341=CARTESIAN_POINT('Ctrl Pts',(1.91785076082092,1.39537545592722,21.4464401676852));
#97342=CARTESIAN_POINT('Ctrl Pts',(1.92463361009703,1.38601051123391,21.4456618266865));
#97343=CARTESIAN_POINT('Ctrl Pts',(1.92839606091981,1.38077090970669,21.4452291129645));
#97344=CARTESIAN_POINT('Ctrl Pts',(1.93806118048639,1.36719466830274,21.4441148421737));
#97345=CARTESIAN_POINT('Ctrl Pts',(1.94393152978422,1.35883502206309,21.4434354265726));
#97346=CARTESIAN_POINT('Ctrl Pts',(1.98101635764553,1.30529232875984,21.4391245586984));
#97347=CARTESIAN_POINT('Ctrl Pts',(2.01071044326692,1.25907049023229,21.4355867641089));
#97348=CARTESIAN_POINT('Ctrl Pts',(2.05132915233621,1.19073524402782,21.4305525145929));
#97349=CARTESIAN_POINT('Ctrl Pts',(2.06355434322322,1.16942090406961,21.4290088453607));
#97350=CARTESIAN_POINT('Ctrl Pts',(2.1653413638624,0.985389324429527,21.4158732304707));
#97351=CARTESIAN_POINT('Ctrl Pts',(2.23583413236536,0.812862584864275,21.404780432448));
#97352=CARTESIAN_POINT('Ctrl Pts',(2.30644683703887,0.558263028975817,21.3881775894915));
#97353=CARTESIAN_POINT('Ctrl Pts',(2.32365009509977,0.48166671447982,21.3831626753346));
#97354=CARTESIAN_POINT('Ctrl Pts',(2.34007646536301,0.386730484296695,21.3768526656097));
#97355=CARTESIAN_POINT('Ctrl Pts',(2.34292784425433,0.369062892568961,21.3756745322218));
#97356=CARTESIAN_POINT('Ctrl Pts',(2.34712026530927,0.341075895435963,21.3738014626047));
#97357=CARTESIAN_POINT('Ctrl Pts',(2.34859383879468,0.330776783897866,21.3731107295425));
#97358=CARTESIAN_POINT('Ctrl Pts',(2.35123283219823,0.311425008639067,21.371809990519));
#97359=CARTESIAN_POINT('Ctrl Pts',(2.35241385444851,0.302374636155485,21.3712004903943));
#97360=CARTESIAN_POINT('Ctrl Pts',(2.35494650264956,0.282053006108913,21.36982918303));
#97361=CARTESIAN_POINT('Ctrl Pts',(2.35626949645607,0.270778471935944,21.3690664865753));
#97362=CARTESIAN_POINT('Ctrl Pts',(2.35943297939522,0.242038241441896,21.3671172662907));
#97363=CARTESIAN_POINT('Ctrl Pts',(2.36116047653273,0.224561059887744,21.3659272212151));
#97364=CARTESIAN_POINT('Ctrl Pts',(2.37067359297253,0.116013528040631,21.3585054595592));
#97365=CARTESIAN_POINT('Ctrl Pts',(2.37338241102787,0.0245870486302439,
21.3521162920509));
#97366=CARTESIAN_POINT('Ctrl Pts',(2.36495765184394,-0.274605748820411,
21.3307601788161));
#97367=CARTESIAN_POINT('Ctrl Pts',(2.33180083118807,-0.48075546460797,21.3152503519221));
#97368=CARTESIAN_POINT('Ctrl Pts',(2.26383514195862,-0.707884099840714,
21.29841322483));
#97369=CARTESIAN_POINT('Ctrl Pts',(2.25495470880947,-0.735682594807681,
21.2963590033748));
#97370=CARTESIAN_POINT('Ctrl Pts',(2.23923502575379,-0.78192785902656,21.2929602432573));
#97371=CARTESIAN_POINT('Ctrl Pts',(2.23267542038401,-0.800465619664024,
21.2916029133169));
#97372=CARTESIAN_POINT('Ctrl Pts',(2.22326157143464,-0.826053152008092,
21.2897385322571));
#97373=CARTESIAN_POINT('Ctrl Pts',(2.22060306347414,-0.833173369411592,
21.2892207215183));
#97374=CARTESIAN_POINT('Ctrl Pts',(2.21604044731529,-0.845216335769105,
21.2883467344542));
#97375=CARTESIAN_POINT('Ctrl Pts',(2.21415406458807,-0.85014569263355,21.287989520228));
#97376=CARTESIAN_POINT('Ctrl Pts',(2.21050940150974,-0.859575238204033,
21.2873072445561));
#97377=CARTESIAN_POINT('Ctrl Pts',(2.20875381187642,-0.864076387764508,
21.2869820200075));
#97378=CARTESIAN_POINT('Ctrl Pts',(2.20452764093215,-0.874814808444424,
21.2862071492798));
#97379=CARTESIAN_POINT('Ctrl Pts',(2.20204430847061,-0.881047067414209,
21.285758261366));
#97380=CARTESIAN_POINT('Ctrl Pts',(2.19306432156613,-0.903308406069299,
21.2841575175206));
#97381=CARTESIAN_POINT('Ctrl Pts',(2.18641862734327,-0.919277338028167,
21.2830141954987));
#97382=CARTESIAN_POINT('Ctrl Pts',(2.11213800682284,-1.09240250978723,21.2706580902213));
#97383=CARTESIAN_POINT('Ctrl Pts',(2.02785132646807,-1.24189685649614,21.260316950865));
#97384=CARTESIAN_POINT('Ctrl Pts',(1.83703761445154,-1.50831016763068,21.2402183305204));
#97385=CARTESIAN_POINT('Ctrl Pts',(1.73351629926569,-1.62622819813745,21.2305289606676));
#97386=CARTESIAN_POINT('Ctrl Pts',(1.60336702902551,-1.74782103547055,21.2189073895246));
#97387=CARTESIAN_POINT('Ctrl Pts',(1.5873905488428,-1.76234372258896,21.2174899309549));
#97388=CARTESIAN_POINT('Ctrl Pts',(1.56283648023269,-1.78405868895823,21.2153238683512));
#97389=CARTESIAN_POINT('Ctrl Pts',(1.55440227454752,-1.79141196579194,21.2145820086449));
#97390=CARTESIAN_POINT('Ctrl Pts',(1.53900317157983,-1.80464689012095,21.2132312613664));
#97391=CARTESIAN_POINT('Ctrl Pts',(1.53205575732524,-1.8105486219941,21.2126232198182));
#97392=CARTESIAN_POINT('Ctrl Pts',(1.51701543801442,-1.82317661209782,21.211309688343));
#97393=CARTESIAN_POINT('Ctrl Pts',(1.50891147160832,-1.82988933072939,21.2106036632936));
#97394=CARTESIAN_POINT('Ctrl Pts',(1.48685313168408,-1.8479146416132,21.2086863911297));
#97395=CARTESIAN_POINT('Ctrl Pts',(1.47281470463787,-1.8591227965458,21.2074709778796));
#97396=CARTESIAN_POINT('Ctrl Pts',(1.40222185981162,-1.91418211791575,21.2013815326785));
#97397=CARTESIAN_POINT('Ctrl Pts',(1.34383585122908,-1.9556131121364,21.1964138437282));
#97398=CARTESIAN_POINT('Ctrl Pts',(1.10826754235946,-2.10723851527118,21.1766181611081));
#97399=CARTESIAN_POINT('Ctrl Pts',(0.918740089505553,-2.19649881505852,
21.1611108941741));
#97400=CARTESIAN_POINT('Ctrl Pts',(0.659665629835438,-2.27904667216431,
21.1415826794664));
#97401=CARTESIAN_POINT('Ctrl Pts',(0.598543555017432,-2.29585708124241,
21.1370977485944));
#97402=CARTESIAN_POINT('Ctrl Pts',(0.525914212829848,-2.31273378561264,
21.1319653095695));
#97403=CARTESIAN_POINT('Ctrl Pts',(0.514994632602176,-2.31518981149414,
21.1311988482973));
#97404=CARTESIAN_POINT('Ctrl Pts',(0.498136980785032,-2.31885625370446,
21.1300239879931));
#97405=CARTESIAN_POINT('Ctrl Pts',(0.492211156861529,-2.32012132357915,
21.129612594849));
#97406=CARTESIAN_POINT('Ctrl Pts',(0.481276468004334,-2.32241192785565,
21.1288564879576));
#97407=CARTESIAN_POINT('Ctrl Pts',(0.476269160230746,-2.32344397162374,
21.1285114191165));
#97408=CARTESIAN_POINT('Ctrl Pts',(0.464939079142822,-2.32574101962232,
21.1277332547696));
#97409=CARTESIAN_POINT('Ctrl Pts',(0.458614469081092,-2.32699643508795,
21.1273007083304));
#97410=CARTESIAN_POINT('Ctrl Pts',(0.43986590918429,-2.33063855874844,21.1260236956619));
#97411=CARTESIAN_POINT('Ctrl Pts',(0.427427650561155,-2.33295172060679,
21.1251832724169));
#97412=CARTESIAN_POINT('Ctrl Pts',(0.303710364290955,-2.35493693211906,
21.1168858184041));
#97413=CARTESIAN_POINT('Ctrl Pts',(0.191161880748561,-2.36673455123434,
21.1098301501645));
#97414=CARTESIAN_POINT('Ctrl Pts',(-0.0842443173053113,-2.37581850165966,
21.0928479563442));
#97415=CARTESIAN_POINT('Ctrl Pts',(-0.246787335855732,-2.36446710196096,
21.0830378534763));
#97416=CARTESIAN_POINT('Ctrl Pts',(-0.473100331433842,-2.32505713966609,
21.0685175478187));
#97417=CARTESIAN_POINT('Ctrl Pts',(-0.538783804257595,-2.3107196511006,
21.0642025391191));
#97418=CARTESIAN_POINT('Ctrl Pts',(-0.620289577317182,-2.28926426309865,
21.0586777748752));
#97419=CARTESIAN_POINT('Ctrl Pts',(-0.636765737865761,-2.28473617637862,
21.057552162054));
#97420=CARTESIAN_POINT('Ctrl Pts',(-0.663022232907123,-2.27721412322809,
21.0557436345621));
#97421=CARTESIAN_POINT('Ctrl Pts',(-0.672834830991789,-2.27433417266923,
21.0550644369151));
#97422=CARTESIAN_POINT('Ctrl Pts',(-0.691394652965542,-2.26875633002332,
21.0537733514402));
#97423=CARTESIAN_POINT('Ctrl Pts',(-0.700145505347256,-2.26607107533139,
21.0531618872933));
#97424=CARTESIAN_POINT('Ctrl Pts',(-0.71997939247914,-2.2598590678387,21.0517696929393));
#97425=CARTESIAN_POINT('Ctrl Pts',(-0.731052399843292,-2.25630133456845,
21.0509879566445));
#97426=CARTESIAN_POINT('Ctrl Pts',(-0.759650405468366,-2.24688024200492,
21.0489571090471));
#97427=CARTESIAN_POINT('Ctrl Pts',(-0.777133562078111,-2.24089333823027,
21.0477039537643));
#97428=CARTESIAN_POINT('Ctrl Pts',(-0.90563739323192,-2.19520403470242,
21.0384050868149));
#97429=CARTESIAN_POINT('Ctrl Pts',(-1.01361218477934,-2.14748277048992,
21.0300917884416));
#97430=CARTESIAN_POINT('Ctrl Pts',(-1.29466764483622,-1.99733441905921,
21.0071203372578));
#97431=CARTESIAN_POINT('Ctrl Pts',(-1.45902101127502,-1.88062923851374,
20.9921480015438));
#97432=CARTESIAN_POINT('Ctrl Pts',(-1.62574206293377,-1.72708726458613,
20.9762773333855));
#97433=CARTESIAN_POINT('Ctrl Pts',(-1.64448947476798,-1.70924608585119,
20.9744829018701));
#97434=CARTESIAN_POINT('Ctrl Pts',(-1.66896422388565,-1.6851788678676,20.9721314757504));
#97435=CARTESIAN_POINT('Ctrl Pts',(-1.67495481219333,-1.67922475563294,
20.9715552100378));
#97436=CARTESIAN_POINT('Ctrl Pts',(-1.68476253771582,-1.66937204336446,
20.9706107646022));
#97437=CARTESIAN_POINT('Ctrl Pts',(-1.68859819205367,-1.66549211195983,
20.9702411540135));
#97438=CARTESIAN_POINT('Ctrl Pts',(-1.6960928164822,-1.6578584672812,20.9695185257588));
#97439=CARTESIAN_POINT('Ctrl Pts',(-1.6997527762559,-1.65410581286782,20.9691654335887));
#97440=CARTESIAN_POINT('Ctrl Pts',(-1.7087472918753,-1.64482211915427,20.9682971042078));
#97441=CARTESIAN_POINT('Ctrl Pts',(-1.71406752773735,-1.63927716559819,
20.9677829732597));
#97442=CARTESIAN_POINT('Ctrl Pts',(-1.73231273249455,-1.62007537331697,
20.9660176054774));
#97443=CARTESIAN_POINT('Ctrl Pts',(-1.7451025999597,-1.60629031901468,20.9647762290587));
#97444=CARTESIAN_POINT('Ctrl Pts',(-1.85582319130809,-1.48407086533995,
20.9539798535635));
#97445=CARTESIAN_POINT('Ctrl Pts',(-1.9437178133738,-1.36693803622698,20.9450492864254));
#97446=CARTESIAN_POINT('Ctrl Pts',(-2.08509320472877,-1.13705418035971,
20.9285137168175));
#97447=CARTESIAN_POINT('Ctrl Pts',(-2.141556035136,-1.02676216291712,20.9209404130938));
#97448=CARTESIAN_POINT('Ctrl Pts',(-2.20543298887878,-0.873528956500393,
20.910428351251));
#97449=CARTESIAN_POINT('Ctrl Pts',(-2.22066108025742,-0.834057281210004,
20.9077226876439));
#97450=CARTESIAN_POINT('Ctrl Pts',(-2.24499579089928,-0.76558116238951,
20.9030169534428));
#97451=CARTESIAN_POINT('Ctrl Pts',(-2.25461553340185,-0.73676948642199,
20.9010335023841));
#97452=CARTESIAN_POINT('Ctrl Pts',(-2.26750574033933,-0.695543108657033,
20.8981868038184));
#97453=CARTESIAN_POINT('Ctrl Pts',(-2.27123309547361,-0.683273527652343,
20.8973385213324));
#97454=CARTESIAN_POINT('Ctrl Pts',(-2.27750046492205,-0.662024743991826,
20.8958673381842));
#97455=CARTESIAN_POINT('Ctrl Pts',(-2.28008734843247,-0.653059575094418,
20.8952459815119));
#97456=CARTESIAN_POINT('Ctrl Pts',(-2.28494835572515,-0.635832138523277,
20.8940506494781));
#97457=CARTESIAN_POINT('Ctrl Pts',(-2.28723073930303,-0.627572337309024,
20.8934769540904));
#97458=CARTESIAN_POINT('Ctrl Pts',(-2.29249672779055,-0.608104704444415,
20.8921233391253));
#97459=CARTESIAN_POINT('Ctrl Pts',(-2.29544295997697,-0.596887081154943,
20.8913422211521));
#97460=CARTESIAN_POINT('Ctrl Pts',(-2.30542208102913,-0.557725224820697,
20.8886110197272));
#97461=CARTESIAN_POINT('Ctrl Pts',(-2.31202765169595,-0.529675757463541,
20.8866472759853));
#97462=CARTESIAN_POINT('Ctrl Pts',(-2.35393100300824,-0.335988205452596,
20.8730298617291));
#97463=CARTESIAN_POINT('Ctrl Pts',(-2.37190321514705,-0.167133874586679,
20.8608188306911));
#97464=CARTESIAN_POINT('Ctrl Pts',(-2.37169704770757,0.0592161657391793,
20.8442899294982));
#97465=CARTESIAN_POINT('Ctrl Pts',(-2.369586273947,0.116225454262654,20.8401188173442));
#97466=CARTESIAN_POINT('Ctrl Pts',(-2.3654264754702,0.173077010733998,20.8359749974364));
#97467=CARTESIAN_POINT('Ctrl Pts',(-2.36542650966497,0.173076543396847,
20.6413652673669));
#97468=CARTESIAN_POINT('Ctrl Pts',(-2.3696452004405,0.11541995515753,20.6455121880587));
#97469=CARTESIAN_POINT('Ctrl Pts',(-2.37175659210489,0.0575990783915476,
20.6496045891759));
#97470=CARTESIAN_POINT('Ctrl Pts',(-2.37174851271759,-0.0131612086354773,
20.6544884432378));
#97471=CARTESIAN_POINT('Ctrl Pts',(-2.3716419523089,-0.0260517523897936,
20.6553730834095));
#97472=CARTESIAN_POINT('Ctrl Pts',(-2.37132271330337,-0.045492707167401,
20.6566989915195));
#97473=CARTESIAN_POINT('Ctrl Pts',(-2.37118797917937,-0.0520438954879125,
20.6571443779233));
#97474=CARTESIAN_POINT('Ctrl Pts',(-2.37089793521941,-0.0637805144074743,
20.657939660729));
#97475=CARTESIAN_POINT('Ctrl Pts',(-2.37075276202606,-0.0689660517614046,
20.6582901073936));
#97476=CARTESIAN_POINT('Ctrl Pts',(-2.37039847004216,-0.0802926495732673,
20.6590535383995));
#97477=CARTESIAN_POINT('Ctrl Pts',(-2.37018250124127,-0.0864333809034787,
20.6594661376441));
#97478=CARTESIAN_POINT('Ctrl Pts',(-2.36949986201149,-0.103909434823094,
20.6606368515593));
#97479=CARTESIAN_POINT('Ctrl Pts',(-2.36897571476367,-0.115242537261224,
20.6613918447916));
#97480=CARTESIAN_POINT('Ctrl Pts',(-2.3649381690402,-0.190791822333342,
20.6663993688259));
#97481=CARTESIAN_POINT('Ctrl Pts',(-2.35889506676514,-0.254852587822693,
20.6705229562528));
#97482=CARTESIAN_POINT('Ctrl Pts',(-2.32100559644241,-0.534361006591841,
20.6882847708484));
#97483=CARTESIAN_POINT('Ctrl Pts',(-2.26218565627446,-0.745074381662656,
20.7011681468132));
#97484=CARTESIAN_POINT('Ctrl Pts',(-2.15062384474508,-1.00194545887362,
20.7189065764197));
#97485=CARTESIAN_POINT('Ctrl Pts',(-2.12357249757711,-1.0580720205822,20.7229106064955));
#97486=CARTESIAN_POINT('Ctrl Pts',(-2.08612418841368,-1.12853481350844,
20.7281390534488));
#97487=CARTESIAN_POINT('Ctrl Pts',(-2.07773185831141,-1.14391225728876,
20.7292927252315));
#97488=CARTESIAN_POINT('Ctrl Pts',(-2.06407996086349,-1.16828097766345,
20.7311419260452));
#97489=CARTESIAN_POINT('Ctrl Pts',(-2.05893006619404,-1.17733321716219,
20.7318335240213));
#97490=CARTESIAN_POINT('Ctrl Pts',(-2.04954324217532,-1.19358297260235,
20.733083617031));
#97491=CARTESIAN_POINT('Ctrl Pts',(-2.04532757367536,-1.20079262461028,
20.7336413358725));
#97492=CARTESIAN_POINT('Ctrl Pts',(-2.03532646531623,-1.21769108777459,
20.7349559052645));
#97493=CARTESIAN_POINT('Ctrl Pts',(-2.02950982341799,-1.22736110198178,
20.735713883741));
#97494=CARTESIAN_POINT('Ctrl Pts',(-2.01236812567664,-1.2554036767555,20.7379289626199));
#97495=CARTESIAN_POINT('Ctrl Pts',(-2.00086127924025,-1.27366320207019,
20.7393927066824));
#97496=CARTESIAN_POINT('Ctrl Pts',(-1.90068407350219,-1.42792002352111,
20.7519461498186));
#97497=CARTESIAN_POINT('Ctrl Pts',(-1.79853245359352,-1.55461158586091,
20.7635589884005));
#97498=CARTESIAN_POINT('Ctrl Pts',(-1.56870983101207,-1.78641745387736,
20.7873461045678));
#97499=CARTESIAN_POINT('Ctrl Pts',(-1.44135462155368,-1.89067267068279,
20.7994552010222));
#97500=CARTESIAN_POINT('Ctrl Pts',(-1.28924575722734,-1.99082041667007,
20.8121091302878));
#97501=CARTESIAN_POINT('Ctrl Pts',(-1.27413449596935,-2.00052540323376,
20.8133477085353));
#97502=CARTESIAN_POINT('Ctrl Pts',(-1.25309534420424,-2.0137023753804,20.8150451811488));
#97503=CARTESIAN_POINT('Ctrl Pts',(-1.24726090217526,-2.01732135346785,
20.8155130811788));
#97504=CARTESIAN_POINT('Ctrl Pts',(-1.23722129010457,-2.02348850161555,
20.8163132625005));
#97505=CARTESIAN_POINT('Ctrl Pts',(-1.23302380233644,-2.0260489976463,20.8166463349663));
#97506=CARTESIAN_POINT('Ctrl Pts',(-1.22424844119997,-2.03136465549287,
20.8173395370334));
#97507=CARTESIAN_POINT('Ctrl Pts',(-1.21966918587069,-2.03411742216213,
20.8176994992834));
#97508=CARTESIAN_POINT('Ctrl Pts',(-1.20850857505186,-2.0407752568808,20.8185725957647));
#97509=CARTESIAN_POINT('Ctrl Pts',(-1.20191746855148,-2.04466403791797,
20.8190846792412));
#97510=CARTESIAN_POINT('Ctrl Pts',(-1.17839443154228,-2.05838967932137,
20.8209001228028));
#97511=CARTESIAN_POINT('Ctrl Pts',(-1.16135906852133,-2.06804900427308,
20.8221926059982));
#97512=CARTESIAN_POINT('Ctrl Pts',(-1.11887979282501,-2.09144495780304,
20.8253657839801));
#97513=CARTESIAN_POINT('Ctrl Pts',(-1.09330005787436,-2.10492972531439,
20.8272330944833));
#97514=CARTESIAN_POINT('Ctrl Pts',(-0.88109591951423,-2.21188413214313,
20.8424228264066));
#97515=CARTESIAN_POINT('Ctrl Pts',(-0.683114109363354,-2.28081890118502,
20.8547781147088));
#97516=CARTESIAN_POINT('Ctrl Pts',(-0.390027147579792,-2.34120991195955,
20.873465687652));
#97517=CARTESIAN_POINT('Ctrl Pts',(-0.300444277150448,-2.35438215506194,
20.8792158416831));
#97518=CARTESIAN_POINT('Ctrl Pts',(-0.192728834378511,-2.36397252436587,
20.8862857501647));
#97519=CARTESIAN_POINT('Ctrl Pts',(-0.17510602318451,-2.36534317855025,
20.8874472191432));
#97520=CARTESIAN_POINT('Ctrl Pts',(-0.14602286956667,-2.36727839496821,
20.8893726702298));
#97521=CARTESIAN_POINT('Ctrl Pts',(-0.134570614173728,-2.36795701389958,
20.8901330772944));
#97522=CARTESIAN_POINT('Ctrl Pts',(-0.113870182078115,-2.36903299347542,
20.8915117342182));
#97523=CARTESIAN_POINT('Ctrl Pts',(-0.10462369074526,-2.36945935219341,
20.892129062778));
#97524=CARTESIAN_POINT('Ctrl Pts',(-0.0847955983121818,-2.37025734365144,
20.8934561991348));
#97525=CARTESIAN_POINT('Ctrl Pts',(-0.0742135639136895,-2.37061226463634,
20.894166516994));
#97526=CARTESIAN_POINT('Ctrl Pts',(-0.0453261631996215,-2.37138753908803,
20.8961113290445));
#97527=CARTESIAN_POINT('Ctrl Pts',(-0.0270180601373795,-2.37166677954516,
20.8973502045664));
#97528=CARTESIAN_POINT('Ctrl Pts',(0.0736176830453946,-2.37203631360565,
20.9041961852921));
#97529=CARTESIAN_POINT('Ctrl Pts',(0.155894547547436,-2.36805191886237,
20.9099291446253));
#97530=CARTESIAN_POINT('Ctrl Pts',(0.448260354323311,-2.33859110567113,
20.9307947711502));
#97531=CARTESIAN_POINT('Ctrl Pts',(0.654914652286427,-2.28932643646113,
20.9465618831532));
#97532=CARTESIAN_POINT('Ctrl Pts',(0.898435089325787,-2.19555419551166,
20.965171444833));
#97533=CARTESIAN_POINT('Ctrl Pts',(0.94402342773639,-2.17634198733309,20.968650677293));
#97534=CARTESIAN_POINT('Ctrl Pts',(0.998946105131645,-2.15114502962015,
20.9728091823508));
#97535=CARTESIAN_POINT('Ctrl Pts',(1.00887935094984,-2.14650430383177,20.9735599249432));
#97536=CARTESIAN_POINT('Ctrl Pts',(1.02431521825704,-2.13916197680044,20.9747240191271));
#97537=CARTESIAN_POINT('Ctrl Pts',(1.0298399911156,-2.13650771686113,20.9751401604018));
#97538=CARTESIAN_POINT('Ctrl Pts',(1.0400228023075,-2.13156692529489,20.9759061322126));
#97539=CARTESIAN_POINT('Ctrl Pts',(1.04468360199809,-2.12928653755461,20.9762563188353));
#97540=CARTESIAN_POINT('Ctrl Pts',(1.0552307346398,-2.12408317850289,20.9770478757895));
#97541=CARTESIAN_POINT('Ctrl Pts',(1.06111241955384,-2.12115102909511,20.9774886684539));
#97542=CARTESIAN_POINT('Ctrl Pts',(1.07896600048825,-2.1121577808734,20.9788250014417));
#97543=CARTESIAN_POINT('Ctrl Pts',(1.09089897173506,-2.10601936738839,20.9797158822237));
#97544=CARTESIAN_POINT('Ctrl Pts',(1.11844141151013,-2.09155440360074,20.9817682760086));
#97545=CARTESIAN_POINT('Ctrl Pts',(1.13401129003754,-2.08315372704289,20.9829256104635));
#97546=CARTESIAN_POINT('Ctrl Pts',(1.18727400993353,-2.05364183420262,20.986879794979));
#97547=CARTESIAN_POINT('Ctrl Pts',(1.22448509815896,-2.03167444999079,20.9896337950729));
#97548=CARTESIAN_POINT('Ctrl Pts',(1.44534283158833,-1.89301834351864,21.0060551261749));
#97549=CARTESIAN_POINT('Ctrl Pts',(1.61281711628574,-1.75253142672316,21.0189288848144));
#97550=CARTESIAN_POINT('Ctrl Pts',(1.80069029088014,-1.54486623879113,21.0366648561276));
#97551=CARTESIAN_POINT('Ctrl Pts',(1.84073424094568,-1.4969280527704,21.0406787183646));
#97552=CARTESIAN_POINT('Ctrl Pts',(1.88953829609246,-1.43357961271023,21.0459183491342));
#97553=CARTESIAN_POINT('Ctrl Pts',(1.90008418972768,-1.41957230280426,21.0470729903874));
#97554=CARTESIAN_POINT('Ctrl Pts',(1.91664703559409,-1.39705788601958,21.0489233826871));
#97555=CARTESIAN_POINT('Ctrl Pts',(1.92276504495133,-1.38862564139934,21.0496151937078));
#97556=CARTESIAN_POINT('Ctrl Pts',(1.93368691997316,-1.37336182459283,21.050865464682));
#97557=CARTESIAN_POINT('Ctrl Pts',(1.93851066049169,-1.36654462854578,21.0514231469281));
#97558=CARTESIAN_POINT('Ctrl Pts',(1.94976489629137,-1.35045997626401,21.0527373563463));
#97559=CARTESIAN_POINT('Ctrl Pts',(1.95616543479715,-1.34117190634214,21.0534950094901));
#97560=CARTESIAN_POINT('Ctrl Pts',(1.97460591897388,-1.31399936692707,21.0557081961122));
#97561=CARTESIAN_POINT('Ctrl Pts',(1.98646829077914,-1.2959963532558,21.0571703558814));
#97562=CARTESIAN_POINT('Ctrl Pts',(2.09089826377963,-1.13270466061889,21.0703990697946));
#97563=CARTESIAN_POINT('Ctrl Pts',(2.167606231319,-0.977924221130729,21.0827603247273));
#97564=CARTESIAN_POINT('Ctrl Pts',(2.27969697486948,-0.672117107464571,
21.1065238119082));
#97565=CARTESIAN_POINT('Ctrl Pts',(2.31841202263608,-0.523195624988745,
21.1178138206501));
#97566=CARTESIAN_POINT('Ctrl Pts',(2.34536531780108,-0.353274135405132,
21.1297753641064));
#97567=CARTESIAN_POINT('Ctrl Pts',(2.34805262375522,-0.334947784231481,
21.1310533285733));
#97568=CARTESIAN_POINT('Ctrl Pts',(2.35145144164751,-0.309713323131881,
21.1327947063899));
#97569=CARTESIAN_POINT('Ctrl Pts',(2.35234763376866,-0.302831368788849,
21.1332677481744));
#97570=CARTESIAN_POINT('Ctrl Pts',(2.35382959894123,-0.291047506660982,
21.1340744226826));
#97571=CARTESIAN_POINT('Ctrl Pts',(2.35443029190172,-0.28614757330336,21.1344088745463));
#97572=CARTESIAN_POINT('Ctrl Pts',(2.35564736421591,-0.275956398973795,
21.135102406473));
#97573=CARTESIAN_POINT('Ctrl Pts',(2.35626122041093,-0.270664922967461,
21.1354613312695));
#97574=CARTESIAN_POINT('Ctrl Pts',(2.35770402871674,-0.257850831249838,
21.1363277759289));
#97575=CARTESIAN_POINT('Ctrl Pts',(2.35851482188043,-0.250326141538377,
21.136834283689));
#97576=CARTESIAN_POINT('Ctrl Pts',(2.3612388165966,-0.223856797556103,21.1386083852662));
#97577=CARTESIAN_POINT('Ctrl Pts',(2.36295995288263,-0.204892491303803,
21.1398657465504));
#97578=CARTESIAN_POINT('Ctrl Pts',(2.3666362029517,-0.158136661947514,21.1429365403592));
#97579=CARTESIAN_POINT('Ctrl Pts',(2.36833045979948,-0.130326901984869,
21.1447376784462));
#97580=CARTESIAN_POINT('Ctrl Pts',(2.37760100822646,0.0839999240548525,
21.1584683102904));
#97581=CARTESIAN_POINT('Ctrl Pts',(2.36362421554544,0.270809630366736,21.1696041734351));
#97582=CARTESIAN_POINT('Ctrl Pts',(2.30630342376191,0.564680969256217,21.1881462629775));
#97583=CARTESIAN_POINT('Ctrl Pts',(2.27687258857723,0.673606879778546,21.1952469049075));
#97584=CARTESIAN_POINT('Ctrl Pts',(2.23373210864795,0.797484129998888,21.203814806863));
#97585=CARTESIAN_POINT('Ctrl Pts',(2.22744607681222,0.81487668628204,21.2050291609565));
#97586=CARTESIAN_POINT('Ctrl Pts',(2.216844708056,0.843169609951421,21.2070241726166));
#97587=CARTESIAN_POINT('Ctrl Pts',(2.21265073162711,0.854114853081182,21.2078007880634));
#97588=CARTESIAN_POINT('Ctrl Pts',(2.20499183407692,0.873667649917114,21.2091970483341));
#97589=CARTESIAN_POINT('Ctrl Pts',(2.2015571838178,0.882286865498201,21.2098156657354));
#97590=CARTESIAN_POINT('Ctrl Pts',(2.19415687556208,0.900545563355231,21.2111328798036));
#97591=CARTESIAN_POINT('Ctrl Pts',(2.19017808066226,0.910179474181156,21.2118319100923));
#97592=CARTESIAN_POINT('Ctrl Pts',(2.17932704549678,0.935970060086562,21.2137142600443));
#97593=CARTESIAN_POINT('Ctrl Pts',(2.17233879851819,0.952076908717332,21.2149014988092));
#97594=CARTESIAN_POINT('Ctrl Pts',(2.13608856483242,1.03315082705193,21.2209380053448));
#97595=CARTESIAN_POINT('Ctrl Pts',(2.10409118424908,1.09684703299919,21.2258803285694));
#97596=CARTESIAN_POINT('Ctrl Pts',(1.99609897720886,1.28965611120571,21.2414843083434));
#97597=CARTESIAN_POINT('Ctrl Pts',(1.91071657903993,1.41307334109011,21.252436384304));
#97598=CARTESIAN_POINT('Ctrl Pts',(1.80496131492765,1.53867548534734,21.264418347522));
#97599=CARTESIAN_POINT('Ctrl Pts',(1.79553678556956,1.54966294839946,21.2654738977897));
#97600=CARTESIAN_POINT('Ctrl Pts',(1.71627096695985,1.64038000044255,21.2742474841337));
#97601=CARTESIAN_POINT('Ctrl Pts',(1.64124847199267,1.71544210806391,21.2818925338484));
#97602=CARTESIAN_POINT('Ctrl Pts',(1.55183822849854,1.79364408996817,21.2900895254204));
#97603=CARTESIAN_POINT('Ctrl Pts',(1.54216188838417,1.80197051506445,21.2909654446803));
#97604=CARTESIAN_POINT('Ctrl Pts',(1.52743779261396,1.81443501888759,21.2922808821841));
#97605=CARTESIAN_POINT('Ctrl Pts',(1.52243960168572,1.81863088885225,21.2927244254997));
#97606=CARTESIAN_POINT('Ctrl Pts',(1.5134383539737,1.82612412125847,21.2935177553389));
#97607=CARTESIAN_POINT('Ctrl Pts',(1.50944176038794,1.82942901780323,21.2938680801313));
#97608=CARTESIAN_POINT('Ctrl Pts',(1.50066973026009,1.83663454186072,21.2946328093154));
#97609=CARTESIAN_POINT('Ctrl Pts',(1.49588991818402,1.84052966141355,21.2950468186593));
#97610=CARTESIAN_POINT('Ctrl Pts',(1.48219464625476,1.85160149075079,21.2962255844801));
#97611=CARTESIAN_POINT('Ctrl Pts',(1.47324220181304,1.85873249228641,21.2969871515889));
#97612=CARTESIAN_POINT('Ctrl Pts',(1.41175610405579,1.90698544825356,21.3021594392204));
#97613=CARTESIAN_POINT('Ctrl Pts',(1.35755378371209,1.94594409293718,21.3064312754567));
#97614=CARTESIAN_POINT('Ctrl Pts',(1.089027520532,2.12226120962693,21.3266302084878));
#97615=CARTESIAN_POINT('Ctrl Pts',(0.855190424216477,2.22679966279556,21.3415830952711));
#97616=CARTESIAN_POINT('Ctrl Pts',(0.578722595261967,2.30027655249391,21.3600797859028));
#97617=CARTESIAN_POINT('Ctrl Pts',(0.548095414337796,2.30776587287932,21.3621361185582));
#97618=CARTESIAN_POINT('Ctrl Pts',(0.505460803794458,2.31729483088571,21.3650127179139));
#97619=CARTESIAN_POINT('Ctrl Pts',(0.493572383321684,2.31985608402364,21.3658163383191));
#97620=CARTESIAN_POINT('Ctrl Pts',(0.473054137302115,2.3241116973564,21.367206120419));
#97621=CARTESIAN_POINT('Ctrl Pts',(0.464433534357405,2.32584971294576,21.3677908797526));
#97622=CARTESIAN_POINT('Ctrl Pts',(0.446581686602045,2.32934565147967,21.369003675859));
#97623=CARTESIAN_POINT('Ctrl Pts',(0.437349275352296,2.33109673197665,21.3696319190955));
#97624=CARTESIAN_POINT('Ctrl Pts',(0.415712591092952,2.3350674282499,21.3711067547596));
#97625=CARTESIAN_POINT('Ctrl Pts',(0.403300649788364,2.3372431255799,21.3719547262087));
#97626=CARTESIAN_POINT('Ctrl Pts',(0.362805276837944,2.34400941477819,21.3747279435138));
#97627=CARTESIAN_POINT('Ctrl Pts',(0.33465738406256,2.34819337315646,21.3766659500521));
#97628=CARTESIAN_POINT('Ctrl Pts',(0.184345764931605,2.36777855768801,21.3870745291786));
#97629=CARTESIAN_POINT('Ctrl Pts',(0.0612154670472332,2.37415305845575,
21.3958240202191));
#97630=CARTESIAN_POINT('Ctrl Pts',(-0.111553816657242,2.3696470897217,21.4083459363374));
#97631=CARTESIAN_POINT('Ctrl Pts',(-0.16121722612389,2.36678693061316,21.4119718441474));
#97632=CARTESIAN_POINT('Ctrl Pts',(-0.35160722406399,2.34980175411044,21.4259301487461));
#97633=CARTESIAN_POINT('Ctrl Pts',(-0.491069034400797,2.32466230383876,
21.4362940625826));
#97634=CARTESIAN_POINT('Ctrl Pts',(-0.645797912876436,2.28221477861414,
21.4474551150239));
#97635=CARTESIAN_POINT('Ctrl Pts',(-0.664065076890717,2.27696659421323,
21.4487669659708));
#97636=CARTESIAN_POINT('Ctrl Pts',(-0.689721124159214,2.26926053938407,
21.4505993489995));
#97637=CARTESIAN_POINT('Ctrl Pts',(-0.697163425399591,2.26698517580838,
21.4511296803836));
#97638=CARTESIAN_POINT('Ctrl Pts',(-0.70966936518123,2.26309427589203,21.4520186523635));
#97639=CARTESIAN_POINT('Ctrl Pts',(-0.714738969277246,2.26149829034101,
21.4523784119759));
#97640=CARTESIAN_POINT('Ctrl Pts',(-0.725083850661469,2.25820330918063,
21.453111224038));
#97641=CARTESIAN_POINT('Ctrl Pts',(-0.730358602131399,2.25650284511101,
21.4534841881488));
#97642=CARTESIAN_POINT('Ctrl Pts',(-0.743806376482816,2.25211548385002,
21.4544334006122));
#97643=CARTESIAN_POINT('Ctrl Pts',(-0.751970918170312,2.24940254784854,
21.455008140662));
#97644=CARTESIAN_POINT('Ctrl Pts',(-0.784589988457899,2.23836634604835,
21.4572987982288));
#97645=CARTESIAN_POINT('Ctrl Pts',(-0.808923671612739,2.2296878658109,21.4589950968454));
#97646=CARTESIAN_POINT('Ctrl Pts',(-1.02135635090556,2.1499890663138,21.4737337164913));
#97647=CARTESIAN_POINT('Ctrl Pts',(-1.19988225430784,2.05570618049798,21.4856895851367));
#97648=CARTESIAN_POINT('Ctrl Pts',(-1.46000987859554,1.87276143993761,21.5053579807119));
#97649=CARTESIAN_POINT('Ctrl Pts',(-1.55051696540666,1.79854270958477,21.5127110460673));
#97650=CARTESIAN_POINT('Ctrl Pts',(-1.64866421063376,1.70512494015636,21.5215601578593));
#97651=CARTESIAN_POINT('Ctrl Pts',(-1.66199902562371,1.692130003073,21.5227826478116));
#97652=CARTESIAN_POINT('Ctrl Pts',(-1.6835036541298,1.67067405267722,21.5247883460952));
#97653=CARTESIAN_POINT('Ctrl Pts',(-1.69176613996554,1.66230672951337,21.5255674381987));
#97654=CARTESIAN_POINT('Ctrl Pts',(-1.70643871200612,1.64722528691826,21.52696642653));
#97655=CARTESIAN_POINT('Ctrl Pts',(-1.71287229353528,1.64053428050837,21.5275852791132));
#97656=CARTESIAN_POINT('Ctrl Pts',(-1.72643065326025,1.62626671440785,21.5289011618166));
#97657=CARTESIAN_POINT('Ctrl Pts',(-1.73354518531059,1.61868073177298,21.5295986146523));
#97658=CARTESIAN_POINT('Ctrl Pts',(-1.75167199125929,1.59909616036568,21.5313937829524));
#97659=CARTESIAN_POINT('Ctrl Pts',(-1.76261083762612,1.58703065724405,21.5324945796743));
#97660=CARTESIAN_POINT('Ctrl Pts',(-1.81438669085634,1.52872647525026,21.5377904706223));
#97661=CARTESIAN_POINT('Ctrl Pts',(-1.85353017782231,1.48102274075293,21.5420546422733));
#97662=CARTESIAN_POINT('Ctrl Pts',(-1.96079502784208,1.33937895031534,21.5545343906508));
#97663=CARTESIAN_POINT('Ctrl Pts',(-2.0239369689956,1.241904399001,21.5629146522692));
#97664=CARTESIAN_POINT('Ctrl Pts',(-2.15499440917576,1.00286257298039,21.5827983924731));
#97665=CARTESIAN_POINT('Ctrl Pts',(-2.21651301019787,0.858377939139675,
21.5943298494037));
#97666=CARTESIAN_POINT('Ctrl Pts',(-2.26881328028884,0.691389883826201,
21.6064931701347));
#97667=CARTESIAN_POINT('Ctrl Pts',(-2.2740861633845,0.673844081010464,21.6077570459858));
#97668=CARTESIAN_POINT('Ctrl Pts',(-2.28106826297322,0.64959482498718,21.6094827235657));
#97669=CARTESIAN_POINT('Ctrl Pts',(-2.28295208999073,0.642942932797866,
21.6099539288732));
#97670=CARTESIAN_POINT('Ctrl Pts',(-2.28612928575771,0.631534045628689,
21.6107582828366));
#97671=CARTESIAN_POINT('Ctrl Pts',(-2.28743694512057,0.626781130241172,
21.6110922406155));
#97672=CARTESIAN_POINT('Ctrl Pts',(-2.2901283108459,0.616878284436149,21.611785643129));
#97673=CARTESIAN_POINT('Ctrl Pts',(-2.291509477117,0.611727729402215,21.6121449283164));
#97674=CARTESIAN_POINT('Ctrl Pts',(-2.29481638174934,0.599227470959713,
21.6130137024167));
#97675=CARTESIAN_POINT('Ctrl Pts',(-2.29672421985806,0.59187300143213,21.613522165707));
#97676=CARTESIAN_POINT('Ctrl Pts',(-2.3007227584584,0.576148655046813,21.6146038382331));
#97677=CARTESIAN_POINT('Ctrl Pts',(-2.30280320806519,0.567776253862717,
21.6151764832947));
#97678=CARTESIAN_POINT('Ctrl Pts',(-2.31151018542596,0.531901316625478,
21.6176168919629));
#97679=CARTESIAN_POINT('Ctrl Pts',(-2.31769036539249,0.504291469635803,
21.6194616419155));
#97680=CARTESIAN_POINT('Ctrl Pts',(-2.34393021934912,0.376368534512657,
21.6278830901827));
#97681=CARTESIAN_POINT('Ctrl Pts',(-2.35796962568734,0.274989332207001,
21.6342053888481));
#97682=CARTESIAN_POINT('Ctrl Pts',(-2.36542651121823,0.173076522168559,
21.6404818371561));
#97683=CARTESIAN_POINT('Origin',(0.,0.,-1.84858989190503));
#97684=CARTESIAN_POINT('',(-2.36542647205564,0.173077057400502,22.8373161962119));
#97685=CARTESIAN_POINT('',(-2.36542649454112,0.173076750093424,22.6375488994376));
#97686=CARTESIAN_POINT('',(-2.36542649454111,0.173076750093529,-1.84858989190503));
#97687=CARTESIAN_POINT('',(-2.37174999975095,-3.43714120204603E-5,21.8508342761113));
#97688=CARTESIAN_POINT('Ctrl Pts',(-2.36542647205563,0.173077057400639,
22.8373161962119));
#97689=CARTESIAN_POINT('Ctrl Pts',(-2.35558699271399,0.307552216936542,
22.8290336145396));
#97690=CARTESIAN_POINT('Ctrl Pts',(-2.33429152119662,0.441040438584974,
22.8206514246345));
#97691=CARTESIAN_POINT('Ctrl Pts',(-2.29496692921169,0.599256497923799,
22.8100741087363));
#97692=CARTESIAN_POINT('Ctrl Pts',(-2.28773509460163,0.626298319391269,
22.8082437799283));
#97693=CARTESIAN_POINT('Ctrl Pts',(-2.27694933891818,0.663946245068075,
22.8056612080991));
#97694=CARTESIAN_POINT('Ctrl Pts',(-2.27379623434611,0.674665536243362,
22.8049219575777));
#97695=CARTESIAN_POINT('Ctrl Pts',(-2.26787604431434,0.694278808476925,
22.8035619283539));
#97696=CARTESIAN_POINT('Ctrl Pts',(-2.26513206928857,0.70317957927455,22.8029419144976));
#97697=CARTESIAN_POINT('Ctrl Pts',(-2.25945757425223,0.721208318025415,
22.8016802306059));
#97698=CARTESIAN_POINT('Ctrl Pts',(-2.25652399827277,0.730335134288215,
22.8010384700706));
#97699=CARTESIAN_POINT('Ctrl Pts',(-2.24912857528644,0.752873488223653,
22.7994459761405));
#97700=CARTESIAN_POINT('Ctrl Pts',(-2.24460206797607,0.766263256834902,
22.7984931247612));
#97701=CARTESIAN_POINT('Ctrl Pts',(-2.22713477775099,0.81644974683606,22.7948956662897));
#97702=CARTESIAN_POINT('Ctrl Pts',(-2.21340722534166,0.852964036057281,
22.7922251760598));
#97703=CARTESIAN_POINT('Ctrl Pts',(-2.17666804699988,0.943819568435279,
22.7854416365893));
#97704=CARTESIAN_POINT('Ctrl Pts',(-2.15251820409061,0.997669059529739,
22.7812929824227));
#97705=CARTESIAN_POINT('Ctrl Pts',(-2.07201206217199,1.1606178629502,22.7683453512165));
#97706=CARTESIAN_POINT('Ctrl Pts',(-2.00917770111188,1.26628117659205,22.7593750808445));
#97707=CARTESIAN_POINT('Ctrl Pts',(-1.89825471466519,1.42362031733921,22.7453172574431));
#97708=CARTESIAN_POINT('Ctrl Pts',(-1.85555564309847,1.47884409746286,22.7402344746356));
#97709=CARTESIAN_POINT('Ctrl Pts',(-1.77168369245427,1.57795511168974,22.7309207641472));
#97710=CARTESIAN_POINT('Ctrl Pts',(-1.73115354122448,1.62231756327132,22.7266732180056));
#97711=CARTESIAN_POINT('Ctrl Pts',(-1.68162793909208,1.67255348792312,22.7218143507961));
#97712=CARTESIAN_POINT('Ctrl Pts',(-1.67422755887628,1.67996124560529,22.7210965650793));
#97713=CARTESIAN_POINT('Ctrl Pts',(-1.66213391704839,1.69190765733032,22.7199372403654));
#97714=CARTESIAN_POINT('Ctrl Pts',(-1.65747064748957,1.6964762699333,22.7194934610599));
#97715=CARTESIAN_POINT('Ctrl Pts',(-1.64911763937748,1.70459240613741,22.718704426452));
#97716=CARTESIAN_POINT('Ctrl Pts',(-1.64543523197978,1.70814728834145,22.7183586049754));
#97717=CARTESIAN_POINT('Ctrl Pts',(-1.63741204944231,1.71584259941598,22.7176095261008));
#97718=CARTESIAN_POINT('Ctrl Pts',(-1.63306707023926,1.71997848584083,22.7172066166591));
#97719=CARTESIAN_POINT('Ctrl Pts',(-1.62077612658569,1.73158939169322,22.7160744572582));
#97720=CARTESIAN_POINT('Ctrl Pts',(-1.61279408389704,1.73902625866763,22.7153480652338));
#97721=CARTESIAN_POINT('Ctrl Pts',(-1.56258377561651,1.78516412404157,22.7108316097686));
#97722=CARTESIAN_POINT('Ctrl Pts',(-1.51901245084755,1.82238344986652,22.7071438034318));
#97723=CARTESIAN_POINT('Ctrl Pts',(-1.4094963585779,1.90927359956167,22.6982998598725));
#97724=CARTESIAN_POINT('Ctrl Pts',(-1.34222459859286,1.95715111485792,22.6932171694765));
#97725=CARTESIAN_POINT('Ctrl Pts',(-1.11425013608458,2.10210672777954,22.6766430167731));
#97726=CARTESIAN_POINT('Ctrl Pts',(-0.944543093247345,2.18362885398592,
22.6652379419402));
#97727=CARTESIAN_POINT('Ctrl Pts',(-0.740621758548927,2.25332093868393,
22.6512619433395));
#97728=CARTESIAN_POINT('Ctrl Pts',(-0.714075617626403,2.26187350378313,
22.6494391119012));
#97729=CARTESIAN_POINT('Ctrl Pts',(-0.676420285763294,2.27327625387389,
22.6468458191595));
#97730=CARTESIAN_POINT('Ctrl Pts',(-0.665431093368501,2.27651724825956,
22.6460880995843));
#97731=CARTESIAN_POINT('Ctrl Pts',(-0.646215722718315,2.28203333490999,
22.6447614043192));
#97732=CARTESIAN_POINT('Ctrl Pts',(-0.637999877120554,2.28434390043603,
22.6441935927472));
#97733=CARTESIAN_POINT('Ctrl Pts',(-0.620746864045961,2.28909567769971,
22.6429999432978));
#97734=CARTESIAN_POINT('Ctrl Pts',(-0.611707374740382,2.2915278253219,22.6423738225227));
#97735=CARTESIAN_POINT('Ctrl Pts',(-0.590090430321594,2.29720701722337,
22.6408746796482));
#97736=CARTESIAN_POINT('Ctrl Pts',(-0.57750034500473,2.30040434179363,22.6400000669896));
#97737=CARTESIAN_POINT('Ctrl Pts',(-0.534407804666629,2.31097188849553,
22.6370010486823));
#97738=CARTESIAN_POINT('Ctrl Pts',(-0.503786787611022,2.31783983026575,
22.6348606371386));
#97739=CARTESIAN_POINT('Ctrl Pts',(-0.429785016831794,2.33290192351682,
22.6296630101178));
#97740=CARTESIAN_POINT('Ctrl Pts',(-0.386295519493603,2.34049607573808,
22.6265879437685));
#97741=CARTESIAN_POINT('Ctrl Pts',(-0.0971590420607199,2.38270735080721,
22.6060066556091));
#97742=CARTESIAN_POINT('Ctrl Pts',(0.152350240948549,2.37980882727667,22.5873753595239));
#97743=CARTESIAN_POINT('Ctrl Pts',(0.4300275982135,2.3326822994552,22.5675108026101));
#97744=CARTESIAN_POINT('Ctrl Pts',(0.463082687731045,2.326345881876,22.5651643152334));
#97745=CARTESIAN_POINT('Ctrl Pts',(0.505442078512209,2.31728714684873,22.562190204124));
#97746=CARTESIAN_POINT('Ctrl Pts',(0.51487815816828,2.31520882558411,22.5615298004521));
#97747=CARTESIAN_POINT('Ctrl Pts',(0.529884866660682,2.31180727278781,22.5604831830983));
#97748=CARTESIAN_POINT('Ctrl Pts',(0.535463731421846,2.31052146333716,22.5600949022876));
#97749=CARTESIAN_POINT('Ctrl Pts',(0.546072755444561,2.30803582054928,22.559358139311));
#97750=CARTESIAN_POINT('Ctrl Pts',(0.551103589105282,2.30683975120977,22.5590094634566));
#97751=CARTESIAN_POINT('Ctrl Pts',(0.562923237103904,2.30398878379735,22.5581918517174));
#97752=CARTESIAN_POINT('Ctrl Pts',(0.569708702060304,2.30232032625334,22.5577236981664));
#97753=CARTESIAN_POINT('Ctrl Pts',(0.591947468725474,2.2967477653618,22.5561930852083));
#97754=CARTESIAN_POINT('Ctrl Pts',(0.607369211444168,2.29271777127163,22.5551375672198));
#97755=CARTESIAN_POINT('Ctrl Pts',(0.644121114734362,2.28271693628169,22.5526336856405));
#97756=CARTESIAN_POINT('Ctrl Pts',(0.66541091189813,2.27660207741005,22.5511925801612));
#97757=CARTESIAN_POINT('Ctrl Pts',(0.744663886734401,2.25263222773845,22.5458522046485));
#97758=CARTESIAN_POINT('Ctrl Pts',(0.802024664869938,2.23285328398392,22.5420355862054));
#97759=CARTESIAN_POINT('Ctrl Pts',(1.05832617816016,2.13332245266067,22.5249436467309));
#97760=CARTESIAN_POINT('Ctrl Pts',(1.24664005681874,2.02904140806073,22.5121792189246));
#97761=CARTESIAN_POINT('Ctrl Pts',(1.45399992596791,1.87431487606233,22.4956071657126));
#97762=CARTESIAN_POINT('Ctrl Pts',(1.48885312322667,1.84675066100328,22.4927280640453));
#97763=CARTESIAN_POINT('Ctrl Pts',(1.53468669184813,1.80836136024325,22.4888011560118));
#97764=CARTESIAN_POINT('Ctrl Pts',(1.54636706648699,1.7983834208659,22.4877876376396));
#97765=CARTESIAN_POINT('Ctrl Pts',(1.56537471926271,1.78182407411574,22.4861167247011));
#97766=CARTESIAN_POINT('Ctrl Pts',(1.5727595178514,1.77530913837813,22.4854620923861));
#97767=CARTESIAN_POINT('Ctrl Pts',(1.58701347531288,1.76257543013912,22.4841877667408));
#97768=CARTESIAN_POINT('Ctrl Pts',(1.59388719573426,1.75636201302964,22.4835683055141));
#97769=CARTESIAN_POINT('Ctrl Pts',(1.60990487013122,1.74171156191803,22.4821130413663));
#97770=CARTESIAN_POINT('Ctrl Pts',(1.61901912209831,1.73324260499905,22.4812758878397));
#97771=CARTESIAN_POINT('Ctrl Pts',(1.64853913227364,1.70537662186464,22.4785342396491));
#97772=CARTESIAN_POINT('Ctrl Pts',(1.66866555270957,1.6856885379369,22.476617224451));
#97773=CARTESIAN_POINT('Ctrl Pts',(1.77399912010252,1.57891385698854,22.4663210974556));
#97774=CARTESIAN_POINT('Ctrl Pts',(1.85273845465151,1.48573002426072,22.4576685100779));
#97775=CARTESIAN_POINT('Ctrl Pts',(2.00770207900375,1.27076213515345,22.4384757527063));
#97776=CARTESIAN_POINT('Ctrl Pts',(2.08074637188678,1.14725680127547,22.427904910793));
#97777=CARTESIAN_POINT('Ctrl Pts',(2.16855310511449,0.962467910526155,22.4132183864481));
#97778=CARTESIAN_POINT('Ctrl Pts',(2.19274144681989,0.906009656431272,22.4088737109581));
#97779=CARTESIAN_POINT('Ctrl Pts',(2.21849728124602,0.838796577063157,22.4039151222576));
#97780=CARTESIAN_POINT('Ctrl Pts',(2.22221514221361,0.828896710543056,22.4031901058899));
#97781=CARTESIAN_POINT('Ctrl Pts',(2.22813159768663,0.812816502391584,22.4020214760737));
#97782=CARTESIAN_POINT('Ctrl Pts',(2.23037093462263,0.806651461163442,22.4015755638971));
#97783=CARTESIAN_POINT('Ctrl Pts',(2.23431286400689,0.795657154061061,22.4007842464348));
#97784=CARTESIAN_POINT('Ctrl Pts',(2.23602541830358,0.790831594938553,22.4004382612361));
#97785=CARTESIAN_POINT('Ctrl Pts',(2.23970269751516,0.780362477826645,22.3996905463802));
#97786=CARTESIAN_POINT('Ctrl Pts',(2.24166172466497,0.774717034943749,22.3992891540903));
#97787=CARTESIAN_POINT('Ctrl Pts',(2.24710241347357,0.758844853203738,22.3981655556702));
#97788=CARTESIAN_POINT('Ctrl Pts',(2.25053562617268,0.748601478982124,22.3974461389909));
#97789=CARTESIAN_POINT('Ctrl Pts',(2.27108654838645,0.685866116138081,22.3930728651433));
#97790=CARTESIAN_POINT('Ctrl Pts',(2.28643854959801,0.63280829443864,22.3895139067073));
#97791=CARTESIAN_POINT('Ctrl Pts',(2.33567686229873,0.437309186656213,22.3767417755981));
#97792=CARTESIAN_POINT('Ctrl Pts',(2.35821259573262,0.292345100244275,22.3679059322618));
#97793=CARTESIAN_POINT('Ctrl Pts',(2.37573060778353,0.0087345427848194,
22.3504251767472));
#97794=CARTESIAN_POINT('Ctrl Pts',(2.37222878365669,-0.129208747688607,
22.3418307580727));
#97795=CARTESIAN_POINT('Ctrl Pts',(2.35467101395557,-0.284738299946942,
22.3316111759174));
#97796=CARTESIAN_POINT('Ctrl Pts',(2.35234014830279,-0.303392940979651,
22.3303770596217));
#97797=CARTESIAN_POINT('Ctrl Pts',(2.34819565296708,-0.333635662487942,
22.3283618240845));
#97798=CARTESIAN_POINT('Ctrl Pts',(2.34651736325497,-0.345241705859396,
22.3275849727099));
#97799=CARTESIAN_POINT('Ctrl Pts',(2.34337426835055,-0.365894917318421,
22.3261961356001));
#97800=CARTESIAN_POINT('Ctrl Pts',(2.34194295242273,-0.374947003757861,
22.3255852220063));
#97801=CARTESIAN_POINT('Ctrl Pts',(2.33881233944465,-0.394028394591959,
22.3242926905392));
#97802=CARTESIAN_POINT('Ctrl Pts',(2.33710091524349,-0.404055492786182,
22.3236106987906));
#97803=CARTESIAN_POINT('Ctrl Pts',(2.33238516107864,-0.430651934568372,
22.3217942003855));
#97804=CARTESIAN_POINT('Ctrl Pts',(2.3292688244095,-0.447200566225111,22.3206561536112));
#97805=CARTESIAN_POINT('Ctrl Pts',(2.31343137277644,-0.526640743817441,
22.3151544099515));
#97806=CARTESIAN_POINT('Ctrl Pts',(2.29833889832132,-0.589026421161469,
22.3107158148247));
#97807=CARTESIAN_POINT('Ctrl Pts',(2.24667769393948,-0.770096421624441,
22.2974731939092));
#97808=CARTESIAN_POINT('Ctrl Pts',(2.20330182225574,-0.886602234784846,
22.2884769534929));
#97809=CARTESIAN_POINT('Ctrl Pts',(2.08969720088046,-1.13117159459081,22.2687865486903));
#97810=CARTESIAN_POINT('Ctrl Pts',(2.01635211822775,-1.25726515815862,22.2581052159777));
#97811=CARTESIAN_POINT('Ctrl Pts',(1.92099084130839,-1.39116713934443,22.2466725232534));
#97812=CARTESIAN_POINT('Ctrl Pts',(1.90989778446525,-1.40635782459123,22.2453744506698));
#97813=CARTESIAN_POINT('Ctrl Pts',(1.89401888562998,-1.42756771711007,22.2435623154559));
#97814=CARTESIAN_POINT('Ctrl Pts',(1.88938305526383,-1.43369759737538,22.2430386246045));
#97815=CARTESIAN_POINT('Ctrl Pts',(1.88153516020645,-1.44397056154901,22.2421611902558));
#97816=CARTESIAN_POINT('Ctrl Pts',(1.87833903752116,-1.44812568643083,22.2418063514578));
#97817=CARTESIAN_POINT('Ctrl Pts',(1.87178857893538,-1.45658344802342,22.2410842537291));
#97818=CARTESIAN_POINT('Ctrl Pts',(1.86843313390856,-1.4608851600815,22.2407170768141));
#97819=CARTESIAN_POINT('Ctrl Pts',(1.85984586255607,-1.47181613912727,22.2397841711837));
#97820=CARTESIAN_POINT('Ctrl Pts',(1.85459336189353,-1.47842918238691,22.2392198924448));
#97821=CARTESIAN_POINT('Ctrl Pts',(1.83310875999604,-1.50518420920423,22.2369367355733));
#97822=CARTESIAN_POINT('Ctrl Pts',(1.81658223073776,-1.52508896983998,22.2352376846321));
#97823=CARTESIAN_POINT('Ctrl Pts',(1.66898045397467,-1.69705777631759,22.2205137942694));
#97824=CARTESIAN_POINT('Ctrl Pts',(1.51939838463671,-1.83219894696173,22.2085757046488));
#97825=CARTESIAN_POINT('Ctrl Pts',(1.25777705256605,-2.0142232443051,22.1888706192198));
#97826=CARTESIAN_POINT('Ctrl Pts',(1.15612409711372,-2.07423957517887,22.1814570447898));
#97827=CARTESIAN_POINT('Ctrl Pts',(1.03387126812045,-2.13463106299017,22.172550809892));
#97828=CARTESIAN_POINT('Ctrl Pts',(1.01720788026547,-2.14262168163942,22.1713373490584));
#97829=CARTESIAN_POINT('Ctrl Pts',(0.989907924936696,-2.15532262892487,
22.1693492213105));
#97830=CARTESIAN_POINT('Ctrl Pts',(0.979326869954151,-2.16015096884906,
22.1685786324842));
#97831=CARTESIAN_POINT('Ctrl Pts',(0.960355589066737,-2.16863989490611,
22.1671967653391));
#97832=CARTESIAN_POINT('Ctrl Pts',(0.951978819150639,-2.17233012571177,
22.1665865186913));
#97833=CARTESIAN_POINT('Ctrl Pts',(0.93419870359439,-2.18004023469208,22.165290958559));
#97834=CARTESIAN_POINT('Ctrl Pts',(0.924790324524047,-2.18404796024462,
22.1646052453137));
#97835=CARTESIAN_POINT('Ctrl Pts',(0.899593656440859,-2.19458908861085,
22.1627682266017));
#97836=CARTESIAN_POINT('Ctrl Pts',(0.883760436108778,-2.20101283036097,
22.1616132377799));
#97837=CARTESIAN_POINT('Ctrl Pts',(0.80531821378666,-2.23185499830731,22.1558868524616));
#97838=CARTESIAN_POINT('Ctrl Pts',(0.741766087422282,-2.2537736483378,22.151232922541));
#97839=CARTESIAN_POINT('Ctrl Pts',(0.520727822627718,-2.31964610485719,
22.1349843343499));
#97840=CARTESIAN_POINT('Ctrl Pts',(0.359690986436795,-2.35000530284568,
22.1230036226616));
#97841=CARTESIAN_POINT('Ctrl Pts',(0.0851343241601928,-2.37287059348336,
22.1029173686899));
#97842=CARTESIAN_POINT('Ctrl Pts',(-0.0271048666478931,-2.37424395256842,
22.0948135971194));
#97843=CARTESIAN_POINT('Ctrl Pts',(-0.15166199778756,-2.36692981711399,
22.0862046294874));
#97844=CARTESIAN_POINT('Ctrl Pts',(-0.164285871328655,-2.36608712666981,
22.0853365979133));
#97845=CARTESIAN_POINT('Ctrl Pts',(-0.183332743319528,-2.3646625010613,
22.0840342921502));
#97846=CARTESIAN_POINT('Ctrl Pts',(-0.18976085257933,-2.36415533754365,
22.0835960485616));
#97847=CARTESIAN_POINT('Ctrl Pts',(-0.201281946383875,-2.36319905611051,
22.0828129587086));
#97848=CARTESIAN_POINT('Ctrl Pts',(-0.206375599236724,-2.3627596818984,
22.0824675815885));
#97849=CARTESIAN_POINT('Ctrl Pts',(-0.217502963796395,-2.36176358606488,
22.081714926538));
#97850=CARTESIAN_POINT('Ctrl Pts',(-0.223535968465657,-2.36120021357984,
22.0813080247748));
#97851=CARTESIAN_POINT('Ctrl Pts',(-0.240705807942999,-2.35953046742589,
22.0801531528503));
#97852=CARTESIAN_POINT('Ctrl Pts',(-0.251837250040576,-2.35836836065011,
22.0794082264967));
#97853=CARTESIAN_POINT('Ctrl Pts',(-0.325919585033467,-2.35010376110711,
22.0744733418479));
#97854=CARTESIAN_POINT('Ctrl Pts',(-0.388578810020382,-2.34055963903911,
22.07040882942));
#97855=CARTESIAN_POINT('Ctrl Pts',(-0.655453211487854,-2.2888943756156,
22.0532807400586));
#97856=CARTESIAN_POINT('Ctrl Pts',(-0.854007189412205,-2.22246232191954,
22.0409229353592));
#97857=CARTESIAN_POINT('Ctrl Pts',(-1.1056949917092,-2.09946873554599,22.0232697713006));
#97858=CARTESIAN_POINT('Ctrl Pts',(-1.16859702136822,-2.06511738399075,
22.0186819910675));
#97859=CARTESIAN_POINT('Ctrl Pts',(-1.24509278078565,-2.01872734046536,
22.0128247049149));
#97860=CARTESIAN_POINT('Ctrl Pts',(-1.26023652631886,-2.00930833293617,
22.0116510711955));
#97861=CARTESIAN_POINT('Ctrl Pts',(-1.28400505475438,-1.99415053552777,
22.0097858828075));
#97862=CARTESIAN_POINT('Ctrl Pts',(-1.29270113915319,-1.98852435187852,
22.0090985033454));
#97863=CARTESIAN_POINT('Ctrl Pts',(-1.30825575156846,-1.97831569404206,
22.0078598845519));
#97864=CARTESIAN_POINT('Ctrl Pts',(-1.31512779394561,-1.97375403215099,
22.0073094319387));
#97865=CARTESIAN_POINT('Ctrl Pts',(-1.32220960092254,-1.96899972397383,
22.0067387890254));
#97866=CARTESIAN_POINT('Ctrl Pts',(-1.32244334638204,-1.968842740645,22.0067199502854));
#97867=CARTESIAN_POINT('Ctrl Pts',(-1.32286524144993,-1.96855928710787,
22.0066859406889));
#97868=CARTESIAN_POINT('Ctrl Pts',(-1.32305340092178,-1.9684328315196,22.0066707703857));
#97869=CARTESIAN_POINT('Ctrl Pts',(-1.32339807141807,-1.96820111844338,
22.006642976872));
#97870=CARTESIAN_POINT('Ctrl Pts',(-1.32355458804031,-1.96809586924831,
22.0066303539755));
#97871=CARTESIAN_POINT('Ctrl Pts',(-1.32384448485905,-1.96790087866541,
22.0066069709215));
#97872=CARTESIAN_POINT('Ctrl Pts',(-1.32397786850046,-1.96781114237743,
22.0065962109571));
#97873=CARTESIAN_POINT('Ctrl Pts',(-1.32444671828358,-1.96749564584857,
22.0065583847778));
#97874=CARTESIAN_POINT('Ctrl Pts',(-1.32478213565962,-1.96726981348315,
22.0065313158332));
#97875=CARTESIAN_POINT('Ctrl Pts',(-1.32544671157619,-1.9668221157089,22.0064776673505));
#97876=CARTESIAN_POINT('Ctrl Pts',(-1.32577587221057,-1.96660025341546,
22.0064510879309));
#97877=CARTESIAN_POINT('Ctrl Pts',(-1.32643079394499,-1.9661585810436,22.0063981883991));
#97878=CARTESIAN_POINT('Ctrl Pts',(-1.32675655614569,-1.96593877261247,
22.0063718683498));
#97879=CARTESIAN_POINT('Ctrl Pts',(-1.32740710142896,-1.9654995810707,22.0063192923926));
#97880=CARTESIAN_POINT('Ctrl Pts',(-1.32773188479249,-1.96528019839874,
22.006293036502));
#97881=CARTESIAN_POINT('Ctrl Pts',(-1.3283825898726,-1.96484042919996,22.0062404177473));
#97882=CARTESIAN_POINT('Ctrl Pts',(-1.32870851115816,-1.96462004206179,
22.0062140548607));
#97883=CARTESIAN_POINT('Ctrl Pts',(-1.32936340082975,-1.96417696983835,
22.0061610674971));
#97884=CARTESIAN_POINT('Ctrl Pts',(-1.32969236813491,-1.96395428318289,
22.0061344429611));
#97885=CARTESIAN_POINT('Ctrl Pts',(-1.3303551175035,-1.96350540778583,22.0060807887469));
#97886=CARTESIAN_POINT('Ctrl Pts',(-1.33068889786266,-1.96327921656006,
22.0060537589749));
#97887=CARTESIAN_POINT('Ctrl Pts',(-1.33136295002236,-1.96282218422363,
22.0059991577652));
#97888=CARTESIAN_POINT('Ctrl Pts',(-1.33170321949915,-1.96259133972101,
22.0059715861992));
#97889=CARTESIAN_POINT('Ctrl Pts',(-1.33239187388041,-1.96212388351877,
22.005915768812));
#97890=CARTESIAN_POINT('Ctrl Pts',(-1.3327402558166,-1.96188726750107,22.0058875228276));
#97891=CARTESIAN_POINT('Ctrl Pts',(-1.33344673639335,-1.96140716100058,
22.005830225511));
#97892=CARTESIAN_POINT('Ctrl Pts',(-1.33380483139542,-1.96116366521722,
22.0058011739782));
#97893=CARTESIAN_POINT('Ctrl Pts',(-1.34477760200122,-1.95369805597566,
22.0049106945234));
#97894=CARTESIAN_POINT('Ctrl Pts',(-1.35533334239517,-1.94639009770567,
22.0040460111039));
#97895=CARTESIAN_POINT('Ctrl Pts',(-1.39232117469314,-1.92033587589226,
22.0009872205718));
#97896=CARTESIAN_POINT('Ctrl Pts',(-1.4184268609842,-1.9011347106955,21.9987757498885));
#97897=CARTESIAN_POINT('Ctrl Pts',(-1.57354345669432,-1.78207026290825,
21.9853066189334));
#97898=CARTESIAN_POINT('Ctrl Pts',(-1.69233947505689,-1.66966532434441,
21.9735434158214));
#97899=CARTESIAN_POINT('Ctrl Pts',(-1.89397986574322,-1.4350712283036,21.9509569684146));
#97900=CARTESIAN_POINT('Ctrl Pts',(-1.97885994181885,-1.31556470744714,
21.9402215775618));
#97901=CARTESIAN_POINT('Ctrl Pts',(-2.06161886714287,-1.17272296189314,
21.9287405900638));
#97902=CARTESIAN_POINT('Ctrl Pts',(-2.07085013913471,-1.15634391761101,
21.9274431193352));
#97903=CARTESIAN_POINT('Ctrl Pts',(-2.08357882973607,-1.13311798289429,
21.925631680632));
#97904=CARTESIAN_POINT('Ctrl Pts',(-2.08723892837341,-1.12636173716228,
21.9251080938001));
#97905=CARTESIAN_POINT('Ctrl Pts',(-2.09334054744121,-1.11496676651852,
21.9242307873889));
#97906=CARTESIAN_POINT('Ctrl Pts',(-2.09579961746597,-1.11033756276992,
21.9238759731474));
#97907=CARTESIAN_POINT('Ctrl Pts',(-2.10078687889581,-1.10087343447876,
21.9231538757216));
#97908=CARTESIAN_POINT('Ctrl Pts',(-2.10331376505755,-1.09603788098158,
21.9227866748165));
#97909=CARTESIAN_POINT('Ctrl Pts',(-2.10971011012355,-1.08369398807491,
21.9218536324405));
#97910=CARTESIAN_POINT('Ctrl Pts',(-2.11355622821125,-1.0761735381388,21.9212892417931));
#97911=CARTESIAN_POINT('Ctrl Pts',(-2.12902388036512,-1.04552631413782,
21.9190050451138));
#97912=CARTESIAN_POINT('Ctrl Pts',(-2.14030719151979,-1.02222953401307,
21.9173050890662));
#97913=CARTESIAN_POINT('Ctrl Pts',(-2.23573894869351,-0.81667940615521,
21.9025816310169));
#97914=CARTESIAN_POINT('Ctrl Pts',(-2.29682560593683,-0.624587548032487,
21.8906445207192));
#97915=CARTESIAN_POINT('Ctrl Pts',(-2.35337179105881,-0.315691106495283,
21.8712290678143));
#97916=CARTESIAN_POINT('Ctrl Pts',(-2.36575636723831,-0.203006181453386,
21.8641141618005));
#97917=CARTESIAN_POINT('Ctrl Pts',(-2.37078592792978,-0.0703770985275363,
21.8554684593717));
#97918=CARTESIAN_POINT('Ctrl Pts',(-2.37128469816994,-0.0508693935166852,
21.8541902450946));
#97919=CARTESIAN_POINT('Ctrl Pts',(-2.37168074547895,-0.0209173389730879,
21.8522166034159));
#97920=CARTESIAN_POINT('Ctrl Pts',(-2.37174984843327,-0.010475830427131,
21.8515265134037));
#97921=CARTESIAN_POINT('Ctrl Pts',(-2.37174999975095,-3.43714120204603E-5,
21.8508342761113));
#97922=CARTESIAN_POINT('Ctrl Pts',(-2.37174999975776,-3.38978675131843E-5,
21.8508342447167));
#97923=CARTESIAN_POINT('Ctrl Pts',(-2.37175006607408,0.00460609143751829,
21.8505266273684));
#97924=CARTESIAN_POINT('Ctrl Pts',(-2.37173651617879,0.0092460494356073,
21.8502185875369));
#97925=CARTESIAN_POINT('Ctrl Pts',(-2.37166471319693,0.021509971748285,
21.8494032634202));
#97926=CARTESIAN_POINT('Ctrl Pts',(-2.3715833142655,0.0291336896286714,
21.8488952616669));
#97927=CARTESIAN_POINT('Ctrl Pts',(-2.37133201731076,0.0453467948163564,
21.8478123708432));
#97928=CARTESIAN_POINT('Ctrl Pts',(-2.37115220595646,0.0539358966119043,
21.8472371785136));
#97929=CARTESIAN_POINT('Ctrl Pts',(-2.37057114567083,0.0759699415556194,
21.8457576209211));
#97930=CARTESIAN_POINT('Ctrl Pts',(-2.37010218248026,0.0894126405761821,
21.8448511483548));
#97931=CARTESIAN_POINT('Ctrl Pts',(-2.36850195743618,0.126279430017873,
21.8423543364406));
#97932=CARTESIAN_POINT('Ctrl Pts',(-2.36713763174833,0.149690770951987,
21.8407568151855));
#97933=CARTESIAN_POINT('Ctrl Pts',(-2.36542649448459,0.173076750866022,
21.8391485779751));
#97934=CARTESIAN_POINT('',(-2.37174904524198,0.00212811977154857,21.6509744404708));
#97935=CARTESIAN_POINT('Ctrl Pts',(-2.36542651121823,0.173076522168564,
21.6404818371561));
#97936=CARTESIAN_POINT('Ctrl Pts',(-2.36958643853432,0.116223043516792,
21.643983241148));
#97937=CARTESIAN_POINT('Ctrl Pts',(-2.37169783275593,0.0592034623896574,
21.647469736661));
#97938=CARTESIAN_POINT('Ctrl Pts',(-2.37174904524198,0.00212811976785121,
21.650974440471));
#97939=CARTESIAN_POINT('Ctrl Pts',(-2.37174904629756,0.0021269430199922,
21.650974512729));
#97940=CARTESIAN_POINT('Ctrl Pts',(-2.37188012947853,-0.14404359682661,
21.6599500957589));
#97941=CARTESIAN_POINT('Ctrl Pts',(-2.35849905695474,-0.289898015962181,
21.669026738009));
#97942=CARTESIAN_POINT('Ctrl Pts',(-2.32884688216636,-0.449363718668568,
21.6795982553866));
#97943=CARTESIAN_POINT('Ctrl Pts',(-2.32575340206418,-0.465109282263969,
21.6806488982764));
#97944=CARTESIAN_POINT('Ctrl Pts',(-2.32032181906543,-0.491345302365815,
21.6824115454637));
#97945=CARTESIAN_POINT('Ctrl Pts',(-2.31807172338858,-0.501853593239797,
21.6831207704345));
#97946=CARTESIAN_POINT('Ctrl Pts',(-2.31350809805088,-0.522480698865444,
21.6845194900442));
#97947=CARTESIAN_POINT('Ctrl Pts',(-2.3111994006053,-0.532600342880585,
21.6852088169083));
#97948=CARTESIAN_POINT('Ctrl Pts',(-2.3066995574121,-0.551744002370816,
21.6865188991827));
#97949=CARTESIAN_POINT('Ctrl Pts',(-2.30452168872987,-0.560770964172024,
21.687139216707));
#97950=CARTESIAN_POINT('Ctrl Pts',(-2.2994575308212,-0.581233364623295,
21.6885512996239));
#97951=CARTESIAN_POINT('Ctrl Pts',(-2.29653885948676,-0.592660457870983,
21.6893440967877));
#97952=CARTESIAN_POINT('Ctrl Pts',(-2.28876367355726,-0.62218154948984,
21.6914034265844));
#97953=CARTESIAN_POINT('Ctrl Pts',(-2.28377786121515,-0.640240329378653,
21.6926741081978));
#97954=CARTESIAN_POINT('Ctrl Pts',(-2.24499355612233,-0.774497441852405,
21.7022048171245));
#97955=CARTESIAN_POINT('Ctrl Pts',(-2.20256557026734,-0.887997041866107,
21.7107468357777));
#97956=CARTESIAN_POINT('Ctrl Pts',(-2.11208029886235,-1.08313079961061,
21.7262690843966));
#97957=CARTESIAN_POINT('Ctrl Pts',(-2.06744264598954,-1.16607681094537,
21.7331578184411));
#97958=CARTESIAN_POINT('Ctrl Pts',(-1.96579793672407,-1.33067911144673,
21.7472751976184));
#97959=CARTESIAN_POINT('Ctrl Pts',(-1.90833360287904,-1.41185510616907,
21.7544878512084));
#97960=CARTESIAN_POINT('Ctrl Pts',(-1.82814147477453,-1.511257924464,21.7634521995085));
#97961=CARTESIAN_POINT('Ctrl Pts',(-1.80994585977779,-1.53300291306676,
21.7654216626015));
#97962=CARTESIAN_POINT('Ctrl Pts',(-1.78702116032091,-1.55942211674064,
21.7678196812142));
#97963=CARTESIAN_POINT('Ctrl Pts',(-1.7826575762754,-1.56440849332449,21.7682725178389));
#97964=CARTESIAN_POINT('Ctrl Pts',(-1.77417618846818,-1.57401882125165,
21.7691456193532));
#97965=CARTESIAN_POINT('Ctrl Pts',(-1.77006106671405,-1.57864505817989,
21.7695660693773));
#97966=CARTESIAN_POINT('Ctrl Pts',(-1.7624668964809,-1.58711542764778,21.7703360877015));
#97967=CARTESIAN_POINT('Ctrl Pts',(-1.75899337097757,-1.59096425597922,
21.7706860413732));
#97968=CARTESIAN_POINT('Ctrl Pts',(-1.75114003275701,-1.59960896119347,
21.7714722348941));
#97969=CARTESIAN_POINT('Ctrl Pts',(-1.7467531316196,-1.60439824943147,21.7719079311884));
#97970=CARTESIAN_POINT('Ctrl Pts',(-1.73378448791691,-1.61844019539197,
21.7731859827644));
#97971=CARTESIAN_POINT('Ctrl Pts',(-1.72514834036726,-1.627642632073,21.774024346926));
#97972=CARTESIAN_POINT('Ctrl Pts',(-1.65236556098458,-1.70396779751785,
21.7809889065736));
#97973=CARTESIAN_POINT('Ctrl Pts',(-1.58439336221097,-1.76734838936921,
21.7868463307339));
#97974=CARTESIAN_POINT('Ctrl Pts',(-1.36661359983591,-1.94772457219401,
21.8043899183517));
#97975=CARTESIAN_POINT('Ctrl Pts',(-1.20634289595142,-2.05085375841614,
21.815760416059));
#97976=CARTESIAN_POINT('Ctrl Pts',(-0.981023734734813,-2.16019799228492,
21.8316485274383));
#97977=CARTESIAN_POINT('Ctrl Pts',(-0.925572170371445,-2.18453155107848,
21.8355455080405));
#97978=CARTESIAN_POINT('Ctrl Pts',(-0.854011731363886,-2.21272013681538,
21.8405892147893));
#97979=CARTESIAN_POINT('Ctrl Pts',(-0.838707924389162,-2.21856607661768,
21.8416686272028));
#97980=CARTESIAN_POINT('Ctrl Pts',(-0.813644479467798,-2.22784373772877,
21.8434382416649));
#97981=CARTESIAN_POINT('Ctrl Pts',(-0.803920606814808,-2.23137103836728,
21.8441252445542));
#97982=CARTESIAN_POINT('Ctrl Pts',(-0.785417633066153,-2.23794628234331,
21.8454334906877));
#97983=CARTESIAN_POINT('Ctrl Pts',(-0.77664306145962,-2.24100646403119,
21.8460543132755));
#97984=CARTESIAN_POINT('Ctrl Pts',(-0.756633130805078,-2.24785340680719,
21.8474711316777));
#97985=CARTESIAN_POINT('Ctrl Pts',(-0.745386979465549,-2.25160762014272,
21.8482681857652));
#97986=CARTESIAN_POINT('Ctrl Pts',(-0.716102296300976,-2.26114005158752,
21.8503458996879));
#97987=CARTESIAN_POINT('Ctrl Pts',(-0.698022151720042,-2.26678668405509,
21.8516308322753));
#97988=CARTESIAN_POINT('Ctrl Pts',(-0.551807373138127,-2.31053605892426,
21.8620417890489));
#97989=CARTESIAN_POINT('Ctrl Pts',(-0.420750495740637,-2.33795337832828,
21.8715154523044));
#97990=CARTESIAN_POINT('Ctrl Pts',(-0.141558102718332,-2.37212064573167,
21.891889276526));
#97991=CARTESIAN_POINT('Ctrl Pts',(0.00633822451968406,-2.37633222090603,
21.9027934306858));
#97992=CARTESIAN_POINT('Ctrl Pts',(0.210758979647264,-2.36305989733668,
21.9174598193607));
#97993=CARTESIAN_POINT('Ctrl Pts',(0.26770496432654,-2.3572880040321,21.9214979645194));
#97994=CARTESIAN_POINT('Ctrl Pts',(0.335300960880602,-2.34795498544842,
21.9261933774168));
#97995=CARTESIAN_POINT('Ctrl Pts',(0.346200083593711,-2.34637270314822,
21.9269473929202));
#97996=CARTESIAN_POINT('Ctrl Pts',(0.363091922640616,-2.34380016228095,
21.9281108187206));
#97997=CARTESIAN_POINT('Ctrl Pts',(0.369092343728505,-2.34286273368837,
21.9285230827554));
#97998=CARTESIAN_POINT('Ctrl Pts',(0.380218101115711,-2.34108078431641,
21.9292855202694));
#97999=CARTESIAN_POINT('Ctrl Pts',(0.385344227360794,-2.34024248111527,
21.9296360231955));
#98000=CARTESIAN_POINT('Ctrl Pts',(0.397024076402254,-2.33829299460417,
21.9304328868139));
#98001=CARTESIAN_POINT('Ctrl Pts',(0.403575904828265,-2.33717109720774,
21.930878636808));
#98002=CARTESIAN_POINT('Ctrl Pts',(0.420668806571474,-2.33417018638141,
21.9320384780676));
#98003=CARTESIAN_POINT('Ctrl Pts',(0.431202169631757,-2.33224728607302,
21.932750173015));
#98004=CARTESIAN_POINT('Ctrl Pts',(0.503407777303255,-2.31856000283583,
21.9376101181506));
#98005=CARTESIAN_POINT('Ctrl Pts',(0.564610929381537,-2.30442096159721,
21.9416360058439));
#98006=CARTESIAN_POINT('Ctrl Pts',(0.689962150613862,-2.27016728151205,
21.9498218072764));
#98007=CARTESIAN_POINT('Ctrl Pts',(0.753960159498969,-2.24972270179852,
21.9539681057298));
#98008=CARTESIAN_POINT('Ctrl Pts',(0.931216382963815,-2.18468168759888,
21.965567187769));
#98009=CARTESIAN_POINT('Ctrl Pts',(1.04202787766788,-2.13405124425065,21.9729632454886));
#98010=CARTESIAN_POINT('Ctrl Pts',(1.2001391844809,-2.04654639097371,21.9842607170541));
#98011=CARTESIAN_POINT('Ctrl Pts',(1.25072412760167,-2.01602940660697,21.9879961495904));
#98012=CARTESIAN_POINT('Ctrl Pts',(1.33285041215006,-1.96220278919546,21.9943123989141));
#98013=CARTESIAN_POINT('Ctrl Pts',(1.36504817828165,-1.93994154315187,21.9968566097392));
#98014=CARTESIAN_POINT('Ctrl Pts',(1.40821591042066,-1.90848887172132,22.0003698654468));
#98015=CARTESIAN_POINT('Ctrl Pts',(1.4196765008619,-1.8999790635134,22.0013127240924));
#98016=CARTESIAN_POINT('Ctrl Pts',(1.43880408341467,-1.8855066137805,22.0029038462866));
#98017=CARTESIAN_POINT('Ctrl Pts',(1.44651263137386,-1.8795993146238,22.0035499335655));
#98018=CARTESIAN_POINT('Ctrl Pts',(1.46165766848853,-1.8678448571244,22.00482905456));
#98019=CARTESIAN_POINT('Ctrl Pts',(1.46909589040661,-1.86200021762661,22.0054619806849));
#98020=CARTESIAN_POINT('Ctrl Pts',(1.48540368264511,-1.84902770004391,22.0068601590178));
#98021=CARTESIAN_POINT('Ctrl Pts',(1.4942572795649,-1.84188021069459,22.0076261887216));
#98022=CARTESIAN_POINT('Ctrl Pts',(1.52524760055357,-1.8164912877595,22.0103324090326));
#98023=CARTESIAN_POINT('Ctrl Pts',(1.54710374133569,-1.79791288138436,22.0122862003529));
#98024=CARTESIAN_POINT('Ctrl Pts',(1.70815172666794,-1.65590579126623,22.0270326294601));
#98025=CARTESIAN_POINT('Ctrl Pts',(1.8326998453104,-1.51690172445385,22.0405108620913));
#98026=CARTESIAN_POINT('Ctrl Pts',(1.95804916479291,-1.33875208261829,22.0564217552804));
#98027=CARTESIAN_POINT('Ctrl Pts',(1.97586081226877,-1.31232151241464,22.0587488866696));
#98028=CARTESIAN_POINT('Ctrl Pts',(2.04567817146216,-1.20407485659599,22.0681292942927));
#98029=CARTESIAN_POINT('Ctrl Pts',(2.09318381532347,-1.11945569501166,22.0751259025091));
#98030=CARTESIAN_POINT('Ctrl Pts',(2.14356201109512,-1.01523072815927,22.0831734269785));
#98031=CARTESIAN_POINT('Ctrl Pts',(2.15154260214543,-0.998206398457185,
22.0844703903553));
#98032=CARTESIAN_POINT('Ctrl Pts',(2.16243502308225,-0.974232792292616,
22.0862705391073));
#98033=CARTESIAN_POINT('Ctrl Pts',(2.16551721945634,-0.967362361685569,
22.0867834433047));
#98034=CARTESIAN_POINT('Ctrl Pts',(2.17072101933894,-0.955613216022753,
22.0876553298763));
#98035=CARTESIAN_POINT('Ctrl Pts',(2.17285900938145,-0.950741862988018,
22.0880152975193));
#98036=CARTESIAN_POINT('Ctrl Pts',(2.17722749210149,-0.940696684311967,
22.0887543870363));
#98037=CARTESIAN_POINT('Ctrl Pts',(2.17945595923357,-0.935522061575013,
22.089133387077));
#98038=CARTESIAN_POINT('Ctrl Pts',(2.185204353286,-0.922041954443394,22.0901163275754));
#98039=CARTESIAN_POINT('Ctrl Pts',(2.18869541662435,-0.913724143938163,
22.0907185441087));
#98040=CARTESIAN_POINT('Ctrl Pts',(2.20260671050952,-0.880041852812717,
22.0931406350282));
#98041=CARTESIAN_POINT('Ctrl Pts',(2.21263465175103,-0.854516262387042,
22.0949384497254));
#98042=CARTESIAN_POINT('Ctrl Pts',(2.31160534342605,-0.589158087416821,
22.1132981743857));
#98043=CARTESIAN_POINT('Ctrl Pts',(2.36164696135619,-0.336587324802956,
22.1281801197011));
#98044=CARTESIAN_POINT('Ctrl Pts',(2.37263024203067,-0.014643083981033,
22.1485513928182));
#98045=CARTESIAN_POINT('Ctrl Pts',(2.37211312761258,0.0516402607674147,
22.1528070897304));
#98046=CARTESIAN_POINT('Ctrl Pts',(2.36796946157724,0.134957109608505,22.1582751161096));
#98047=CARTESIAN_POINT('Ctrl Pts',(2.36693057451503,0.152093464806864,22.1594060273946));
#98048=CARTESIAN_POINT('Ctrl Pts',(2.36496821508573,0.179527908339262,22.1612272548627));
#98049=CARTESIAN_POINT('Ctrl Pts',(2.36416326534706,0.189834078216609,22.1619138481391));
#98050=CARTESIAN_POINT('Ctrl Pts',(2.36250670901786,0.209395544393419,22.1632217724663));
#98051=CARTESIAN_POINT('Ctrl Pts',(2.36166802196505,0.218651764112619,22.1638426859007));
#98052=CARTESIAN_POINT('Ctrl Pts',(2.35963461996036,0.239715158632776,22.1652603506821));
#98053=CARTESIAN_POINT('Ctrl Pts',(2.35840565476579,0.251518698414878,22.1660581650507));
#98054=CARTESIAN_POINT('Ctrl Pts',(2.35498120107995,0.282173317508111,22.1681391718902));
#98055=CARTESIAN_POINT('Ctrl Pts',(2.35264797285727,0.3010078367596,22.1694266594914));
#98056=CARTESIAN_POINT('Ctrl Pts',(2.3312838109564,0.457999145687072,22.180234965604));
#98057=CARTESIAN_POINT('Ctrl Pts',(2.3003307894739,0.594233102229342,22.1901359903791));
#98058=CARTESIAN_POINT('Ctrl Pts',(2.22795590310611,0.819002502240006,22.2072651171016));
#98059=CARTESIAN_POINT('Ctrl Pts',(2.19270809477539,0.909166234695663,22.2143609871841));
#98060=CARTESIAN_POINT('Ctrl Pts',(2.1137449647882,1.07962368753853,22.2280239530832));
#98061=CARTESIAN_POINT('Ctrl Pts',(2.07069502286623,1.16005638319759,22.2345860480154));
#98062=CARTESIAN_POINT('Ctrl Pts',(2.01359560193973,1.25338089059117,22.2421869587339));
#98063=CARTESIAN_POINT('Ctrl Pts',(2.00389443805835,1.26883333715996,22.243444943498));
#98064=CARTESIAN_POINT('Ctrl Pts',(1.98998708262334,1.29042815785981,22.2452005312094));
#98065=CARTESIAN_POINT('Ctrl Pts',(1.98592912047796,1.29666454869589,22.2457072374982));
#98066=CARTESIAN_POINT('Ctrl Pts',(1.97892840409493,1.30731349008542,22.2465718223577));
#98067=CARTESIAN_POINT('Ctrl Pts',(1.97600009318352,1.31173542450993,22.2469306459759));
#98068=CARTESIAN_POINT('Ctrl Pts',(1.96991286461586,1.32086088151078,22.2476706926283));
#98069=CARTESIAN_POINT('Ctrl Pts',(1.96675190355217,1.32556294233046,22.2480517751314));
#98070=CARTESIAN_POINT('Ctrl Pts',(1.95843474268517,1.33783981972731,22.2490462625423));
#98071=CARTESIAN_POINT('Ctrl Pts',(1.95325137908773,1.34539625449051,22.2496578675058));
#98072=CARTESIAN_POINT('Ctrl Pts',(1.93173469802664,1.37637734385366,22.2521641944863));
#98073=CARTESIAN_POINT('Ctrl Pts',(1.91502196940298,1.3995372711884,22.2540348914062));
#98074=CARTESIAN_POINT('Ctrl Pts',(1.74529017117802,1.62601015470865,22.272360390465));
#98075=CARTESIAN_POINT('Ctrl Pts',(1.56089894808136,1.80376848451313,22.2871738322896));
#98076=CARTESIAN_POINT('Ctrl Pts',(1.29737515059554,1.98655353019216,22.3074562274472));
#98077=CARTESIAN_POINT('Ctrl Pts',(1.24144972943193,2.02197391305081,22.3117065141737));
#98078=CARTESIAN_POINT('Ctrl Pts',(1.16925153232451,2.06357539426526,22.3171684512662));
#98079=CARTESIAN_POINT('Ctrl Pts',(1.15429035615847,2.07198125029782,22.3182989114494));
#98080=CARTESIAN_POINT('Ctrl Pts',(1.13017394057919,2.08518866347215,22.3201195897213));
#98081=CARTESIAN_POINT('Ctrl Pts',(1.12107604676841,2.09009411028116,22.320806089069));
#98082=CARTESIAN_POINT('Ctrl Pts',(1.10373667803629,2.09929745338874,22.32211394973));
#98083=CARTESIAN_POINT('Ctrl Pts',(1.09550141403624,2.10360668848688,22.3227348941856));
#98084=CARTESIAN_POINT('Ctrl Pts',(1.07669150728283,2.11330886652205,22.324152790807));
#98085=CARTESIAN_POINT('Ctrl Pts',(1.06610134918203,2.11867101540827,22.3249508072048));
#98086=CARTESIAN_POINT('Ctrl Pts',(1.03846746618552,2.1324033213596,22.3270326718392));
#98087=CARTESIAN_POINT('Ctrl Pts',(1.02136296788795,2.14064855930857,22.3283208209198));
#98088=CARTESIAN_POINT('Ctrl Pts',(0.876800030451471,2.20820821235097,22.339206474802));
#98089=CARTESIAN_POINT('Ctrl Pts',(0.744422202246773,2.25627666622694,22.3491906896422));
#98090=CARTESIAN_POINT('Ctrl Pts',(0.470109495060137,2.32910363622487,22.3697841554716));
#98091=CARTESIAN_POINT('Ctrl Pts',(0.328582878283811,2.3532447326379,22.3803581365282));
#98092=CARTESIAN_POINT('Ctrl Pts',(0.13110300111649,2.36875788384632,22.3945217323217));
#98093=CARTESIAN_POINT('Ctrl Pts',(0.0763263095821373,2.371155271999,22.398385473687));
#98094=CARTESIAN_POINT('Ctrl Pts',(0.0106244495738307,2.37175119057223,
22.4029057009315));
#98095=CARTESIAN_POINT('Ctrl Pts',(-0.000262903066657681,2.37177497484476,
22.4036509760575));
#98096=CARTESIAN_POINT('Ctrl Pts',(-0.0171960727512356,2.37169536615083,
22.4048038573033));
#98097=CARTESIAN_POINT('Ctrl Pts',(-0.0232418063662103,2.37164382554773,
22.4052142370099));
#98098=CARTESIAN_POINT('Ctrl Pts',(-0.0344844800221831,2.37150498571862,
22.4059749945917));
#98099=CARTESIAN_POINT('Ctrl Pts',(-0.039681288991119,2.3714237227401,22.4063256888757));
#98100=CARTESIAN_POINT('Ctrl Pts',(-0.0515623861758423,2.37119886987704,
22.4071253055671));
#98101=CARTESIAN_POINT('Ctrl Pts',(-0.0582463598604284,2.37104410007626,
22.4075736003437));
#98102=CARTESIAN_POINT('Ctrl Pts',(-0.0757616024085256,2.37056441809999,
22.4087445041672));
#98103=CARTESIAN_POINT('Ctrl Pts',(-0.0865916066402694,2.37019353333702,
22.4094646415977));
#98104=CARTESIAN_POINT('Ctrl Pts',(-0.163202786603556,2.36704409349722,
22.4145340127815));
#98105=CARTESIAN_POINT('Ctrl Pts',(-0.228852550289266,2.36160140775172,
22.4187485629111));
#98106=CARTESIAN_POINT('Ctrl Pts',(-0.429622478481986,2.33650363113286,
22.4314701649112));
#98107=CARTESIAN_POINT('Ctrl Pts',(-0.563340803168248,2.3079159633336,22.4397203620771));
#98108=CARTESIAN_POINT('Ctrl Pts',(-0.811402457582291,2.23202430107256,
22.4556909955144));
#98109=CARTESIAN_POINT('Ctrl Pts',(-0.925953221603575,2.18698684515527,
22.4633581653699));
#98110=CARTESIAN_POINT('Ctrl Pts',(-1.06206334168855,2.12085546286663,22.473172376375));
#98111=CARTESIAN_POINT('Ctrl Pts',(-1.08741010812859,2.10797191143811,22.4750310229163));
#98112=CARTESIAN_POINT('Ctrl Pts',(-1.12364331012592,2.08872747242237,22.4777361196238));
#98113=CARTESIAN_POINT('Ctrl Pts',(-1.13472089207309,2.08273023437895,22.4785697568969));
#98114=CARTESIAN_POINT('Ctrl Pts',(-1.15397707441661,2.07210599699617,22.480030715553));
#98115=CARTESIAN_POINT('Ctrl Pts',(-1.16217700219262,2.06751806818695,22.4806566320012));
#98116=CARTESIAN_POINT('Ctrl Pts',(-1.17799904624854,2.05854163489464,22.4818718292058));
#98117=CARTESIAN_POINT('Ctrl Pts',(-1.18562445104928,2.05415921316244,22.4824608831453));
#98118=CARTESIAN_POINT('Ctrl Pts',(-1.20373883479151,2.04361416982451,22.4838684029715));
#98119=CARTESIAN_POINT('Ctrl Pts',(-1.21420503378303,2.03741311073883,22.4846882537639));
#98120=CARTESIAN_POINT('Ctrl Pts',(-1.25164647371089,2.0148386809647,22.4876453432213));
#98121=CARTESIAN_POINT('Ctrl Pts',(-1.27834099522613,1.99800849295929,22.4897991913964));
#98122=CARTESIAN_POINT('Ctrl Pts',(-1.5172480024249,1.84063615071706,22.5095026416014));
#98123=CARTESIAN_POINT('Ctrl Pts',(-1.70585503767571,1.66732762664449,22.5284260927669));
#98124=CARTESIAN_POINT('Ctrl Pts',(-1.90454155807901,1.41505123651421,22.5515249591234));
#98125=CARTESIAN_POINT('Ctrl Pts',(-1.94359283469667,1.3609178219825,22.5562548987976));
#98126=CARTESIAN_POINT('Ctrl Pts',(-1.98661120255633,1.29564847633764,22.5616374814979));
#98127=CARTESIAN_POINT('Ctrl Pts',(-1.99284029585741,1.28604689372995,22.5624214610316));
#98128=CARTESIAN_POINT('Ctrl Pts',(-2.00231797058502,1.27120369051112,22.5636209692646));
#98129=CARTESIAN_POINT('Ctrl Pts',(-2.00561591425012,1.26599403032063,22.5640396338283));
#98130=CARTESIAN_POINT('Ctrl Pts',(-2.01165030430024,1.25637892772263,22.5648079532478));
#98131=CARTESIAN_POINT('Ctrl Pts',(-2.01439260692912,1.25197738917158,22.5651579814293));
#98132=CARTESIAN_POINT('Ctrl Pts',(-2.02055308143064,1.2420168642996,22.565946305158));
#98133=CARTESIAN_POINT('Ctrl Pts',(-2.02396275696216,1.23645275166331,22.5663840434118));
#98134=CARTESIAN_POINT('Ctrl Pts',(-2.03397400628247,1.21996341811316,22.5676737460992));
#98135=CARTESIAN_POINT('Ctrl Pts',(-2.04051052669679,1.20899867998439,22.5685216097931));
#98136=CARTESIAN_POINT('Ctrl Pts',(-2.10045129965389,1.10657950429431,22.5763564263201));
#98137=CARTESIAN_POINT('Ctrl Pts',(-2.14776992026356,1.01168397188873,22.5829925433187));
#98138=CARTESIAN_POINT('Ctrl Pts',(-2.22777191451311,0.820103133794522,
22.595814061272));
#98139=CARTESIAN_POINT('Ctrl Pts',(-2.26087917626553,0.723852633869651,
22.6019948224209));
#98140=CARTESIAN_POINT('Ctrl Pts',(-2.31046247031473,0.542585729870637,
22.613582236249));
#98141=CARTESIAN_POINT('Ctrl Pts',(-2.32866145897594,0.45822487196253,22.6189544039954));
#98142=CARTESIAN_POINT('Ctrl Pts',(-2.35026819610624,0.322570682446353,
22.6277192803704));
#98143=CARTESIAN_POINT('Ctrl Pts',(-2.35667537937432,0.271832627306682,
22.6310244615013));
#98144=CARTESIAN_POINT('Ctrl Pts',(-2.36290425392802,0.205254525262823,
22.6354148335364));
#98145=CARTESIAN_POINT('Ctrl Pts',(-2.36421465984301,0.189565175022731,
22.6364532564907));
#98146=CARTESIAN_POINT('Ctrl Pts',(-2.36538803639278,0.173601754216798,
22.6375140099822));
#98147=CARTESIAN_POINT('Ctrl Pts',(-2.36540728732125,0.173339253674963,
22.6375314540332));
#98148=CARTESIAN_POINT('Ctrl Pts',(-2.36542649454112,0.173076750093424,
22.6375488994376));
#98149=CARTESIAN_POINT('Origin',(0.,0.,-1.84858989190503));
#98150=CARTESIAN_POINT('',(-2.36542649454004,0.173076750108263,23.8347324553251));
#98151=CARTESIAN_POINT('',(-2.36542649498006,0.173076744094521,23.6397760267629));
#98152=CARTESIAN_POINT('',(-2.36542649454111,0.173076750093529,-1.84858989190503));
#98153=CARTESIAN_POINT('Ctrl Pts',(-2.36542649454004,0.173076750108263,
23.8347324553251));
#98154=CARTESIAN_POINT('Ctrl Pts',(-2.36521313794873,0.175992678062693,
23.8345313836012));
#98155=CARTESIAN_POINT('Ctrl Pts',(-2.36499438735582,0.178908241316125,
23.834330581952));
#98156=CARTESIAN_POINT('Ctrl Pts',(-2.36425986193181,0.188461377098688,
23.8336734540962));
#98157=CARTESIAN_POINT('Ctrl Pts',(-2.36372152556061,0.195097251863204,
23.833218290546));
#98158=CARTESIAN_POINT('Ctrl Pts',(-2.36272707028727,0.206746694398436,
23.8324216189125));
#98159=CARTESIAN_POINT('Ctrl Pts',(-2.3622829210848,0.211761201046456,23.8320794661881));
#98160=CARTESIAN_POINT('Ctrl Pts',(-2.3613697446941,0.221710538565071,23.8314021861645));
#98161=CARTESIAN_POINT('Ctrl Pts',(-2.36090121088067,0.226645335461349,
23.8310670422598));
#98162=CARTESIAN_POINT('Ctrl Pts',(-2.35985728557643,0.237285771784479,
23.8303460997473));
#98163=CARTESIAN_POINT('Ctrl Pts',(-2.35927667342204,0.242990793664687,
23.8299605980873));
#98164=CARTESIAN_POINT('Ctrl Pts',(-2.35765841762324,0.258338748278819,
23.8289261700615));
#98165=CARTESIAN_POINT('Ctrl Pts',(-2.3565822948449,0.267977646112384,23.8282793613162));
#98166=CARTESIAN_POINT('Ctrl Pts',(-2.35146978022023,0.311355992487421,
23.8253801864661));
#98167=CARTESIAN_POINT('Ctrl Pts',(-2.34676749748528,0.345014911616439,
23.8231624700867));
#98168=CARTESIAN_POINT('Ctrl Pts',(-2.33491738404618,0.418305656405469,
23.8183803982314));
#98169=CARTESIAN_POINT('Ctrl Pts',(-2.32748037347506,0.457880193432647,
23.8158284349045));
#98170=CARTESIAN_POINT('Ctrl Pts',(-2.27523796823757,0.701525462369068,
23.8001994040348));
#98171=CARTESIAN_POINT('Ctrl Pts',(-2.20463981528273,0.899120122662086,
23.7877997598158));
#98172=CARTESIAN_POINT('Ctrl Pts',(-2.07902091174658,1.14332131371335,23.7704256929237));
#98173=CARTESIAN_POINT('Ctrl Pts',(-2.04656744409077,1.20044659412911,23.7662058700489));
#98174=CARTESIAN_POINT('Ctrl Pts',(-2.0027876216054,1.27056230931542,23.7607864832281));
#98175=CARTESIAN_POINT('Ctrl Pts',(-1.99363295087202,1.28487916603263,23.7596668854329));
#98176=CARTESIAN_POINT('Ctrl Pts',(-1.97872578581389,1.30764935705449,23.757864606012));
#98177=CARTESIAN_POINT('Ctrl Pts',(-1.9730709862839,1.31616619541743,23.757185572392));
#98178=CARTESIAN_POINT('Ctrl Pts',(-1.96223187422345,1.33226442004618,23.7558925695491));
#98179=CARTESIAN_POINT('Ctrl Pts',(-1.95705822815673,1.33985279066526,23.7552790106854));
#98180=CARTESIAN_POINT('Ctrl Pts',(-1.94518470362675,1.35705261415231,23.7538789233561));
#98181=CARTESIAN_POINT('Ctrl Pts',(-1.93845746113787,1.36664479349996,23.7530913632644));
#98182=CARTESIAN_POINT('Ctrl Pts',(-1.92080248554561,1.39142588213364,23.7510388989541));
#98183=CARTESIAN_POINT('Ctrl Pts',(-1.90976576391999,1.40653576773763,23.7497698333138));
#98184=CARTESIAN_POINT('Ctrl Pts',(-1.80584043185118,1.54533688914444,23.737945009887));
#98185=CARTESIAN_POINT('Ctrl Pts',(-1.70125634563476,1.65976976458415,23.7269158091475));
#98186=CARTESIAN_POINT('Ctrl Pts',(-1.48959879474454,1.85019298693801,23.7062066580574));
#98187=CARTESIAN_POINT('Ctrl Pts',(-1.38590113822146,1.92909264605851,23.6966348156477));
#98188=CARTESIAN_POINT('Ctrl Pts',(-1.24611658568828,2.01833347925838,23.6847896863805));
#98189=CARTESIAN_POINT('Ctrl Pts',(-1.21554538902937,2.03689132620092,23.6822594883462));
#98190=CARTESIAN_POINT('Ctrl Pts',(-1.1711530099552,2.06248353705227,23.6786825573337));
#98191=CARTESIAN_POINT('Ctrl Pts',(-1.15766563500709,2.07008406118458,23.677608356588));
#98192=CARTESIAN_POINT('Ctrl Pts',(-1.13363324103126,2.08331865887766,23.6757176755115));
#98193=CARTESIAN_POINT('Ctrl Pts',(-1.12311835901335,2.08900601393742,23.6748982689628));
#98194=CARTESIAN_POINT('Ctrl Pts',(-1.1071052755875,2.09751141325316,23.6736627212651));
#98195=CARTESIAN_POINT('Ctrl Pts',(-1.10163852005926,2.10038777212284,23.6732430746725));
#98196=CARTESIAN_POINT('Ctrl Pts',(-1.09614594010506,2.10325037519577,23.6728236548216));
#98197=CARTESIAN_POINT('Ctrl Pts',(-1.09613136919284,2.10325796901888,23.6728225421852));
#98198=CARTESIAN_POINT('Ctrl Pts',(-1.09610218260238,2.1032731796098,23.6728203135252));
#98199=CARTESIAN_POINT('Ctrl Pts',(-1.09608756691289,2.10328079638231,23.6728191975009));
#98200=CARTESIAN_POINT('Ctrl Pts',(-1.09605829047896,2.10329605301908,23.6728169620432));
#98201=CARTESIAN_POINT('Ctrl Pts',(-1.09604362975711,2.10330369287038,23.6728158426118));
#98202=CARTESIAN_POINT('Ctrl Pts',(-1.0960142629681,2.10331899581245,23.672813600318));
#98203=CARTESIAN_POINT('Ctrl Pts',(-1.0959995569568,2.10332665887291,23.6728124774601));
#98204=CARTESIAN_POINT('Ctrl Pts',(-1.0959700994035,2.10334200832631,23.6728102282995));
#98205=CARTESIAN_POINT('Ctrl Pts',(-1.09595534779118,2.10334969475468,23.6728091019916));
#98206=CARTESIAN_POINT('Ctrl Pts',(-1.09592579876749,2.10336509108006,23.6728068459109));
#98207=CARTESIAN_POINT('Ctrl Pts',(-1.09591100136163,2.10337280097299,23.6728057161386));
#98208=CARTESIAN_POINT('Ctrl Pts',(-1.09588136045039,2.10338824438037,23.6728034531066));
#98209=CARTESIAN_POINT('Ctrl Pts',(-1.09586651697123,2.10339597787993,23.6728023198489));
#98210=CARTESIAN_POINT('Ctrl Pts',(-1.09583678367889,2.10341146861906,23.6728000498284));
#98211=CARTESIAN_POINT('Ctrl Pts',(-1.09582189383909,2.10341922587125,23.6727989130636));
#98212=CARTESIAN_POINT('Ctrl Pts',(-1.09579206756248,2.10343476424889,23.6727966360093));
#98213=CARTESIAN_POINT('Ctrl Pts',(-1.09577713112336,2.1034425453743,23.6727954957195));
#98214=CARTESIAN_POINT('Ctrl Pts',(-1.09574721135856,2.10345813164545,23.6727932115934));
#98215=CARTESIAN_POINT('Ctrl Pts',(-1.09573222805405,2.1034659367789,23.6727920677587));
#98216=CARTESIAN_POINT('Ctrl Pts',(-1.09570221429531,2.10348157119942,23.6727897765228));
#98217=CARTESIAN_POINT('Ctrl Pts',(-1.09568718384419,2.10348940048359,23.6727886291219));
#98218=CARTESIAN_POINT('Ctrl Pts',(-1.0956570755362,2.10350508333507,23.6727863307345));
#98219=CARTESIAN_POINT('Ctrl Pts',(-1.09564199767223,2.10351293690479,23.6727851797475));
#98220=CARTESIAN_POINT('Ctrl Pts',(-1.09561179429435,2.1035286684507,23.6727828741695));
#98221=CARTESIAN_POINT('Ctrl Pts',(-1.09559666873913,2.1035365464471,23.6727817195754));
#98222=CARTESIAN_POINT('Ctrl Pts',(-1.09556636967161,2.10355232700241,23.6727794067601));
#98223=CARTESIAN_POINT('Ctrl Pts',(-1.09555119618796,2.10356022954509,23.6727782485411));
#98224=CARTESIAN_POINT('Ctrl Pts',(-1.09552105426528,2.10357592742604,23.6727759477882));
#98225=CARTESIAN_POINT('Ctrl Pts',(-1.09550608588474,2.10358372273944,23.6727748052582));
#98226=CARTESIAN_POINT('Ctrl Pts',(-1.09547592681293,2.10359942873321,23.6727725032624));
#98227=CARTESIAN_POINT('Ctrl Pts',(-1.0954607360854,2.10360733942639,23.6727713437943));
#98228=CARTESIAN_POINT('Ctrl Pts',(-1.09543012873505,2.10362327802809,23.6727690076503));
#98229=CARTESIAN_POINT('Ctrl Pts',(-1.09541471208834,2.10363130594279,23.672767830973));
#98230=CARTESIAN_POINT('Ctrl Pts',(-1.09538364918485,2.10364748090303,23.6727654601285));
#98231=CARTESIAN_POINT('Ctrl Pts',(-1.09536800296256,2.10365562792416,23.6727642659645));
#98232=CARTESIAN_POINT('Ctrl Pts',(-1.09533647720975,2.10367204300343,23.6727618598658));
#98233=CARTESIAN_POINT('Ctrl Pts',(-1.09532059762454,2.1036803110834,23.6727606479275));
#98234=CARTESIAN_POINT('Ctrl Pts',(-1.09528860131534,2.10369697025471,23.6727582059896));
#98235=CARTESIAN_POINT('Ctrl Pts',(-1.09527248461808,2.10370536132527,23.6727569759927));
#98236=CARTESIAN_POINT('Ctrl Pts',(-1.09524001018804,2.10372226848588,23.6727544976417));
#98237=CARTESIAN_POINT('Ctrl Pts',(-1.09522365247353,2.10373078455934,23.6727532492896));
#98238=CARTESIAN_POINT('Ctrl Pts',(-1.09519069208353,2.103747943748,23.6727507339307));
#98239=CARTESIAN_POINT('Ctrl Pts',(-1.09517408940007,2.10375658686006,23.6727494669237));
#98240=CARTESIAN_POINT('Ctrl Pts',(-1.09514063507814,2.10377400218312,23.672746913952));
#98241=CARTESIAN_POINT('Ctrl Pts',(-1.09512378340937,2.10378277440236,23.6727456279855));
#98242=CARTESIAN_POINT('Ctrl Pts',(-1.09508982699332,2.10380045006355,23.6727430367818));
#98243=CARTESIAN_POINT('Ctrl Pts',(-1.09507272227568,2.10380935348229,23.6727417315475));
#98244=CARTESIAN_POINT('Ctrl Pts',(-1.09503825561346,2.10382729367839,23.6727391014935));
#98245=CARTESIAN_POINT('Ctrl Pts',(-1.09502089364249,2.10383633046145,23.6727377766724));
#98246=CARTESIAN_POINT('Ctrl Pts',(-1.09498590822939,2.10385453957107,23.6727351071231));
#98247=CARTESIAN_POINT('Ctrl Pts',(-1.09496828479217,2.10386371188678,23.6727337623958));
#98248=CARTESIAN_POINT('Ctrl Pts',(-1.09493277214936,2.10388219427325,23.6727310527081));
#98249=CARTESIAN_POINT('Ctrl Pts',(-1.09491488289931,2.1038915043586,23.672729687745));
#98250=CARTESIAN_POINT('Ctrl Pts',(-1.09487883419898,2.10391026456504,23.6727269372497));
#98251=CARTESIAN_POINT('Ctrl Pts',(-1.09486067477835,2.10391971466189,23.6727255517204));
#98252=CARTESIAN_POINT('Ctrl Pts',(-1.09482408128368,2.10393875718215,23.6727227597549));
#98253=CARTESIAN_POINT('Ctrl Pts',(-1.09480564716241,2.10394834962105,23.6727213533159));
#98254=CARTESIAN_POINT('Ctrl Pts',(-1.0947684996824,2.10396767918335,23.6727185191836));
#98255=CARTESIAN_POINT('Ctrl Pts',(-1.09474978634802,2.10397741628468,23.672717091493));
#98256=CARTESIAN_POINT('Ctrl Pts',(-1.09471207578653,2.10399703756582,23.6727142145044));
#98257=CARTESIAN_POINT('Ctrl Pts',(-1.09469307856191,2.10400692173463,23.6727127652075));
#98258=CARTESIAN_POINT('Ctrl Pts',(-1.09465479551704,2.10402683956839,23.67270984465));
#98259=CARTESIAN_POINT('Ctrl Pts',(-1.0946355096674,2.10403687323863,23.6727083733881));
#98260=CARTESIAN_POINT('Ctrl Pts',(-1.09459664450278,2.10405709257861,23.6727054085315));
#98261=CARTESIAN_POINT('Ctrl Pts',(-1.09457706525111,2.10406727820509,23.6727039149426));
#98262=CARTESIAN_POINT('Ctrl Pts',(-1.09453760839208,2.10408780397049,23.6727009050615));
#98263=CARTESIAN_POINT('Ctrl Pts',(-1.09451773077602,2.1040981441033,23.6726993887696));
#98264=CARTESIAN_POINT('Ctrl Pts',(-1.09447767224156,2.10411898142243,23.6726963331078));
#98265=CARTESIAN_POINT('Ctrl Pts',(-1.09445749127362,2.10412947862353,23.672694793735));
#98266=CARTESIAN_POINT('Ctrl Pts',(-1.09441682092992,2.10415063270171,23.6726916915249));
#98267=CARTESIAN_POINT('Ctrl Pts',(-1.09439633154815,2.10416128957058,23.6726901286879));
#98268=CARTESIAN_POINT('Ctrl Pts',(-1.09435503917578,2.10418276565521,23.6726869791554));
#98269=CARTESIAN_POINT('Ctrl Pts',(-1.09433423618284,2.10419358486046,23.6726853924606));
#98270=CARTESIAN_POINT('Ctrl Pts',(-1.09429231130924,2.10421538832798,23.6726821948127));
#98271=CARTESIAN_POINT('Ctrl Pts',(-1.09427118942314,2.10422637258097,23.6726805838601));
#98272=CARTESIAN_POINT('Ctrl Pts',(-1.09422862138021,2.10424850890684,23.6726773372889));
#98273=CARTESIAN_POINT('Ctrl Pts',(-1.09420717522818,2.10425966096475,23.6726757016717));
#98274=CARTESIAN_POINT('Ctrl Pts',(-1.09416395319099,2.10428213570325,23.6726724053579));
#98275=CARTESIAN_POINT('Ctrl Pts',(-1.09414217728436,2.10429345838213,23.6726707446606));
#98276=CARTESIAN_POINT('Ctrl Pts',(-1.09409829015848,2.10431627722483,23.6726673977641));
#98277=CARTESIAN_POINT('Ctrl Pts',(-1.09407617893379,2.10432777337816,23.6726657115656));
#98278=CARTESIAN_POINT('Ctrl Pts',(-1.09403161549073,2.10435094208335,23.6726623132368));
#98279=CARTESIAN_POINT('Ctrl Pts',(-1.09400916325981,2.10436261462798,23.6726606011067));
#98280=CARTESIAN_POINT('Ctrl Pts',(-1.09396391200434,2.1043861390896,23.6726571504755));
#98281=CARTESIAN_POINT('Ctrl Pts',(-1.0939411129928,2.10439799098563,23.6726554119768));
#98282=CARTESIAN_POINT('Ctrl Pts',(-1.08964141779047,2.10663306669688,23.6723275534236));
#98283=CARTESIAN_POINT('Ctrl Pts',(-1.08535780243853,2.10884322286384,23.6720022701121));
#98284=CARTESIAN_POINT('Ctrl Pts',(-1.07533399526423,2.11397643150274,23.6712442230504));
#98285=CARTESIAN_POINT('Ctrl Pts',(-1.06958861676846,2.11688916754811,23.6708121069931));
#98286=CARTESIAN_POINT('Ctrl Pts',(-1.05257448115073,2.12542787616847,23.6695392520864));
#98287=CARTESIAN_POINT('Ctrl Pts',(-1.04127247586534,2.1309876450776,23.6687025047322));
#98288=CARTESIAN_POINT('Ctrl Pts',(-0.940926625929911,2.17936157822732,
23.661345926429));
#98289=CARTESIAN_POINT('Ctrl Pts',(-0.849320358175713,2.21666866288519,
23.6551312243294));
#98290=CARTESIAN_POINT('Ctrl Pts',(-0.588121170694252,2.30446205477606,
23.6380722041268));
#98291=CARTESIAN_POINT('Ctrl Pts',(-0.414838402408274,2.34186692684986,
23.6274560766513));
#98292=CARTESIAN_POINT('Ctrl Pts',(-0.172259230618248,2.3664373891252,23.6120422467127));
#98293=CARTESIAN_POINT('Ctrl Pts',(-0.105259339219353,2.37036248404714,
23.6077341991622));
#98294=CARTESIAN_POINT('Ctrl Pts',(-0.0211068496666656,2.37171760426656,
23.6022169764951));
#98295=CARTESIAN_POINT('Ctrl Pts',(-0.00402391345202829,2.37180810273268,
23.6010915718038));
#98296=CARTESIAN_POINT('Ctrl Pts',(0.0232869442456301,2.37165773505211,
23.5992830722208));
#98297=CARTESIAN_POINT('Ctrl Pts',(0.0335151327760142,2.37153524626704,
23.5986036885838));
#98298=CARTESIAN_POINT('Ctrl Pts',(0.0528993367509235,2.37117768348711,
23.5973120486883));
#98299=CARTESIAN_POINT('Ctrl Pts',(0.0620554315771254,2.37095572836017,
23.5967002150144));
#98300=CARTESIAN_POINT('Ctrl Pts',(0.0828459897703354,2.37033122689557,
23.5953068991122));
#98301=CARTESIAN_POINT('Ctrl Pts',(0.0944791624916371,2.36989604469401,
23.5945244081852));
#98302=CARTESIAN_POINT('Ctrl Pts',(0.124595059399102,2.36854735494653,23.5924910365971));
#98303=CARTESIAN_POINT('Ctrl Pts',(0.143070840973736,2.36750315775391,23.5912360998484));
#98304=CARTESIAN_POINT('Ctrl Pts',(0.279728087573277,2.35817422236538,23.5818964810739));
#98305=CARTESIAN_POINT('Ctrl Pts',(0.397134108619264,2.34126246367862,23.573541592238));
#98306=CARTESIAN_POINT('Ctrl Pts',(0.708752002267166,2.27225898370835,23.5505270915312));
#98307=CARTESIAN_POINT('Ctrl Pts',(0.898424657274827,2.20416041600553,23.535556948897));
#98308=CARTESIAN_POINT('Ctrl Pts',(1.10018794678767,2.10129656434137,23.5197002410519));
#98309=CARTESIAN_POINT('Ctrl Pts',(1.12293176815558,2.08923075595065,23.5179151878064));
#98310=CARTESIAN_POINT('Ctrl Pts',(1.1528563298866,2.07272559431387,23.5155741165569));
#98311=CARTESIAN_POINT('Ctrl Pts',(1.16021527926622,2.06861538665671,23.5149990253939));
#98312=CARTESIAN_POINT('Ctrl Pts',(1.17229729156827,2.06178244217671,23.5140560481075));
#98313=CARTESIAN_POINT('Ctrl Pts',(1.17703307824363,2.05908254155913,23.5136867386581));
#98314=CARTESIAN_POINT('Ctrl Pts',(1.18630237719542,2.0537556293337,23.5129645648943));
#98315=CARTESIAN_POINT('Ctrl Pts',(1.19083654679544,2.05112989223599,23.5126116275206));
#98316=CARTESIAN_POINT('Ctrl Pts',(1.20200262901963,2.0446141092736,23.5117431665545));
#98317=CARTESIAN_POINT('Ctrl Pts',(1.20862447628754,2.04070675391773,23.5112287533436));
#98318=CARTESIAN_POINT('Ctrl Pts',(1.23141771033269,2.02710728079874,23.5094597755772));
#98319=CARTESIAN_POINT('Ctrl Pts',(1.24749297544227,2.01725428165373,23.5082151424283));
#98320=CARTESIAN_POINT('Ctrl Pts',(1.38513924237059,1.93061207355577,23.4975680576467));
#98321=CARTESIAN_POINT('Ctrl Pts',(1.49962944556639,1.84309447536245,23.4887704813196));
#98322=CARTESIAN_POINT('Ctrl Pts',(1.69781700365633,1.66082722078565,23.4722735560336));
#98323=CARTESIAN_POINT('Ctrl Pts',(1.78324977539863,1.56874050544723,23.464602431382));
#98324=CARTESIAN_POINT('Ctrl Pts',(1.90100717021844,1.41969535016007,23.4525787980039));
#98325=CARTESIAN_POINT('Ctrl Pts',(1.93892950751035,1.36744810547589,23.448430710302));
#98326=CARTESIAN_POINT('Ctrl Pts',(1.98401058369055,1.29968623565738,23.443094549426));
#98327=CARTESIAN_POINT('Ctrl Pts',(1.99319902750171,1.28555043449443,23.4419837426714));
#98328=CARTESIAN_POINT('Ctrl Pts',(2.00768713422237,1.26273269583808,23.4401938535362));
#98329=CARTESIAN_POINT('Ctrl Pts',(2.01308312556053,1.25411236104989,23.4395183618577));
#98330=CARTESIAN_POINT('Ctrl Pts',(2.0232300493525,1.23766797376387,23.4382309835327));
#98331=CARTESIAN_POINT('Ctrl Pts',(2.02799146682588,1.22985058129126,23.4376194981242));
#98332=CARTESIAN_POINT('Ctrl Pts',(2.03873539359529,1.2119789329157,23.4362226135859));
#98333=CARTESIAN_POINT('Ctrl Pts',(2.04468896029643,1.20190764454556,23.4354361755094));
#98334=CARTESIAN_POINT('Ctrl Pts',(2.05997884896358,1.17560026165529,23.4333836363636));
#98335=CARTESIAN_POINT('Ctrl Pts',(2.06919764401533,1.15929716128147,23.432113336878));
#98336=CARTESIAN_POINT('Ctrl Pts',(2.15372560965346,1.00559177039827,23.4201501425658));
#98337=CARTESIAN_POINT('Ctrl Pts',(2.21542327885618,0.861179899036344,23.4089685305938));
#98338=CARTESIAN_POINT('Ctrl Pts',(2.29598560400879,0.605104599155677,23.3894240088308));
#98339=CARTESIAN_POINT('Ctrl Pts',(2.32195778633276,0.496199761280336,23.3812046810344));
#98340=CARTESIAN_POINT('Ctrl Pts',(2.3515417781784,0.316783438908808,23.3681045635035));
#98341=CARTESIAN_POINT('Ctrl Pts',(2.35986961506396,0.247220582269833,23.3631327452343));
#98342=CARTESIAN_POINT('Ctrl Pts',(2.36596368937732,0.165966785138111,23.3575218083263));
#98343=CARTESIAN_POINT('Ctrl Pts',(2.36673733666838,0.154543022470951,23.3567374642195));
#98344=CARTESIAN_POINT('Ctrl Pts',(2.36779692816067,0.137014967764215,23.355541383649));
#98345=CARTESIAN_POINT('Ctrl Pts',(2.36814204742628,0.130914627751493,23.3551264775818));
#98346=CARTESIAN_POINT('Ctrl Pts',(2.36873234556284,0.119713067216328,23.3543672159242));
#98347=CARTESIAN_POINT('Ctrl Pts',(2.36898462212039,0.114612409981005,23.3540224809888));
#98348=CARTESIAN_POINT('Ctrl Pts',(2.36951494687385,0.10313905708221,23.3532492543183));
#98349=CARTESIAN_POINT('Ctrl Pts',(2.36978376318234,0.096766041198624,23.3528212824365));
#98350=CARTESIAN_POINT('Ctrl Pts',(2.37049660678263,0.0780756713808241,
23.3515704250662));
#98351=CARTESIAN_POINT('Ctrl Pts',(2.37087034413836,0.0657556141695112,
23.350751339451));
#98352=CARTESIAN_POINT('Ctrl Pts',(2.37299230253983,-0.0284088394800388,
23.3445286151073));
#98353=CARTESIAN_POINT('Ctrl Pts',(2.37059831258936,-0.110301374516682,
23.3393337331117));
#98354=CARTESIAN_POINT('Ctrl Pts',(2.35256814407307,-0.332393527750058,
23.325444112802));
#98355=CARTESIAN_POINT('Ctrl Pts',(2.32866451942597,-0.471578742878834,
23.3169423946824));
#98356=CARTESIAN_POINT('Ctrl Pts',(2.26553857495637,-0.709673163410089,
23.3016969477584));
#98357=CARTESIAN_POINT('Ctrl Pts',(2.23178048833928,-0.809600419849382,
23.2950720155049));
#98358=CARTESIAN_POINT('Ctrl Pts',(2.18148942406516,-0.931121121142471,
23.2865260292116));
#98359=CARTESIAN_POINT('Ctrl Pts',(2.17108517973295,-0.955129155046752,
23.2848132653419));
#98360=CARTESIAN_POINT('Ctrl Pts',(2.15529782836025,-0.989967369701426,
23.2822896370721));
#98361=CARTESIAN_POINT('Ctrl Pts',(2.15022544942074,-1.00093687589132,23.2814894065501));
#98362=CARTESIAN_POINT('Ctrl Pts',(2.14113822885043,-1.02020098928727,23.2800739192183));
#98363=CARTESIAN_POINT('Ctrl Pts',(2.13715843700206,-1.02851192730985,23.2794598849882));
#98364=CARTESIAN_POINT('Ctrl Pts',(2.12929527522493,-1.04468974313156,23.278257941064));
#98365=CARTESIAN_POINT('Ctrl Pts',(2.12541648335709,-1.05255869061325,23.277670198773));
#98366=CARTESIAN_POINT('Ctrl Pts',(2.11483981806569,-1.07371882831812,23.2760811983146));
#98367=CARTESIAN_POINT('Ctrl Pts',(2.10806043784326,-1.08696860632082,23.2750770959752));
#98368=CARTESIAN_POINT('Ctrl Pts',(2.0821658779951,-1.13642401131925,23.2712942557773));
#98369=CARTESIAN_POINT('Ctrl Pts',(2.06223995106247,-1.17219465000897,23.2684870737217));
#98370=CARTESIAN_POINT('Ctrl Pts',(1.91775471701896,-1.41647555800478,23.2488044441098));
#98371=CARTESIAN_POINT('Ctrl Pts',(1.76274018414759,-1.60526804795243,23.2307402339452));
#98372=CARTESIAN_POINT('Ctrl Pts',(1.53271798853135,-1.8111657393774,23.2085429045993));
#98373=CARTESIAN_POINT('Ctrl Pts',(1.48177034157325,-1.85307966581385,23.2038700181985));
#98374=CARTESIAN_POINT('Ctrl Pts',(1.42011460329042,-1.89963164421286,23.198551462756));
#98375=CARTESIAN_POINT('Ctrl Pts',(1.4110434529972,-1.90637935804305,23.1977771545701));
#98376=CARTESIAN_POINT('Ctrl Pts',(1.3970152310102,-1.91665947563325,23.1965926807939));
#98377=CARTESIAN_POINT('Ctrl Pts',(1.39209238828904,-1.92023797634512,23.1961794501014));
#98378=CARTESIAN_POINT('Ctrl Pts',(1.38300828209876,-1.92678807838513,23.1954214582325));
#98379=CARTESIAN_POINT('Ctrl Pts',(1.37885119885717,-1.92976516182755,23.1950763305369));
#98380=CARTESIAN_POINT('Ctrl Pts',(1.36945139673063,-1.9364509217487,23.1942998497357));
#98381=CARTESIAN_POINT('Ctrl Pts',(1.36420323213931,-1.94015175804224,23.193869033298));
#98382=CARTESIAN_POINT('Ctrl Pts',(1.34867488510603,-1.9510076859209,23.1926021017682));
#98383=CARTESIAN_POINT('Ctrl Pts',(1.33835278269682,-1.95810285285008,23.1917699339177));
#98384=CARTESIAN_POINT('Ctrl Pts',(1.24980928761275,-2.01793825847819,23.184711871424));
#98385=CARTESIAN_POINT('Ctrl Pts',(1.16855119832032,-2.06605682919888,23.1787643262675));
#98386=CARTESIAN_POINT('Ctrl Pts',(0.915231919940702,-2.19632273165112,
23.1611027647524));
#98387=CARTESIAN_POINT('Ctrl Pts',(0.735962221065859,-2.26270697676572,
23.149696813605));
#98388=CARTESIAN_POINT('Ctrl Pts',(0.512459153630386,-2.31605868697322,
23.1351080087506));
#98389=CARTESIAN_POINT('Ctrl Pts',(0.474018113536081,-2.3242307950135,23.132589053918));
#98390=CARTESIAN_POINT('Ctrl Pts',(0.407184520227784,-2.33671186090213,
23.1281805119068));
#98391=CARTESIAN_POINT('Ctrl Pts',(0.37888341834952,-2.3414672308131,23.1263048000837));
#98392=CARTESIAN_POINT('Ctrl Pts',(0.33810451132477,-2.3475605596802,23.1235862868678));
#98393=CARTESIAN_POINT('Ctrl Pts',(0.325690758578103,-2.34931495579413,
23.1227566400809));
#98394=CARTESIAN_POINT('Ctrl Pts',(0.304063322917073,-2.35219678414945,
23.1213073311147));
#98395=CARTESIAN_POINT('Ctrl Pts',(0.294855764197943,-2.35336871097951,
23.120689087377));
#98396=CARTESIAN_POINT('Ctrl Pts',(0.277067360006177,-2.35552676517372,
23.1194922214471));
#98397=CARTESIAN_POINT('Ctrl Pts',(0.268487526841918,-2.35652012678393,
23.1189138380588));
#98398=CARTESIAN_POINT('Ctrl Pts',(0.24810858295146,-2.35876683502552,23.1175373485811));
#98399=CARTESIAN_POINT('Ctrl Pts',(0.236305209257145,-2.35997853593964,
23.1167379434654));
#98400=CARTESIAN_POINT('Ctrl Pts',(0.19433111571026,-2.36396943070917,23.1138872365677));
#98401=CARTESIAN_POINT('Ctrl Pts',(0.164117909635038,-2.36625890702768,
23.1118206834036));
#98402=CARTESIAN_POINT('Ctrl Pts',(-0.0980878242950857,-2.38108239777978,
23.0937516124217));
#98403=CARTESIAN_POINT('Ctrl Pts',(-0.330679545441945,-2.36003766890093,
23.0766282408757));
#98404=CARTESIAN_POINT('Ctrl Pts',(-0.63622140906218,-2.28629808097498,
23.0538243573354));
#98405=CARTESIAN_POINT('Ctrl Pts',(-0.714974303038032,-2.262907691939,23.0479377427313));
#98406=CARTESIAN_POINT('Ctrl Pts',(-0.808600170055024,-2.22972209040883,
23.0410447956196));
#98407=CARTESIAN_POINT('Ctrl Pts',(-0.824774876025817,-2.2237898468432,
23.0398579553041));
#98408=CARTESIAN_POINT('Ctrl Pts',(-0.847625396393234,-2.21512555599948,
23.0381883455427));
#98409=CARTESIAN_POINT('Ctrl Pts',(-0.854355125574872,-2.21253866956675,
23.0376975047563));
#98410=CARTESIAN_POINT('Ctrl Pts',(-0.865923846672474,-2.20803103616243,
23.0368553682762));
#98411=CARTESIAN_POINT('Ctrl Pts',(-0.870768469027594,-2.20612498296049,
23.0365032074034));
#98412=CARTESIAN_POINT('Ctrl Pts',(-0.880187721617931,-2.20238323924681,
23.0358195294535));
#98413=CARTESIAN_POINT('Ctrl Pts',(-0.884762917691652,-2.20054923562659,
23.03548790981));
#98414=CARTESIAN_POINT('Ctrl Pts',(-0.89723891413959,-2.19550293407542,
23.0345847989968));
#98415=CARTESIAN_POINT('Ctrl Pts',(-0.905128256577518,-2.19226222139023,
23.0340149964834));
#98416=CARTESIAN_POINT('Ctrl Pts',(-0.935425379984224,-2.17962560992005,
23.0318311420567));
#98417=CARTESIAN_POINT('Ctrl Pts',(-0.957706697006248,-2.16992774945174,
23.0302342369377));
#98418=CARTESIAN_POINT('Ctrl Pts',(-1.10952596273061,-2.10105475766969,
23.0193901951613));
#98419=CARTESIAN_POINT('Ctrl Pts',(-1.23367115596603,-2.03065141905409,
23.0106972654708));
#98420=CARTESIAN_POINT('Ctrl Pts',(-1.45025201314077,-1.88058969465217,
22.9945538038634));
#98421=CARTESIAN_POINT('Ctrl Pts',(-1.54431306600674,-1.80414594425563,
22.9871363762879));
#98422=CARTESIAN_POINT('Ctrl Pts',(-1.66243185636055,-1.69211791473719,
22.9768234468295));
#98423=CARTESIAN_POINT('Ctrl Pts',(-1.69197198302066,-1.66258028663596,
22.9741508527357));
#98424=CARTESIAN_POINT('Ctrl Pts',(-1.74141615722146,-1.61045724869729,
22.9694976456557));
#98425=CARTESIAN_POINT('Ctrl Pts',(-1.76169893987479,-1.58824415435028,
22.9675331496302));
#98426=CARTESIAN_POINT('Ctrl Pts',(-1.78998464783484,-1.55605789220829,
22.9647090306807));
#98427=CARTESIAN_POINT('Ctrl Pts',(-1.79833842227419,-1.54639584569376,
22.9638640485207));
#98428=CARTESIAN_POINT('Ctrl Pts',(-1.81265275057972,-1.52956691584467,
22.9623968248351));
#98429=CARTESIAN_POINT('Ctrl Pts',(-1.81864990748264,-1.52243142833548,
22.9617761055263));
#98430=CARTESIAN_POINT('Ctrl Pts',(-1.83008569475433,-1.50866099937072,
22.9605807535569));
#98431=CARTESIAN_POINT('Ctrl Pts',(-1.83553070207065,-1.50203152415951,
22.9600063939815));
#98432=CARTESIAN_POINT('Ctrl Pts',(-1.84827828351086,-1.48633809433353,
22.9586492901414));
#98433=CARTESIAN_POINT('Ctrl Pts',(-1.85555028249908,-1.47724970287719,
22.957865331527));
#98434=CARTESIAN_POINT('Ctrl Pts',(-1.88068091814271,-1.44536362410089,
22.9551214029163));
#98435=CARTESIAN_POINT('Ctrl Pts',(-1.89818804956177,-1.42229347198847,
22.9531476272808));
#98436=CARTESIAN_POINT('Ctrl Pts',(-2.00948440161574,-1.26991597792227,
22.9401792960293));
#98437=CARTESIAN_POINT('Ctrl Pts',(-2.09041149552327,-1.13175808072487,
22.928694572674));
#98438=CARTESIAN_POINT('Ctrl Pts',(-2.20565602922112,-0.879804962810913,
22.9084781713023));
#98439=CARTESIAN_POINT('Ctrl Pts',(-2.24649047860357,-0.769583192365358,
22.899862388963));
#98440=CARTESIAN_POINT('Ctrl Pts',(-2.28814372154299,-0.625049815125328,
22.8891408409844));
#98441=CARTESIAN_POINT('Ctrl Pts',(-2.29662663232989,-0.593123351541301,
22.8868080348292));
#98442=CARTESIAN_POINT('Ctrl Pts',(-2.30954187336032,-0.540073632223861,
22.8830010662205));
#98443=CARTESIAN_POINT('Ctrl Pts',(-2.31435761125718,-0.519049249499883,
22.8815100922245));
#98444=CARTESIAN_POINT('Ctrl Pts',(-2.32054047728001,-0.490257121677173,
22.8794951139561));
#98445=CARTESIAN_POINT('Ctrl Pts',(-2.32215648631423,-0.48254472291694,
22.8789579901675));
#98446=CARTESIAN_POINT('Ctrl Pts',(-2.32480186974153,-0.469598528107036,
22.8780609110371));
#98447=CARTESIAN_POINT('Ctrl Pts',(-2.32585206740307,-0.464369113407465,
22.8776997913014));
#98448=CARTESIAN_POINT('Ctrl Pts',(-2.32780948477424,-0.45444899555954,
22.8770171616387));
#98449=CARTESIAN_POINT('Ctrl Pts',(-2.32872018446531,-0.4497590360126,22.8766954497944));
#98450=CARTESIAN_POINT('Ctrl Pts',(-2.33106879238806,-0.437465685025876,
22.8758547620553));
#98451=CARTESIAN_POINT('Ctrl Pts',(-2.33248368798569,-0.429857871779538,
22.8753370848505));
#98452=CARTESIAN_POINT('Ctrl Pts',(-2.33726614076484,-0.403423856062453,
22.8735469120357));
#98453=CARTESIAN_POINT('Ctrl Pts',(-2.34044331634184,-0.384563338206025,
22.8722846497996));
#98454=CARTESIAN_POINT('Ctrl Pts',(-2.36215703217978,-0.245409601646564,
22.863068147003));
#98455=CARTESIAN_POINT('Ctrl Pts',(-2.37163990223934,-0.123870369466769,
22.8555429262571));
#98456=CARTESIAN_POINT('Ctrl Pts',(-2.37180149900125,0.0563807931440272,
22.8444766113764));
#98457=CARTESIAN_POINT('Ctrl Pts',(-2.36968900558597,0.114821446852761,
22.8409042704249));
#98458=CARTESIAN_POINT('Ctrl Pts',(-2.36542647205563,0.173077057400636,
22.8373161962119));
#98459=CARTESIAN_POINT('Ctrl Pts',(-2.36542649454112,0.173076750093424,
22.6375488994376));
#98460=CARTESIAN_POINT('Ctrl Pts',(-2.3661388636995,0.163340856160745,22.6381959253031));
#98461=CARTESIAN_POINT('Ctrl Pts',(-2.36679110884809,0.153600780959581,
22.6388448135099));
#98462=CARTESIAN_POINT('Ctrl Pts',(-2.3679525343904,0.134487787915918,22.640121361727));
#98463=CARTESIAN_POINT('Ctrl Pts',(-2.36846623843217,0.125115319822445,
22.6407488675116));
#98464=CARTESIAN_POINT('Ctrl Pts',(-2.36952546227323,0.103435541717451,
22.6422040098318));
#98465=CARTESIAN_POINT('Ctrl Pts',(-2.37003074984772,0.0911266286698586,
22.6430328907792));
#98466=CARTESIAN_POINT('Ctrl Pts',(-2.37132321985088,0.0522540697189382,
22.6456594248895));
#98467=CARTESIAN_POINT('Ctrl Pts',(-2.37175982230706,0.0256816243651149,
22.6474679495416));
#98468=CARTESIAN_POINT('Ctrl Pts',(-2.37170837929134,-0.111157339372951,
22.656852124219));
#98469=CARTESIAN_POINT('Ctrl Pts',(-2.36397757858074,-0.221269658741762,
22.6646497781992));
#98470=CARTESIAN_POINT('Ctrl Pts',(-2.32873649624718,-0.471753883068607,
22.6828981369618));
#98471=CARTESIAN_POINT('Ctrl Pts',(-2.29614003560575,-0.610986100626804,
22.6934256964943));
#98472=CARTESIAN_POINT('Ctrl Pts',(-2.24597325550628,-0.762286630255959,
22.7049314770699));
#98473=CARTESIAN_POINT('Ctrl Pts',(-2.24055185727853,-0.778077223748826,
22.70613279557));
#98474=CARTESIAN_POINT('Ctrl Pts',(-2.21540362821652,-0.848881851785801,
22.7115183105915));
#98475=CARTESIAN_POINT('Ctrl Pts',(-2.19381229719774,-0.903217889182414,
22.7156483952386));
#98476=CARTESIAN_POINT('Ctrl Pts',(-2.1660027905404,-0.966302214104502,
22.7203969108266));
#98477=CARTESIAN_POINT('Ctrl Pts',(-2.16170854119895,-0.975871021548873,
22.7211158765168));
#98478=CARTESIAN_POINT('Ctrl Pts',(-2.15461655288039,-0.991397439723287,
22.7222799812653));
#98479=CARTESIAN_POINT('Ctrl Pts',(-2.1518572991874,-0.997372317658715,
22.7227273468716));
#98480=CARTESIAN_POINT('Ctrl Pts',(-2.14687775890053,-1.00803813585572,
22.7235247580776));
#98481=CARTESIAN_POINT('Ctrl Pts',(-2.14466691964414,-1.01273333139938,
22.7238753666159));
#98482=CARTESIAN_POINT('Ctrl Pts',(-2.13981405161934,-1.02295228467462,
22.724637530639));
#98483=CARTESIAN_POINT('Ctrl Pts',(-2.13716604138198,-1.0284730749715,22.7250487112479));
#98484=CARTESIAN_POINT('Ctrl Pts',(-2.12959539288709,-1.04410148858156,
22.7262112241099));
#98485=CARTESIAN_POINT('Ctrl Pts',(-2.12462214292929,-1.05418462240831,
22.7269595041109));
#98486=CARTESIAN_POINT('Ctrl Pts',(-2.09176834746567,-1.1196178557757,22.7318064247401));
#98487=CARTESIAN_POINT('Ctrl Pts',(-2.06179635300671,-1.17389791441905,
22.7357854558786));
#98488=CARTESIAN_POINT('Ctrl Pts',(-1.92962405058496,-1.39254965414665,
22.7518980470798));
#98489=CARTESIAN_POINT('Ctrl Pts',(-1.80962582330238,-1.54528556569233,
22.7634144567564));
#98490=CARTESIAN_POINT('Ctrl Pts',(-1.61169767098765,-1.74211262704637,
22.7808843284437));
#98491=CARTESIAN_POINT('Ctrl Pts',(-1.54778221169918,-1.79913686973881,
22.7863349930808));
#98492=CARTESIAN_POINT('Ctrl Pts',(-1.46733189643567,-1.8634479410569,22.7930705632821));
#98493=CARTESIAN_POINT('Ctrl Pts',(-1.453615018906,-1.87416767485568,22.7942147383574));
#98494=CARTESIAN_POINT('Ctrl Pts',(-1.43072987914596,-1.89165002713215,
22.7961174369228));
#98495=CARTESIAN_POINT('Ctrl Pts',(-1.42162852477293,-1.89849944485158,
22.7968725331211));
#98496=CARTESIAN_POINT('Ctrl Pts',(-1.40504654413444,-1.91079246845791,
22.7982455690657));
#98497=CARTESIAN_POINT('Ctrl Pts',(-1.39758269100841,-1.9162584028048,22.7988626226279));
#98498=CARTESIAN_POINT('Ctrl Pts',(-1.38145863066075,-1.92792207393038,
22.8001936561382));
#98499=CARTESIAN_POINT('Ctrl Pts',(-1.37278830550615,-1.93410540902406,
22.8009081736812));
#98500=CARTESIAN_POINT('Ctrl Pts',(-1.34886939536106,-1.9509215742933,22.8028761909784));
#98501=CARTESIAN_POINT('Ctrl Pts',(-1.33353725531349,-1.9614336565659,22.8041342486639));
#98502=CARTESIAN_POINT('Ctrl Pts',(-1.24573399648598,-2.02012831633968,
22.8113210077753));
#98503=CARTESIAN_POINT('Ctrl Pts',(-1.17078646355645,-2.06446780823758,
22.8173910038987));
#98504=CARTESIAN_POINT('Ctrl Pts',(-0.88345515166124,-2.21377030927592,
22.8404355763361));
#98505=CARTESIAN_POINT('Ctrl Pts',(-0.658195280883046,-2.29085875111872,
22.8582198615693));
#98506=CARTESIAN_POINT('Ctrl Pts',(-0.401758654445174,-2.33759687660502,
22.8764464485488));
#98507=CARTESIAN_POINT('Ctrl Pts',(-0.37818344102016,-2.3415265468616,22.8781023300548));
#98508=CARTESIAN_POINT('Ctrl Pts',(-0.346080665181735,-2.34638011309947,
22.8803268281599));
#98509=CARTESIAN_POINT('Ctrl Pts',(-0.3376025417441,-2.34761495810114,22.8809114384758));
#98510=CARTESIAN_POINT('Ctrl Pts',(-0.3241821182491,-2.34949544699558,22.8818321221227));
#98511=CARTESIAN_POINT('Ctrl Pts',(-0.319244261086383,-2.35017148399574,
22.8821698649993));
#98512=CARTESIAN_POINT('Ctrl Pts',(-0.309057419870157,-2.35153345607968,
22.8828644990753));
#98513=CARTESIAN_POINT('Ctrl Pts',(-0.303808249316206,-2.35221738622069,
22.883221262447));
#98514=CARTESIAN_POINT('Ctrl Pts',(-0.29123005893677,-2.35381342942204,
22.8840734188807));
#98515=CARTESIAN_POINT('Ctrl Pts',(-0.283898904720153,-2.35470890416378,
22.8845678819676));
#98516=CARTESIAN_POINT('Ctrl Pts',(-0.258771760707469,-2.35765904026258,
22.8862554209968));
#98517=CARTESIAN_POINT('Ctrl Pts',(-0.240956196738947,-2.35954638298514,
22.8874395440333));
#98518=CARTESIAN_POINT('Ctrl Pts',(-0.135679794203057,-2.36949428514516,
22.8943729847273));
#98519=CARTESIAN_POINT('Ctrl Pts',(-0.0478372558555888,-2.37289429656389,
22.8998997604611));
#98520=CARTESIAN_POINT('Ctrl Pts',(0.051644136535442,-2.3712162609732,22.9060661745913));
#98521=CARTESIAN_POINT('Ctrl Pts',(0.0632861612777919,-2.37093410683426,
22.9067863514726));
#98522=CARTESIAN_POINT('Ctrl Pts',(0.2351799419568,-2.36550111571691,22.9174038103189));
#98523=CARTESIAN_POINT('Ctrl Pts',(0.394501062185377,-2.34419987827504,
22.9270726642322));
#98524=CARTESIAN_POINT('Ctrl Pts',(0.621114370105323,-2.29012927205432,
22.9417458010868));
#98525=CARTESIAN_POINT('Ctrl Pts',(0.690956141472397,-2.27003372628854,
22.9463955245219));
#98526=CARTESIAN_POINT('Ctrl Pts',(0.777004461513788,-2.24093584681048,
22.9523414489791));
#98527=CARTESIAN_POINT('Ctrl Pts',(0.794179880476881,-2.23490664001054,
22.9535392392594));
#98528=CARTESIAN_POINT('Ctrl Pts',(0.821309441411762,-2.22503094276704,
22.9554494729037));
#98529=CARTESIAN_POINT('Ctrl Pts',(0.831310189740711,-2.22131385826566,
22.956157610009));
#98530=CARTESIAN_POINT('Ctrl Pts',(0.849931612688952,-2.21424927081853,
22.957483751261));
#98531=CARTESIAN_POINT('Ctrl Pts',(0.858558479078264,-2.21091856778902,
22.9581011827082));
#98532=CARTESIAN_POINT('Ctrl Pts',(0.877738458997944,-2.20338428246305,
22.9594808563651));
#98533=CARTESIAN_POINT('Ctrl Pts',(0.888281238304005,-2.19915518608325,
22.9602439461024));
#98534=CARTESIAN_POINT('Ctrl Pts',(0.919106150079819,-2.18653235998805,
22.9624891652622));
#98535=CARTESIAN_POINT('Ctrl Pts',(0.939302151461556,-2.17793280154996,
22.9639782200499));
#98536=CARTESIAN_POINT('Ctrl Pts',(0.984824070776736,-2.15779840335284,
22.967376651177));
#98537=CARTESIAN_POINT('Ctrl Pts',(1.01007178846239,-2.14609581997832,22.9692915460008));
#98538=CARTESIAN_POINT('Ctrl Pts',(1.09270560182075,-2.10601299635434,22.9756602539608));
#98539=CARTESIAN_POINT('Ctrl Pts',(1.14914475580988,-2.07575561197449,22.9801750172605));
#98540=CARTESIAN_POINT('Ctrl Pts',(1.301593861362,-1.98590266102623,22.9928236833596));
#98541=CARTESIAN_POINT('Ctrl Pts',(1.39467316866816,-1.92167616410992,23.0010763570968));
#98542=CARTESIAN_POINT('Ctrl Pts',(1.53236254739288,-1.81137883728895,23.0139589192861));
#98543=CARTESIAN_POINT('Ctrl Pts',(1.58029781293401,-1.76971400626846,23.0185856431617));
#98544=CARTESIAN_POINT('Ctrl Pts',(1.67513625438375,-1.68035155469987,23.0279634723725));
#98545=CARTESIAN_POINT('Ctrl Pts',(1.7218145569077,-1.63248868752505,23.0327043849828));
#98546=CARTESIAN_POINT('Ctrl Pts',(1.77366953336858,-1.57461509120875,23.0380600509995));
#98547=CARTESIAN_POINT('Ctrl Pts',(1.78087013053637,-1.5664666892523,23.0388058424641));
#98548=CARTESIAN_POINT('Ctrl Pts',(1.79241427416385,-1.55322051723364,23.0400045267799));
#98549=CARTESIAN_POINT('Ctrl Pts',(1.79679261426107,-1.54815348383766,23.0404598644193));
#98550=CARTESIAN_POINT('Ctrl Pts',(1.80453127423543,-1.53912051542346,23.041265835484));
#98551=CARTESIAN_POINT('Ctrl Pts',(1.80790007389399,-1.53516201275571,23.0416170838312));
#98552=CARTESIAN_POINT('Ctrl Pts',(1.81515351357574,-1.52658187862291,23.0423741988551));
#98553=CARTESIAN_POINT('Ctrl Pts',(1.81903352728858,-1.52195648382285,23.0427797308518));
#98554=CARTESIAN_POINT('Ctrl Pts',(1.82983620864999,-1.50897819840385,23.0439104778261));
#98555=CARTESIAN_POINT('Ctrl Pts',(1.83671940122731,-1.50059241840012,23.0446328980133));
#98556=CARTESIAN_POINT('Ctrl Pts',(1.87758904784791,-1.45009846553379,23.0489360909865));
#98557=CARTESIAN_POINT('Ctrl Pts',(1.91018688171083,-1.4068807144998,23.0524260414535));
#98558=CARTESIAN_POINT('Ctrl Pts',(2.0167664384339,-1.25503602338574,23.0641874890026));
#98559=CARTESIAN_POINT('Ctrl Pts',(2.08319082677375,-1.14139544836367,23.072160228334));
#98560=CARTESIAN_POINT('Ctrl Pts',(2.20600687577525,-0.88445192073966,23.0896372626051));
#98561=CARTESIAN_POINT('Ctrl Pts',(2.25856243028706,-0.740005184954343,
23.099147283715));
#98562=CARTESIAN_POINT('Ctrl Pts',(2.30152987427224,-0.573164136774601,
23.1103949485897));
#98563=CARTESIAN_POINT('Ctrl Pts',(2.30603409105361,-0.554764478467687,
23.1116383491805));
#98564=CARTESIAN_POINT('Ctrl Pts',(2.31299847165395,-0.524763488289189,
23.1136715097836));
#98565=CARTESIAN_POINT('Ctrl Pts',(2.31559292944544,-0.513193944791641,
23.1144569604307));
#98566=CARTESIAN_POINT('Ctrl Pts',(2.32006592893637,-0.49252260039326,23.1158630122859));
#98567=CARTESIAN_POINT('Ctrl Pts',(2.32197794298424,-0.483428231052103,
23.1164825282888));
#98568=CARTESIAN_POINT('Ctrl Pts',(2.32590512007363,-0.464187928985814,
23.1177952509953));
#98569=CARTESIAN_POINT('Ctrl Pts',(2.32790744914565,-0.454039605463795,
23.1184888533661));
#98570=CARTESIAN_POINT('Ctrl Pts',(2.33306157058002,-0.426986501193547,
23.120341210399));
#98571=CARTESIAN_POINT('Ctrl Pts',(2.33609595765507,-0.410060256241769,
23.121503669563));
#98572=CARTESIAN_POINT('Ctrl Pts',(2.34998556372365,-0.327417674790233,
23.1271975520379));
#98573=CARTESIAN_POINT('Ctrl Pts',(2.35825226964407,-0.261302864185152,
23.1318097583441));
#98574=CARTESIAN_POINT('Ctrl Pts',(2.38523700274425,0.0659092742757167,
23.154933606839));
#98575=CARTESIAN_POINT('Ctrl Pts',(2.36342562879834,0.328453439871522,23.1746740265317));
#98576=CARTESIAN_POINT('Ctrl Pts',(2.29367009815016,0.603973795083269,23.1945198682148));
#98577=CARTESIAN_POINT('Ctrl Pts',(2.28782201771796,0.625761434976696,23.196081203516));
#98578=CARTESIAN_POINT('Ctrl Pts',(2.2793846736041,0.655494675196571,23.1981978466196));
#98579=CARTESIAN_POINT('Ctrl Pts',(2.27706319402351,0.663514110784612,23.198767317868));
#98580=CARTESIAN_POINT('Ctrl Pts',(2.27330028395333,0.676260526317819,23.1996700203236));
#98581=CARTESIAN_POINT('Ctrl Pts',(2.27188636956548,0.680995451827686,23.200004810821));
#98582=CARTESIAN_POINT('Ctrl Pts',(2.26891739398172,0.690825811960946,23.2006987143842));
#98583=CARTESIAN_POINT('Ctrl Pts',(2.26735995308383,0.695920460263877,23.2010576740294));
#98584=CARTESIAN_POINT('Ctrl Pts',(2.26355158155666,0.708229777020815,23.2019234582874));
#98585=CARTESIAN_POINT('Ctrl Pts',(2.2612832806096,0.715439101676275,23.2024292770499));
#98586=CARTESIAN_POINT('Ctrl Pts',(2.2532052127656,0.740691314226301,23.2041970169068));
#98587=CARTESIAN_POINT('Ctrl Pts',(2.24721345989887,0.758675870039446,23.2054488149318));
#98588=CARTESIAN_POINT('Ctrl Pts',(2.20873854471694,0.869703347499156,23.213143410879));
#98589=CARTESIAN_POINT('Ctrl Pts',(2.17069420490474,0.960729549417549,23.2193077067805));
#98590=CARTESIAN_POINT('Ctrl Pts',(2.05589304541637,1.19348587954897,23.2353293162124));
#98591=CARTESIAN_POINT('Ctrl Pts',(1.97018928140877,1.3302097032042,23.2450375354138));
#98592=CARTESIAN_POINT('Ctrl Pts',(1.82738695775039,1.51359291011812,23.2596859954296));
#98593=CARTESIAN_POINT('Ctrl Pts',(1.78095066126048,1.56796676292969,23.2642632475828));
#98594=CARTESIAN_POINT('Ctrl Pts',(1.71976458106991,1.63338168327896,23.2701271256744));
#98595=CARTESIAN_POINT('Ctrl Pts',(1.7072446132067,1.64646340321458,23.2713187500619));
#98596=CARTESIAN_POINT('Ctrl Pts',(1.68712430833667,1.66701022085875,23.2732215902467));
#98597=CARTESIAN_POINT('Ctrl Pts',(1.67962117627239,1.67456985705221,23.2739285632099));
#98598=CARTESIAN_POINT('Ctrl Pts',(1.66550375916694,1.68860325249131,23.2752540524203));
#98599=CARTESIAN_POINT('Ctrl Pts',(1.6589019836655,1.69508935473305,23.2758720066497));
#98600=CARTESIAN_POINT('Ctrl Pts',(1.64408532657908,1.70947694250957,23.2772548295635));
#98601=CARTESIAN_POINT('Ctrl Pts',(1.63585115201714,1.71735813929517,23.2780205598831));
#98602=CARTESIAN_POINT('Ctrl Pts',(1.6114709149086,1.74035882546914,23.2802799689226));
#98603=CARTESIAN_POINT('Ctrl Pts',(1.59517014812144,1.75531179328788,23.281780698244));
#98604=CARTESIAN_POINT('Ctrl Pts',(1.46829185996675,1.86847236195672,23.2933898910201));
#98605=CARTESIAN_POINT('Ctrl Pts',(1.34897650987916,1.95635309903308,23.3039255317526));
#98606=CARTESIAN_POINT('Ctrl Pts',(1.08402641862237,2.11568212167048,23.3264022948006));
#98607=CARTESIAN_POINT('Ctrl Pts',(0.937647520516158,2.18450126199222,23.3383270637343));
#98608=CARTESIAN_POINT('Ctrl Pts',(0.756555337324953,2.24805633352086,23.3518289938383));
#98609=CARTESIAN_POINT('Ctrl Pts',(0.727504923768372,2.25762487272788,23.3539574342134));
#98610=CARTESIAN_POINT('Ctrl Pts',(0.689286805912397,2.26939865034461,23.3567017039674));
#98611=CARTESIAN_POINT('Ctrl Pts',(0.680281129544448,2.27211446175078,23.3573443424587));
#98612=CARTESIAN_POINT('Ctrl Pts',(0.665773173933974,2.27639558563376,23.3583729052043));
#98613=CARTESIAN_POINT('Ctrl Pts',(0.660281089432748,2.27799465893488,23.3587607332911));
#98614=CARTESIAN_POINT('Ctrl Pts',(0.649713515610885,2.28103008142851,23.3595039401175));
#98615=CARTESIAN_POINT('Ctrl Pts',(0.644638992526011,2.28246937648357,23.3598594777554));
#98616=CARTESIAN_POINT('Ctrl Pts',(0.632538188190395,2.28585797241889,23.3607041655991));
#98617=CARTESIAN_POINT('Ctrl Pts',(0.625507570527957,2.28779184200947,23.3611924258191));
#98618=CARTESIAN_POINT('Ctrl Pts',(0.601692673283296,2.29422447323487,23.3628381973648));
#98619=CARTESIAN_POINT('Ctrl Pts',(0.584867416428193,2.29857132928951,23.3639873272444));
#98620=CARTESIAN_POINT('Ctrl Pts',(0.487748591326862,2.32252679233712,23.370550327774));
#98621=CARTESIAN_POINT('Ctrl Pts',(0.406512658223501,2.33811460863067,23.3757664584904));
#98622=CARTESIAN_POINT('Ctrl Pts',(0.157871084295467,2.37246936447168,23.3913570572604));
#98623=CARTESIAN_POINT('Ctrl Pts',(-0.0108546185834055,2.3776917500096,
23.4014623286112));
#98624=CARTESIAN_POINT('Ctrl Pts',(-0.2597617503961,2.35888280122194,23.4171148508039));
#98625=CARTESIAN_POINT('Ctrl Pts',(-0.340432658189673,2.34859694853301,
23.4222988470915));
#98626=CARTESIAN_POINT('Ctrl Pts',(-0.43892269547475,2.33085794224683,23.4288450967247));
#98627=CARTESIAN_POINT('Ctrl Pts',(-0.457394077275822,2.32730369824493,
23.4300822092254));
#98628=CARTESIAN_POINT('Ctrl Pts',(-0.486403256315172,2.32136309515186,
23.4320407686154));
#98629=CARTESIAN_POINT('Ctrl Pts',(-0.496970633158464,2.31912374195317,
23.4327575184811));
#98630=CARTESIAN_POINT('Ctrl Pts',(-0.516452998849367,2.31485592405895,
23.4340851936952));
#98631=CARTESIAN_POINT('Ctrl Pts',(-0.525372304277465,2.31284793858812,
23.4346954513427));
#98632=CARTESIAN_POINT('Ctrl Pts',(-0.54512965951049,2.30827982106654,23.4360527481966));
#98633=CARTESIAN_POINT('Ctrl Pts',(-0.555961681239863,2.30569483662775,
23.4368005750237));
#98634=CARTESIAN_POINT('Ctrl Pts',(-0.587071131271974,2.29803882334521,
23.4389591637181));
#98635=CARTESIAN_POINT('Ctrl Pts',(-0.607299819618479,2.29277600889447,
23.4403760740188));
#98636=CARTESIAN_POINT('Ctrl Pts',(-0.786544220108168,2.24360425477636,
23.4530532963383));
#98637=CARTESIAN_POINT('Ctrl Pts',(-0.940613108902813,2.18349226559486,
23.4648569039047));
#98638=CARTESIAN_POINT('Ctrl Pts',(-1.23183282770601,2.033292702644,23.4887415972583));
#98639=CARTESIAN_POINT('Ctrl Pts',(-1.36843905867133,1.94398414650229,23.500745819513));
#98640=CARTESIAN_POINT('Ctrl Pts',(-1.50871661848653,1.83010715544336,23.5132995216918));
#98641=CARTESIAN_POINT('Ctrl Pts',(-1.52247689346887,1.81867594488152,23.5145332291178));
#98642=CARTESIAN_POINT('Ctrl Pts',(-1.54132792955243,1.80265172169718,23.5162249969383));
#98643=CARTESIAN_POINT('Ctrl Pts',(-1.54652965642546,1.79819104683339,23.5166919958253));
#98644=CARTESIAN_POINT('Ctrl Pts',(-1.55542566550005,1.79049523127157,23.5174908509254));
#98645=CARTESIAN_POINT('Ctrl Pts',(-1.55912932943563,1.7872710788591,23.5178234949254));
#98646=CARTESIAN_POINT('Ctrl Pts',(-1.56651620959089,1.78080013881076,23.5184870148891));
#98647=CARTESIAN_POINT('Ctrl Pts',(-1.57019938452929,1.77755339236576,23.5188178825288));
#98648=CARTESIAN_POINT('Ctrl Pts',(-1.57925866939608,1.76951743585439,23.5196318455953));
#98649=CARTESIAN_POINT('Ctrl Pts',(-1.58462316563945,1.76471508380249,23.5201139677787));
#98650=CARTESIAN_POINT('Ctrl Pts',(-1.60225894344346,1.748782093305,23.5216997067464));
#98651=CARTESIAN_POINT('Ctrl Pts',(-1.61443581111957,1.7375470012838,23.5227958305708));
#98652=CARTESIAN_POINT('Ctrl Pts',(-1.64368904090397,1.70998320147671,23.5254350843012));
#98653=CARTESIAN_POINT('Ctrl Pts',(-1.66064140238457,1.69352485640265,23.5269695964148));
#98654=CARTESIAN_POINT('Ctrl Pts',(-1.72445087527935,1.62969519827923,23.5327785894735));
#98655=CARTESIAN_POINT('Ctrl Pts',(-1.76955331795264,1.58060737595379,23.5369547406256));
#98656=CARTESIAN_POINT('Ctrl Pts',(-1.84856984134563,1.48698008886257,23.5445453325266));
#98657=CARTESIAN_POINT('Ctrl Pts',(-1.8830884051977,1.44301717751472,23.5479713848785));
#98658=CARTESIAN_POINT('Ctrl Pts',(-2.01661899165418,1.25999110305726,23.5618550429729));
#98659=CARTESIAN_POINT('Ctrl Pts',(-2.10202537335978,1.11166987272222,23.5722988597832));
#98660=CARTESIAN_POINT('Ctrl Pts',(-2.18240899964653,0.929044186277643,
23.5852288000051));
#98661=CARTESIAN_POINT('Ctrl Pts',(-2.19355948442685,0.902401690823416,
23.5871153699846));
#98662=CARTESIAN_POINT('Ctrl Pts',(-2.20854914650283,0.864665386103283,
23.5897909809212));
#98663=CARTESIAN_POINT('Ctrl Pts',(-2.21279702455577,0.853735838678894,
23.5905663159395));
#98664=CARTESIAN_POINT('Ctrl Pts',(-2.22005027253388,0.834655800507353,
23.591920746519));
#98665=CARTESIAN_POINT('Ctrl Pts',(-2.22309226170503,0.826519395060308,
23.5924986079923));
#98666=CARTESIAN_POINT('Ctrl Pts',(-2.22936101663033,0.809467367280539,
23.5937103580647));
#98667=CARTESIAN_POINT('Ctrl Pts',(-2.2325791465368,0.80054875622889,23.5943445217906));
#98668=CARTESIAN_POINT('Ctrl Pts',(-2.24010736825965,0.779286836110114,
23.5958574127246));
#98669=CARTESIAN_POINT('Ctrl Pts',(-2.24436900536133,0.766926821878375,
23.5967377258283));
#98670=CARTESIAN_POINT('Ctrl Pts',(-2.25845288549978,0.724956456675117,
23.5997301811685));
#98671=CARTESIAN_POINT('Ctrl Pts',(-2.26779266929493,0.695188857372109,
23.6018580307696));
#98672=CARTESIAN_POINT('Ctrl Pts',(-2.32348697165967,0.504597316193869,
23.61552282045));
#98673=CARTESIAN_POINT('Ctrl Pts',(-2.35324136537112,0.339609969413825,
23.6275853298065));
#98674=CARTESIAN_POINT('Ctrl Pts',(-2.36542649498009,0.173076744094113,
23.6397760267629));
#98675=CARTESIAN_POINT('Origin',(0.,0.,0.));
#98676=CARTESIAN_POINT('',(-2.94561598299575,0.00187102060485729,0.322176117089595));
#98677=CARTESIAN_POINT('',(1.2910272435207,2.64899789736804,5.96387826521875E-5));
#98678=CARTESIAN_POINT('Ctrl Pts',(-2.94561598299575,0.00187102060485729,
0.322176117089595));
#98679=CARTESIAN_POINT('Ctrl Pts',(-2.94627700058788,0.099138654117573,
0.316895328369764));
#98680=CARTESIAN_POINT('Ctrl Pts',(-2.8977661387304,1.17124645315207,0.258650561155306));
#98681=CARTESIAN_POINT('Ctrl Pts',(-1.62977873101038,3.0288441099736,0.151278401719662));
#98682=CARTESIAN_POINT('Ctrl Pts',(0.47570852676496,3.04092581158969,0.0491870310038447));
#98683=CARTESIAN_POINT('Ctrl Pts',(1.29102724352071,2.64899789736804,5.96387826521875E-5));
#98684=CARTESIAN_POINT('',(-1.28892185405319,2.64462557919719,0.));
#98685=CARTESIAN_POINT('Origin',(0.,0.,0.));
#98686=CARTESIAN_POINT('',(-2.94199832420209,0.00314012613217853,0.177823882943095));
#98687=CARTESIAN_POINT('Ctrl Pts',(-1.28892185405319,2.64462557919719,-1.94289029309402E-15));
#98688=CARTESIAN_POINT('Ctrl Pts',(-1.37483881637629,2.60275188212522,0.00517052748665724));
#98689=CARTESIAN_POINT('Ctrl Pts',(-1.45877171164705,2.55665900158965,0.0103410549733164));
#98690=CARTESIAN_POINT('Ctrl Pts',(-1.54029698572466,2.50656122920776,0.0155115824599756));
#98691=CARTESIAN_POINT('Ctrl Pts',(-1.6217746032091,2.45649274208967,0.0206790874517372));
#98692=CARTESIAN_POINT('Ctrl Pts',(-1.70084704886668,2.40242423989201,0.0258465924434988));
#98693=CARTESIAN_POINT('Ctrl Pts',(-1.77711654308791,2.3446152759639,0.0310140974352603));
#98694=CARTESIAN_POINT('Ctrl Pts',(-1.85580329515119,2.28497413558277,0.0363453794664889));
#98695=CARTESIAN_POINT('Ctrl Pts',(-1.93150605636844,2.22135170164654,0.0416766614977175));
#98696=CARTESIAN_POINT('Ctrl Pts',(-2.00382190342501,2.15408026297865,0.0470079435289461));
#98697=CARTESIAN_POINT('Ctrl Pts',(-2.07390541239702,2.08888544514359,0.0521746527258335));
#98698=CARTESIAN_POINT('Ctrl Pts',(-2.14080775230235,2.0202639299885,0.0573413619227208));
#98699=CARTESIAN_POINT('Ctrl Pts',(-2.20419800366129,1.94855719973923,0.0625080711196082));
#98700=CARTESIAN_POINT('Ctrl Pts',(-2.26759963803479,1.87683759308174,0.0676757081046758));
#98701=CARTESIAN_POINT('Ctrl Pts',(-2.32748765382612,1.8020319790956,0.0728433450897433));
#98702=CARTESIAN_POINT('Ctrl Pts',(-2.38357059315908,1.72451594003282,0.0780109820748108));
#98703=CARTESIAN_POINT('Ctrl Pts',(-2.43967598230067,1.64696887156495,0.0831806876472737));
#98704=CARTESIAN_POINT('Ctrl Pts',(-2.49197302046287,1.5667095543312,0.0883503932197366));
#98705=CARTESIAN_POINT('Ctrl Pts',(-2.54021329705219,1.48414298687129,0.0935200987921995));
#98706=CARTESIAN_POINT('Ctrl Pts',(-2.58848353796475,1.4015251334012,0.0986930155139297));
#98707=CARTESIAN_POINT('Ctrl Pts',(-2.63269179296663,1.31659753470971,0.10386593223566));
#98708=CARTESIAN_POINT('Ctrl Pts',(-2.67263571909581,1.22978954013002,0.10903884895739));
#98709=CARTESIAN_POINT('Ctrl Pts',(-2.71263977449153,1.14285086983691,0.114219552687521));
#98710=CARTESIAN_POINT('Ctrl Pts',(-2.74836651135852,1.05402652900781,0.119400256417653));
#98711=CARTESIAN_POINT('Ctrl Pts',(-2.7796617792108,0.963765735640482,0.124580960147784));
#98712=CARTESIAN_POINT('Ctrl Pts',(-2.81098456103485,0.873425587370955,
0.129766218615609));
#98713=CARTESIAN_POINT('Ctrl Pts',(-2.83786799345476,0.781646866830215,
0.134951477083434));
#98714=CARTESIAN_POINT('Ctrl Pts',(-2.86020837059367,0.688891919524305,
0.140136735551259));
#98715=CARTESIAN_POINT('Ctrl Pts',(-2.88258671205671,0.595979348250766,
0.145330805635463));
#98716=CARTESIAN_POINT('Ctrl Pts',(-2.90040650544948,0.502087643872117,
0.150524875719667));
#98717=CARTESIAN_POINT('Ctrl Pts',(-2.91361546104576,0.407687312968051,
0.155718945803871));
#98718=CARTESIAN_POINT('Ctrl Pts',(-2.91636701024738,0.388022839631122,
0.156800919264163));
#98719=CARTESIAN_POINT('Ctrl Pts',(-2.91891866257042,0.368336303150983,
0.157882892724454));
#98720=CARTESIAN_POINT('Ctrl Pts',(-2.92127022970174,0.348631962187004,
0.158964866184746));
#98721=CARTESIAN_POINT('Ctrl Pts',(-2.93493299361991,0.234148409849401,
0.165251205093298));
#98722=CARTESIAN_POINT('Ctrl Pts',(-2.94187489336978,0.118783007009487,
0.171537544001849));
#98723=CARTESIAN_POINT('Ctrl Pts',(-2.94199832420144,0.00314012673363615,
0.1778238829104));
#98724=CARTESIAN_POINT('',(-2.94185727375763,0.00142673463472898,1.1778238505128));
#98725=CARTESIAN_POINT('Ctrl Pts',(-2.94199832420208,0.00314012613217657,
0.177823882943095));
#98726=CARTESIAN_POINT('Ctrl Pts',(-2.94209516594599,-0.0875913401540299,
0.182756039124081));
#98727=CARTESIAN_POINT('Ctrl Pts',(-2.93799066139926,-0.178517496165705,
0.187688195305066));
#98728=CARTESIAN_POINT('Ctrl Pts',(-2.92965745352971,-0.269204764032533,
0.192620351486051));
#98729=CARTESIAN_POINT('Ctrl Pts',(-2.92133503561485,-0.359774608750091,
0.19754612144188));
#98730=CARTESIAN_POINT('Ctrl Pts',(-2.90879482451379,-0.450105719668528,
0.202471891397708));
#98731=CARTESIAN_POINT('Ctrl Pts',(-2.89206147248208,-0.539763317931814,
0.207397661353537));
#98732=CARTESIAN_POINT('Ctrl Pts',(-2.87534435746252,-0.629333917994769,
0.212318651646183));
#98733=CARTESIAN_POINT('Ctrl Pts',(-2.85444226635288,-0.718231847586187,
0.21723964193883));
#98734=CARTESIAN_POINT('Ctrl Pts',(-2.82943163687848,-0.806027674606241,
0.222160632231477));
#98735=CARTESIAN_POINT('Ctrl Pts',(-2.80443376779796,-0.893778708298135,
0.227079111840637));
#98736=CARTESIAN_POINT('Ctrl Pts',(-2.77533164599731,-0.98042830775922,
0.231997591449797));
#98737=CARTESIAN_POINT('Ctrl Pts',(-2.74225248475926,-1.06555868436782,
0.236916071058958));
#98738=CARTESIAN_POINT('Ctrl Pts',(-2.70918004756733,-1.15067175640891,
0.241833550882074));
#98739=CARTESIAN_POINT('Ctrl Pts',(-2.67213234464307,-1.23426578455603,
0.24675103070519));
#98740=CARTESIAN_POINT('Ctrl Pts',(-2.63128551283259,-1.31594093710824,
0.251668510528306));
#98741=CARTESIAN_POINT('Ctrl Pts',(-2.59043444759753,-1.39762455459111,
0.256586500006127));
#98742=CARTESIAN_POINT('Ctrl Pts',(-2.54578368257135,-1.47738848615293,
0.261504489483948));
#98743=CARTESIAN_POINT('Ctrl Pts',(-2.49755562285416,-1.55485687789893,
0.266422478961768));
#98744=CARTESIAN_POINT('Ctrl Pts',(-2.44927774207178,-1.63240529687009,
0.271345548873588));
#98745=CARTESIAN_POINT('Ctrl Pts',(-2.39741543999569,-1.70765304858344,
0.276268618785408));
#98746=CARTESIAN_POINT('Ctrl Pts',(-2.3422344852868,-1.78025324488773,0.281191688697228));
#98747=CARTESIAN_POINT('Ctrl Pts',(-2.2870215635897,-1.85289549935559,0.286117610602433));
#98748=CARTESIAN_POINT('Ctrl Pts',(-2.22848646666738,-1.92288679334015,
0.291043532507638));
#98749=CARTESIAN_POINT('Ctrl Pts',(-2.1669336730891,-1.98991518825114,0.295969454412843));
#98750=CARTESIAN_POINT('Ctrl Pts',(-2.10528114624034,-2.05705218848532,
0.300903357731614));
#98751=CARTESIAN_POINT('Ctrl Pts',(-2.04060149944086,-2.12121638682871,
0.305837261050386));
#98752=CARTESIAN_POINT('Ctrl Pts',(-1.9732338943125,-2.18213473423076,0.310771164369158));
#98753=CARTESIAN_POINT('Ctrl Pts',(-1.94065282200704,-2.2115967446088,0.313157353702603));
#98754=CARTESIAN_POINT('Ctrl Pts',(-1.90744349998323,-2.24030018420665,
0.315543543036049));
#98755=CARTESIAN_POINT('Ctrl Pts',(-1.87364667060443,-2.26821783648152,
0.317929732369494));
#98756=CARTESIAN_POINT('Ctrl Pts',(-1.80198568799447,-2.3274129275878,0.322989280128001));
#98757=CARTESIAN_POINT('Ctrl Pts',(-1.72739011311397,-2.3833132220152,0.328048827886508));
#98758=CARTESIAN_POINT('Ctrl Pts',(-1.65019520011135,-2.43561487134758,
0.333108375645015));
#98759=CARTESIAN_POINT('Ctrl Pts',(-1.57310658002327,-2.48784450434459,
0.338160956699932));
#98760=CARTESIAN_POINT('Ctrl Pts',(-1.49342609802247,-2.53648509324391,
0.343213537754849));
#98761=CARTESIAN_POINT('Ctrl Pts',(-1.4115224133712,-2.58127264669014,0.348266118809766));
#98762=CARTESIAN_POINT('Ctrl Pts',(-1.32970640747573,-2.62601225458939,
0.353313291023526));
#98763=CARTESIAN_POINT('Ctrl Pts',(-1.24567231625463,-2.66690681484048,
0.358360463237286));
#98764=CARTESIAN_POINT('Ctrl Pts',(-1.15981723600913,-2.7037359299784,0.363407635451046));
#98765=CARTESIAN_POINT('Ctrl Pts',(-1.07402472071201,-2.74053820673143,
0.368451129652182));
#98766=CARTESIAN_POINT('Ctrl Pts',(-0.986414260068643,-2.77328075361311,
0.373494623853317));
#98767=CARTESIAN_POINT('Ctrl Pts',(-0.89740604689479,-2.80178985418191,
0.378538118054452));
#98768=CARTESIAN_POINT('Ctrl Pts',(-0.808430709768861,-2.83028842463755,
0.383579749392024));
#98769=CARTESIAN_POINT('Ctrl Pts',(-0.718059067082031,-2.85455652055424,
0.388621380729597));
#98770=CARTESIAN_POINT('Ctrl Pts',(-0.626728759781356,-2.87446952700197,
0.39366301206717));
#98771=CARTESIAN_POINT('Ctrl Pts',(-0.535406845971985,-2.89438070339294,
0.398704180065792));
#98772=CARTESIAN_POINT('Ctrl Pts',(-0.443126875368464,-2.90993749200716,
0.403745348064413));
#98773=CARTESIAN_POINT('Ctrl Pts',(-0.350337929466291,-2.92106612988773,
0.408786516063035));
#98774=CARTESIAN_POINT('Ctrl Pts',(-0.257531766689741,-2.93219683267332,
0.413828619444156));
#98775=CARTESIAN_POINT('Ctrl Pts',(-0.16421688069103,-2.93889770053683,
0.418870722825277));
#98776=CARTESIAN_POINT('Ctrl Pts',(-0.0708476160087499,-2.94114681974666,
0.423912826206398));
#98777=CARTESIAN_POINT('Ctrl Pts',(0.0226219382875447,-2.94339835477607,
0.428960345401852));
#98778=CARTESIAN_POINT('Ctrl Pts',(0.116145544535804,-2.94118858532501,
0.434007864597306));
#98779=CARTESIAN_POINT('Ctrl Pts',(0.209269017545923,-2.93454774680791,
0.43905538379276));
#98780=CARTESIAN_POINT('Ctrl Pts',(0.302448533360736,-2.92790291175583,
0.444105940644815));
#98781=CARTESIAN_POINT('Ctrl Pts',(0.395226997086348,-2.91682175051154,
0.449156497496869));
#98782=CARTESIAN_POINT('Ctrl Pts',(0.48715764938872,-2.90138612126033,0.454207054348924));
#98783=CARTESIAN_POINT('Ctrl Pts',(0.579234252341123,-2.88592598614446,
0.459265629549996));
#98784=CARTESIAN_POINT('Ctrl Pts',(0.670459924425042,-2.86609767494053,
0.464324204751068));
#98785=CARTESIAN_POINT('Ctrl Pts',(0.76040053390516,-2.84203360783027,0.46938277995214));
#98786=CARTESIAN_POINT('Ctrl Pts',(0.804920154320144,-2.83012215715652,
0.471886719486174));
#98787=CARTESIAN_POINT('Ctrl Pts',(0.849125183726759,-2.81717364719446,
0.474390659020208));
#98788=CARTESIAN_POINT('Ctrl Pts',(0.892964786050042,-2.8032084993583,0.476894598554242));
#98789=CARTESIAN_POINT('Ctrl Pts',(0.981572334246543,-2.77498247894782,
0.48195550082491));
#98790=CARTESIAN_POINT('Ctrl Pts',(1.06899313626838,-2.74250241713219,0.487016403095577));
#98791=CARTESIAN_POINT('Ctrl Pts',(1.15479018409174,-2.70588684736176,0.492077305366244));
#98792=CARTESIAN_POINT('Ctrl Pts',(1.24047196846654,-2.66932046852446,0.497131408602873));
#98793=CARTESIAN_POINT('Ctrl Pts',(1.32453393024678,-2.62862979536122,0.502185511839503));
#98794=CARTESIAN_POINT('Ctrl Pts',(1.40655463318329,-2.58398298443906,0.507239615076133));
#98795=CARTESIAN_POINT('Ctrl Pts',(1.48849023387733,-2.53938249772035,0.512288474325528));
#98796=CARTESIAN_POINT('Ctrl Pts',(1.5683883992688,-2.49083424348688,0.517337333574923));
#98797=CARTESIAN_POINT('Ctrl Pts',(1.64584908580887,-2.43855383101176,0.522386192824318));
#98798=CARTESIAN_POINT('Ctrl Pts',(1.72325702242345,-2.3863090209562,0.527431613852841));
#98799=CARTESIAN_POINT('Ctrl Pts',(1.79823041370787,-2.33033735128013,0.532477034881364));
#98800=CARTESIAN_POINT('Ctrl Pts',(1.87039606650381,-2.27089906301603,0.537522455909887));
#98801=CARTESIAN_POINT('Ctrl Pts',(1.94253719679688,-2.21148097238804,0.542566162461414));
#98802=CARTESIAN_POINT('Ctrl Pts',(2.01187214297372,-2.14859888467587,0.547609869012941));
#98803=CARTESIAN_POINT('Ctrl Pts',(2.07805966309663,-2.08255420976519,0.552653575564468));
#98804=CARTESIAN_POINT('Ctrl Pts',(2.14424302411208,-2.01651368498582,0.557696965178338));
#98805=CARTESIAN_POINT('Ctrl Pts',(2.2072790393132,-1.94731128091343,0.562740354792208));
#98806=CARTESIAN_POINT('Ctrl Pts',(2.26686312716272,-1.87528546165911,0.567783744406077));
#98807=CARTESIAN_POINT('Ctrl Pts',(2.32645997354199,-1.80324421977117,0.572828213943106));
#98808=CARTESIAN_POINT('Ctrl Pts',(2.38260314260021,-1.72837870293375,0.577872683480135));
#98809=CARTESIAN_POINT('Ctrl Pts',(2.4350288801728,-1.65105976655129,0.582917153017164));
#98810=CARTESIAN_POINT('Ctrl Pts',(2.48751304877621,-1.57365465445888,0.5879672448605));
#98811=CARTESIAN_POINT('Ctrl Pts',(2.53627126673176,-1.49379103128267,0.593017336703836));
#98812=CARTESIAN_POINT('Ctrl Pts',(2.581083772037,-1.41186775645854,0.598067428547172));
#98813=CARTESIAN_POINT('Ctrl Pts',(2.6259243092101,-1.32989323561727,0.603120679408428));
#98814=CARTESIAN_POINT('Ctrl Pts',(2.66681402620945,-1.24585689555878,0.608173930269683));
#98815=CARTESIAN_POINT('Ctrl Pts',(2.70358063846019,-1.1601791807058,0.613227181130939));
#98816=CARTESIAN_POINT('Ctrl Pts',(2.74040678082037,-1.07436274206433,0.618288613887625));
#98817=CARTESIAN_POINT('Ctrl Pts',(2.77309633592506,-0.986900036885405,
0.623350046644311));
#98818=CARTESIAN_POINT('Ctrl Pts',(2.80152640179825,-0.898228155886535,
0.628411479400998));
#98819=CARTESIAN_POINT('Ctrl Pts',(2.81547151207044,-0.854734089988602,
0.630894141180328));
#98820=CARTESIAN_POINT('Ctrl Pts',(2.82839258253587,-0.810949283268288,
0.633376802959659));
#98821=CARTESIAN_POINT('Ctrl Pts',(2.84027962227694,-0.766926115918837,
0.63585946473899));
#98822=CARTESIAN_POINT('Ctrl Pts',(2.86443637764123,-0.677462556682363,
0.640904711878893));
#98823=CARTESIAN_POINT('Ctrl Pts',(2.88440660936451,-0.586691594128352,
0.645949959018796));
#98824=CARTESIAN_POINT('Ctrl Pts',(2.90005137898637,-0.495041411640717,
0.6509952061587));
#98825=CARTESIAN_POINT('Ctrl Pts',(2.91567424617995,-0.403519537948771,
0.656033390032967));
#98826=CARTESIAN_POINT('Ctrl Pts',(2.92698360909852,-0.311121325401966,
0.661071573907234));
#98827=CARTESIAN_POINT('Ctrl Pts',(2.93389056820814,-0.218289105956563,
0.666109757781502));
#98828=CARTESIAN_POINT('Ctrl Pts',(2.94079000852528,-0.12555794200929,0.671142457178675));
#98829=CARTESIAN_POINT('Ctrl Pts',(2.94329653689728,-0.032394152113643,
0.67617515657585));
#98830=CARTESIAN_POINT('Ctrl Pts',(2.94137267422002,0.060751883524479,0.681207855973023));
#98831=CARTESIAN_POINT('Ctrl Pts',(2.93945023702623,0.153828902732275,0.686236826398321));
#98832=CARTESIAN_POINT('Ctrl Pts',(2.93310394246262,0.246887749584014,0.691265796823618));
#98833=CARTESIAN_POINT('Ctrl Pts',(2.92234835876399,0.339476170046479,0.696294767248916));
#98834=CARTESIAN_POINT('Ctrl Pts',(2.91159681473904,0.432029815361808,0.70132184885069));
#98835=CARTESIAN_POINT('Ctrl Pts',(2.8964393226185,0.524112943032413,0.706348930452465));
#98836=CARTESIAN_POINT('Ctrl Pts',(2.87694238148067,0.615277606971287,0.71137601205424));
#98837=CARTESIAN_POINT('Ctrl Pts',(2.85744726700986,0.706433729699323,0.7164026226691));
#98838=CARTESIAN_POINT('Ctrl Pts',(2.83361360512464,0.796671123973326,0.721429233283959));
#98839=CARTESIAN_POINT('Ctrl Pts',(2.80555894103354,0.885552386020586,0.726455843898819));
#98840=CARTESIAN_POINT('Ctrl Pts',(2.77749899685084,0.974450376167096,0.731483400558315));
#98841=CARTESIAN_POINT('Ctrl Pts',(2.7452166074292,1.06199130236983,0.736510957217811));
#98842=CARTESIAN_POINT('Ctrl Pts',(2.70887871331399,1.14775437988898,0.741538513877307));
#98843=CARTESIAN_POINT('Ctrl Pts',(2.67250091164686,1.23361164543283,0.746571591976152));
#98844=CARTESIAN_POINT('Ctrl Pts',(2.63205888894935,1.31768675387426,0.751604670074996));
#98845=CARTESIAN_POINT('Ctrl Pts',(2.58776700753775,1.39958062100728,0.75663774817384));
#98846=CARTESIAN_POINT('Ctrl Pts',(2.54344805401219,1.48152454336561,0.761673902594112));
#98847=CARTESIAN_POINT('Ctrl Pts',(2.49527478783876,1.56128418925326,0.766710057014383));
#98848=CARTESIAN_POINT('Ctrl Pts',(2.44350547838044,1.63848862587592,0.771746211434655));
#98849=CARTESIAN_POINT('Ctrl Pts',(2.39165167247806,1.71581907345813,0.776790585727756));
#98850=CARTESIAN_POINT('Ctrl Pts',(2.33619037114104,1.79058562837981,0.781834960020858));
#98851=CARTESIAN_POINT('Ctrl Pts',(2.27742062830142,1.86244980651485,0.78687933431396));
#98852=CARTESIAN_POINT('Ctrl Pts',(2.24656609739313,1.90017900862343,0.789527666517219));
#98853=CARTESIAN_POINT('Ctrl Pts',(2.21480028320741,1.93710882306337,0.792175998720478));
#98854=CARTESIAN_POINT('Ctrl Pts',(2.18217036558718,1.97319449004732,0.794824330923737));
#98855=CARTESIAN_POINT('Ctrl Pts',(2.11990642314893,2.04205264402996,0.79987784058258));
#98856=CARTESIAN_POINT('Ctrl Pts',(2.05426861974718,2.10808406357649,0.804931350241422));
#98857=CARTESIAN_POINT('Ctrl Pts',(1.98554367777261,2.17093995855648,0.809984859900264));
#98858=CARTESIAN_POINT('Ctrl Pts',(1.91691347614877,2.23370920392478,0.815031403074105));
#98859=CARTESIAN_POINT('Ctrl Pts',(1.84520491759781,2.29331132661815,0.820077946247946));
#98860=CARTESIAN_POINT('Ctrl Pts',(1.77074359213942,2.34943208688764,0.825124489421787));
#98861=CARTESIAN_POINT('Ctrl Pts',(1.69636193878188,2.40549279908727,0.830165632897272));
#98862=CARTESIAN_POINT('Ctrl Pts',(1.61923372570595,2.45807928711824,0.835206776372757));
#98863=CARTESIAN_POINT('Ctrl Pts',(1.53971902963432,2.50691629492928,0.840247919848242));
#98864=CARTESIAN_POINT('Ctrl Pts',(1.46026170981883,2.55571806290658,0.845285425732771));
#98865=CARTESIAN_POINT('Ctrl Pts',(1.37842170712222,2.60077549671088,0.850322931617301));
#98866=CARTESIAN_POINT('Ctrl Pts',(1.29458874332141,2.64185616294027,0.85536043750183));
#98867=CARTESIAN_POINT('Ctrl Pts',(1.21078631891674,2.68292186394974,0.860396108280206));
#98868=CARTESIAN_POINT('Ctrl Pts',(1.12499277404117,2.7200134802234,0.865431779058582));
#98869=CARTESIAN_POINT('Ctrl Pts',(1.03762222005052,2.75294462865809,0.870467449836958));
#98870=CARTESIAN_POINT('Ctrl Pts',(0.950259085454411,2.78587298062221,0.875502692992679));
#98871=CARTESIAN_POINT('Ctrl Pts',(0.861319623545659,2.8146414107707,0.880537936148401));
#98872=CARTESIAN_POINT('Ctrl Pts',(0.771236629574986,2.83911219595172,0.885573179304122));
#98873=CARTESIAN_POINT('Ctrl Pts',(0.681136119198972,2.86358773941368,0.89060940154986));
#98874=CARTESIAN_POINT('Ctrl Pts',(0.58989206370933,2.88376386222337,0.895645623795598));
#98875=CARTESIAN_POINT('Ctrl Pts',(0.497949957875531,2.89955338620481,0.900681846041336));
#98876=CARTESIAN_POINT('Ctrl Pts',(0.405907090868191,2.91536021423808,0.905723587582712));
#98877=CARTESIAN_POINT('Ctrl Pts',(0.313165084742484,2.92677077203526,0.910765329124089));
#98878=CARTESIAN_POINT('Ctrl Pts',(0.220176808105396,2.9337495075709,0.915807070665465));
#98879=CARTESIAN_POINT('Ctrl Pts',(0.127131573496098,2.94073251778116,0.920851900417366));
#98880=CARTESIAN_POINT('Ctrl Pts',(0.0338402115888993,2.9432782892246,0.925896730169267));
#98881=CARTESIAN_POINT('Ctrl Pts',(-0.0592443339899067,2.94140342504902,
0.930941559921168));
#98882=CARTESIAN_POINT('Ctrl Pts',(-0.15247932597867,2.93952553065416,0.935994543298575));
#98883=CARTESIAN_POINT('Ctrl Pts',(-0.245506391858317,2.93321276680787,
0.941047526675982));
#98884=CARTESIAN_POINT('Ctrl Pts',(-0.337877810556575,2.92253359007788,
0.946100510053389));
#98885=CARTESIAN_POINT('Ctrl Pts',(-0.384729005725857,2.91711706405419,
0.948663405738421));
#98886=CARTESIAN_POINT('Ctrl Pts',(-0.431411691090738,2.91057806867327,
0.951226301423452));
#98887=CARTESIAN_POINT('Ctrl Pts',(-0.4778687221613,2.90293049940572,0.953789197108484));
#98888=CARTESIAN_POINT('Ctrl Pts',(-0.569465358203213,2.88785223024682,
0.958842310014444));
#98889=CARTESIAN_POINT('Ctrl Pts',(-0.660511415684644,2.86840750677345,
0.963895422920404));
#98890=CARTESIAN_POINT('Ctrl Pts',(-0.75055847125516,2.84464865690424,0.968948535826364));
#98891=CARTESIAN_POINT('Ctrl Pts',(-0.8404816688065,2.82092248688297,0.973994698271244));
#98892=CARTESIAN_POINT('Ctrl Pts',(-0.929408169316603,2.79289409451912,
0.979040860716123));
#98893=CARTESIAN_POINT('Ctrl Pts',(-1.01689756881339,2.76066719010847,0.984087023161002));
#98894=CARTESIAN_POINT('Ctrl Pts',(-1.10429363537458,2.72847466508106,0.989127802403376));
#98895=CARTESIAN_POINT('Ctrl Pts',(-1.19025523370667,2.692092683341,0.994168581645751));
#98896=CARTESIAN_POINT('Ctrl Pts',(-1.27435607900167,2.65167505247372,0.999209360888125));
#98897=CARTESIAN_POINT('Ctrl Pts',(-1.35839667286267,2.61128637756056,1.00424652882104));
#98898=CARTESIAN_POINT('Ctrl Pts',(-1.44057876424077,2.56686799201402,1.00928369675396));
#98899=CARTESIAN_POINT('Ctrl Pts',(-1.52049603449511,2.51862180747421,1.01432086468688));
#98900=CARTESIAN_POINT('Ctrl Pts',(-1.60038445116335,2.47039304189071,1.01935621398463));
#98901=CARTESIAN_POINT('Ctrl Pts',(-1.67800929136593,2.41833945211539,1.02439156328237));
#98902=CARTESIAN_POINT('Ctrl Pts',(-1.75298976429711,2.36270837943864,1.02942691258012));
#98903=CARTESIAN_POINT('Ctrl Pts',(-1.82796412186676,2.30708184399817,1.03446185119785));
#98904=CARTESIAN_POINT('Ctrl Pts',(-1.90029418444405,2.24787867054407,1.03949678981559));
#98905=CARTESIAN_POINT('Ctrl Pts',(-1.96962997187994,2.18538824328132,1.04453172843332));
#98906=CARTESIAN_POINT('Ctrl Pts',(-2.03897948230982,2.1228854478637,1.0495676635701));
#98907=CARTESIAN_POINT('Ctrl Pts',(-2.10533321099665,2.05709440404767,1.05460359870687));
#98908=CARTESIAN_POINT('Ctrl Pts',(-2.16837681252091,1.98834252555279,1.05963953384365));
#98909=CARTESIAN_POINT('Ctrl Pts',(-2.23148986449097,1.91951490822802,1.06468101669553));
#98910=CARTESIAN_POINT('Ctrl Pts',(-2.29128520978513,1.84772027321607,1.0697224995474));
#98911=CARTESIAN_POINT('Ctrl Pts',(-2.34748792750901,1.77332017137331,1.07476398239928));
#98912=CARTESIAN_POINT('Ctrl Pts',(-2.403725248713,1.69887426209367,1.07980856924432));
#98913=CARTESIAN_POINT('Ctrl Pts',(-2.45636528844208,1.62182005880557,1.08485315608936));
#98914=CARTESIAN_POINT('Ctrl Pts',(-2.50517694724487,1.54254739408319,1.0898977429344));
#98915=CARTESIAN_POINT('Ctrl Pts',(-2.55406776315899,1.46314617410782,1.09495051050783));
#98916=CARTESIAN_POINT('Ctrl Pts',(-2.59911758937913,1.38151969871054,1.10000327808125));
#98917=CARTESIAN_POINT('Ctrl Pts',(-2.6401417594153,1.29808146515984,1.10505604565467));
#98918=CARTESIAN_POINT('Ctrl Pts',(-2.66097554208699,1.25570805400313,1.10762205153419));
#98919=CARTESIAN_POINT('Ctrl Pts',(-2.68077187101766,1.21286769363492,1.11018805741371));
#98920=CARTESIAN_POINT('Ctrl Pts',(-2.69951144407883,1.16961616066444,1.11275406329323));
#98921=CARTESIAN_POINT('Ctrl Pts',(-2.74022999787104,1.07563643838875,1.11832964647729));
#98922=CARTESIAN_POINT('Ctrl Pts',(-2.77608165791071,0.979425506923374,
1.12390522966136));
#98923=CARTESIAN_POINT('Ctrl Pts',(-2.80684144268218,0.881478936584314,
1.12948081284542));
#98924=CARTESIAN_POINT('Ctrl Pts',(-2.83751496533341,0.783807045632354,
1.13504075997641));
#98925=CARTESIAN_POINT('Ctrl Pts',(-2.8631249797981,0.684409483757163,1.1406007071074));
#98926=CARTESIAN_POINT('Ctrl Pts',(-2.88349448363252,0.583800961681977,
1.1461606542384));
#98927=CARTESIAN_POINT('Ctrl Pts',(-2.90376330266601,0.483689739349581,
1.15169311900288));
#98928=CARTESIAN_POINT('Ctrl Pts',(-2.91884317063577,0.382379762838641,
1.15722558376735));
#98929=CARTESIAN_POINT('Ctrl Pts',(-2.92860739691918,0.280397422795379,
1.16275804853183));
#98930=CARTESIAN_POINT('Ctrl Pts',(-2.9374705886954,0.187825926462083,1.16777998214742));
#98931=CARTESIAN_POINT('Ctrl Pts',(-2.94195441755449,0.0947008074507425,
1.172801915763));
#98932=CARTESIAN_POINT('Ctrl Pts',(-2.94199965400596,0.00142682472305235,
1.17782384937858));
#98933=CARTESIAN_POINT('',(-2.94199890897741,-0.00253368816290432,2.17782391179132));
#98934=CARTESIAN_POINT('Ctrl Pts',(-2.93779035503166,0.00142416137127735,
1.1778238829104));
#98935=CARTESIAN_POINT('Ctrl Pts',(-2.93530052620224,-0.579059729582153,
1.20912223176626));
#98936=CARTESIAN_POINT('Ctrl Pts',(-2.48777091207476,-2.14587530839216,
1.29340886935037));
#98937=CARTESIAN_POINT('Ctrl Pts',(0.062516362566841,-3.47815940114863,
1.43068379566273));
#98938=CARTESIAN_POINT('Ctrl Pts',(2.95837544317475,-1.83021987966787,1.58964866184748));
#98939=CARTESIAN_POINT('Ctrl Pts',(3.14027796553594,1.49678333878866,1.74861352803222));
#98940=CARTESIAN_POINT('Ctrl Pts',(0.441324113405188,3.45063445902487,1.90757839421697));
#98941=CARTESIAN_POINT('Ctrl Pts',(-2.35214246222887,2.36009024843845,2.0506485125097));
#98942=CARTESIAN_POINT('Ctrl Pts',(-2.93447401517848,0.684077783047056,
2.14073034207417));
#98943=CARTESIAN_POINT('Ctrl Pts',(-2.94008683942583,-0.00253150687518534,
2.1778238829104));
#98944=CARTESIAN_POINT('',(-2.9424770351591,-0.000169397631985995,3.1778238829104));
#98945=CARTESIAN_POINT('Ctrl Pts',(-2.94199890897741,-0.00253368816290432,
2.17782391179132));
#98946=CARTESIAN_POINT('Ctrl Pts',(-2.94190216531002,-0.114867860970932,
2.18388878241826));
#98947=CARTESIAN_POINT('Ctrl Pts',(-2.93536775276288,-0.226920986668357,
2.1899536530452));
#98948=CARTESIAN_POINT('Ctrl Pts',(-2.92251465713287,-0.338041534198877,
2.19601852367214));
#98949=CARTESIAN_POINT('Ctrl Pts',(-2.90948481331824,-0.450690145910656,
2.20216679482018));
#98950=CARTESIAN_POINT('Ctrl Pts',(-2.8899613801613,-0.562380351909379,
2.20831506596822));
#98951=CARTESIAN_POINT('Ctrl Pts',(-2.86411726493774,-0.672455420593505,
2.21446333711626));
#98952=CARTESIAN_POINT('Ctrl Pts',(-2.84864175944927,-0.738368581668222,
2.21814493360633));
#98953=CARTESIAN_POINT('Ctrl Pts',(-2.83090081430642,-0.803703035369289,
2.22182653009641));
#98954=CARTESIAN_POINT('Ctrl Pts',(-2.81093966913266,-0.86832147071023,
2.22550812658648));
#98955=CARTESIAN_POINT('Ctrl Pts',(-2.78354799893388,-0.956994082136707,
2.23056019529212));
#98956=CARTESIAN_POINT('Ctrl Pts',(-2.75190715797264,-1.0445286238472,2.23561226399775));
#98957=CARTESIAN_POINT('Ctrl Pts',(-2.71612972920927,-1.1304880778255,2.24066433270339));
#98958=CARTESIAN_POINT('Ctrl Pts',(-2.6804016769171,-1.21632889906102,2.24570942904311));
#98959=CARTESIAN_POINT('Ctrl Pts',(-2.64054855035648,-1.30059854550508,
2.25075452538283));
#98960=CARTESIAN_POINT('Ctrl Pts',(-2.59673275416955,-1.38287490519679,
2.25579962172254));
#98961=CARTESIAN_POINT('Ctrl Pts',(-2.55296388650603,-1.46506314351657,
2.26083931455617));
#98962=CARTESIAN_POINT('Ctrl Pts',(-2.50524099285918,-1.54526194844353,
2.26587900738979));
#98963=CARTESIAN_POINT('Ctrl Pts',(-2.45377419903128,-1.62306998622007,
2.27091870022342));
#98964=CARTESIAN_POINT('Ctrl Pts',(-2.40234454804303,-1.70082187106271,
2.27595475598372));
#98965=CARTESIAN_POINT('Ctrl Pts',(-2.34717661171069,-1.77618604868358,
2.28099081174402));
#98966=CARTESIAN_POINT('Ctrl Pts',(-2.28852546734672,-1.8487874905747,2.28602686750432));
#98967=CARTESIAN_POINT('Ctrl Pts',(-2.22989568477973,-1.92136248972068,
2.29106108904294));
#98968=CARTESIAN_POINT('Ctrl Pts',(-2.16778549339298,-1.99117640686272,
2.29609531058155));
#98969=CARTESIAN_POINT('Ctrl Pts',(-2.10249151778873,-2.05788566680135,
2.30112953212017));
#98970=CARTESIAN_POINT('Ctrl Pts',(-2.03720305329349,-2.12458929617453,
2.30616332874755));
#98971=CARTESIAN_POINT('Ctrl Pts',(-1.96873164977634,-2.18818847195827,
2.31119712537494));
#98972=CARTESIAN_POINT('Ctrl Pts',(-1.89741140531284,-2.24837584913838,
2.31623092200232));
#98973=CARTESIAN_POINT('Ctrl Pts',(-1.82607722448565,-2.30857498725936,
2.32126570226095));
#98974=CARTESIAN_POINT('Ctrl Pts',(-1.75189343691651,-2.36536071649472,
2.32630048251957));
#98975=CARTESIAN_POINT('Ctrl Pts',(-1.67522698116193,-2.41846615886745,
2.3313352627782));
#98976=CARTESIAN_POINT('Ctrl Pts',(-1.59847624074301,-2.47162998367538,
2.33637557811419));
#98977=CARTESIAN_POINT('Ctrl Pts',(-1.51923774978229,-2.52110519192561,
2.34141589345018));
#98978=CARTESIAN_POINT('Ctrl Pts',(-1.43790691383838,-2.56666860095646,
2.34645620878617));
#98979=CARTESIAN_POINT('Ctrl Pts',(-1.35652613571789,-2.61225998874583,
2.35149961918833));
#98980=CARTESIAN_POINT('Ctrl Pts',(-1.27305085199775,-2.65393459692558,
2.35654302959049));
#98981=CARTESIAN_POINT('Ctrl Pts',(-1.18789853504342,-2.69151650012436,
2.36158643999265));
#98982=CARTESIAN_POINT('Ctrl Pts',(-1.10260813749234,-2.72915934507795,
2.36663802864694));
#98983=CARTESIAN_POINT('Ctrl Pts',(-1.01563569170389,-2.76269607612556,
2.37168961730123));
#98984=CARTESIAN_POINT('Ctrl Pts',(-0.927415806383621,-2.79199998604402,
2.37674120595553));
#98985=CARTESIAN_POINT('Ctrl Pts',(-0.882407038325336,-2.80695050292502,
2.37931846822743));
#98986=CARTESIAN_POINT('Ctrl Pts',(-0.837073773584584,-2.82080006448637,
2.38189573049932));
#98987=CARTESIAN_POINT('Ctrl Pts',(-0.791474681886919,-2.83353698192418,
2.38447299277122));
#98988=CARTESIAN_POINT('Ctrl Pts',(-0.702089360760649,-2.85850444098862,
2.38952505427559));
#98989=CARTESIAN_POINT('Ctrl Pts',(-0.611360851967397,-2.87928305935194,
2.39457711577996));
#98990=CARTESIAN_POINT('Ctrl Pts',(-0.519717551769654,-2.89573093818859,
2.39962917728434));
#98991=CARTESIAN_POINT('Ctrl Pts',(-0.428200729617469,-2.91215611710539,
2.4046742663765));
#98992=CARTESIAN_POINT('Ctrl Pts',(-0.33577205834179,-2.92426235552378,
2.40971935546866));
#98993=CARTESIAN_POINT('Ctrl Pts',(-0.242874369756889,-2.93195771465333,
2.41476444456083));
#98994=CARTESIAN_POINT('Ctrl Pts',(-0.150076179228881,-2.93964483166953,
2.419804130111));
#98995=CARTESIAN_POINT('Ctrl Pts',(-0.0568104102683452,-2.94293042308684,
2.42484381566117));
#98996=CARTESIAN_POINT('Ctrl Pts',(0.0364717442503167,-2.94177392263093,
2.42988350121133));
#98997=CARTESIAN_POINT('Ctrl Pts',(0.12968657787327,-2.94061825681103,2.43491954966557));
#98998=CARTESIAN_POINT('Ctrl Pts',(0.22291733056244,-2.93502687660495,2.4399555981198));
#98999=CARTESIAN_POINT('Ctrl Pts',(0.315710594910331,-2.92501125130509,
2.44499164657403));
#99000=CARTESIAN_POINT('Ctrl Pts',(0.408470062032939,-2.91499927390303,
2.4500258607953));
#99001=CARTESIAN_POINT('Ctrl Pts',(0.50079191607328,-2.90056630024354,2.45506007501656));
#99002=CARTESIAN_POINT('Ctrl Pts',(0.592226706455157,-2.88177575952073,
2.46009428923783));
#99003=CARTESIAN_POINT('Ctrl Pts',(0.683653779273689,-2.86298680481554,
2.46512807854571));
#99004=CARTESIAN_POINT('Ctrl Pts',(0.774193502125792,-2.83984110392919,
2.47016186785358));
#99005=CARTESIAN_POINT('Ctrl Pts',(0.863406602989814,-2.81245320635092,
2.47519565716146));
#99006=CARTESIAN_POINT('Ctrl Pts',(0.952637136727754,-2.78505995698284,
2.48023043010754));
#99007=CARTESIAN_POINT('Ctrl Pts',(1.04054010903926,-2.75342299535612,2.48526520305361));
#99008=CARTESIAN_POINT('Ctrl Pts',(1.12669249679957,-2.7177063891553,2.49029997599969));
#99009=CARTESIAN_POINT('Ctrl Pts',(1.21293959884157,-2.68195051680309,2.49534028407852));
#99010=CARTESIAN_POINT('Ctrl Pts',(1.29743186360145,-2.64210621750187,2.50038059215735));
#99011=CARTESIAN_POINT('Ctrl Pts',(1.37976759867321,-2.5983851472889,2.50542090023618));
#99012=CARTESIAN_POINT('Ctrl Pts',(1.46215389340231,-2.55463722940977,2.51046430340184));
#99013=CARTESIAN_POINT('Ctrl Pts',(1.5423806403506,-2.50700802797234,2.5155077065675));
#99014=CARTESIAN_POINT('Ctrl Pts',(1.62007393732598,-2.45575333402952,2.52055110973316));
#99015=CARTESIAN_POINT('Ctrl Pts',(1.69789322133219,-2.40441552575178,2.52560269125416));
#99016=CARTESIAN_POINT('Ctrl Pts',(1.77317049537466,-2.34944074974798,2.53065427277516));
#99017=CARTESIAN_POINT('Ctrl Pts',(1.84556396510959,-2.29112584785056,2.53570585429616));
#99018=CARTESIAN_POINT('Ctrl Pts',(1.88249937124613,-2.26137337717496,2.53828318918276));
#99019=CARTESIAN_POINT('Ctrl Pts',(1.91868467709676,-2.23075205745533,2.54086052406937));
#99020=CARTESIAN_POINT('Ctrl Pts',(1.95407829257496,-2.19930489620865,2.54343785895597));
#99021=CARTESIAN_POINT('Ctrl Pts',(2.02345639223248,-2.13766258424246,2.54848991691042));
#99022=CARTESIAN_POINT('Ctrl Pts',(2.09003949319129,-2.07262344160913,2.55354197486487));
#99023=CARTESIAN_POINT('Ctrl Pts',(2.15347638948948,-2.00447086282424,2.55859403281932));
#99024=CARTESIAN_POINT('Ctrl Pts',(2.21682573467604,-1.93641234340198,2.56363911828117));
#99025=CARTESIAN_POINT('Ctrl Pts',(2.27703720352976,-1.86524924876456,2.56868420374302));
#99026=CARTESIAN_POINT('Ctrl Pts',(2.33379378359529,-1.79130415498094,2.57372928920488));
#99027=CARTESIAN_POINT('Ctrl Pts',(2.39048957364674,-1.71743826123521,2.57876897104981));
#99028=CARTESIAN_POINT('Ctrl Pts',(2.44373756094513,-1.64079664148663,2.58380865289474));
#99029=CARTESIAN_POINT('Ctrl Pts',(2.49325940237114,-1.56173671036059,2.58884833473968));
#99030=CARTESIAN_POINT('Ctrl Pts',(2.54274550335376,-1.48273383763365,2.59388437939224));
#99031=CARTESIAN_POINT('Ctrl Pts',(2.58851056843526,-1.40131649803873,2.59892042404481));
#99032=CARTESIAN_POINT('Ctrl Pts',(2.63031880851819,-1.31787213551067,2.60395646869737));
#99033=CARTESIAN_POINT('Ctrl Pts',(2.6721118206787,-1.2344581661366,2.60899067905849));
#99034=CARTESIAN_POINT('Ctrl Pts',(2.70995067210863,-1.14901903738044,2.61402488941961));
#99035=CARTESIAN_POINT('Ctrl Pts',(2.74364540472195,-1.06196699249464,2.61905909978072));
#99036=CARTESIAN_POINT('Ctrl Pts',(2.77733729296488,-0.97492229618355,2.62409288517456));
#99037=CARTESIAN_POINT('Ctrl Pts',(2.80688559771618,-0.886265368862106,
2.62912667056839));
#99038=CARTESIAN_POINT('Ctrl Pts',(2.83214885381344,-0.796427567229569,
2.63416045596223));
#99039=CARTESIAN_POINT('Ctrl Pts',(2.85741704628676,-0.706572211518826,
2.63919522494494));
#99040=CARTESIAN_POINT('Ctrl Pts',(2.87839840733941,-0.615535951036533,
2.64422999392765));
#99041=CARTESIAN_POINT('Ctrl Pts',(2.89500190357574,-0.523763284597973,
2.64926476291037));
#99042=CARTESIAN_POINT('Ctrl Pts',(2.91162365322265,-0.431889725905328,
2.65430506697461));
#99043=CARTESIAN_POINT('Ctrl Pts',(2.92385785167403,-0.339278583109973,
2.65934537103886));
#99044=CARTESIAN_POINT('Ctrl Pts',(2.9316650254743,-0.246382179572217,2.66438567510311));
#99045=CARTESIAN_POINT('Ctrl Pts',(2.93947699335174,-0.153428732021019,
2.66942907421907));
#99046=CARTESIAN_POINT('Ctrl Pts',(2.94285650858153,-0.0601901186905315,
2.67447247333503));
#99047=CARTESIAN_POINT('Ctrl Pts',(2.94181625057161,0.0328808131405041,
2.67951587245099));
#99048=CARTESIAN_POINT('Ctrl Pts',(2.94077430568675,0.126102668128605,2.68456744990687));
#99049=CARTESIAN_POINT('Ctrl Pts',(2.93529830536063,0.219155855786866,2.68961902736274));
#99050=CARTESIAN_POINT('Ctrl Pts',(2.9254528257311,0.311592304818211,2.69467060481862));
#99051=CARTESIAN_POINT('Ctrl Pts',(2.92042954776898,0.358754453823466,2.69724797825932));
#99052=CARTESIAN_POINT('Ctrl Pts',(2.91426965086572,0.405756209443027,2.69982535170001));
#99053=CARTESIAN_POINT('Ctrl Pts',(2.90698678445479,0.452539318739461,2.70240272514071));
#99054=CARTESIAN_POINT('Ctrl Pts',(2.89271120775524,0.544241655061684,2.70745478708446));
#99055=CARTESIAN_POINT('Ctrl Pts',(2.87406653123876,0.635432610317872,2.7125068490282));
#99056=CARTESIAN_POINT('Ctrl Pts',(2.85110093070811,0.725663477732859,2.71755891097195));
#99057=CARTESIAN_POINT('Ctrl Pts',(2.82816702538286,0.815769816034299,2.72260400048139));
#99058=CARTESIAN_POINT('Ctrl Pts',(2.80092415463223,0.904918272664531,2.72764908999083));
#99059=CARTESIAN_POINT('Ctrl Pts',(2.76947194826134,0.992667682456494,2.73269417950027));
#99060=CARTESIAN_POINT('Ctrl Pts',(2.73805342890985,1.0803231078699,2.73773386544514));
#99061=CARTESIAN_POINT('Ctrl Pts',(2.70243468419276,1.16658204884566,2.74277355139));
#99062=CARTESIAN_POINT('Ctrl Pts',(2.66276556900507,1.25101699609602,2.74781323733487));
#99063=CARTESIAN_POINT('Ctrl Pts',(2.62312508294012,1.33539100681032,2.75284928614826));
#99064=CARTESIAN_POINT('Ctrl Pts',(2.57944022493256,1.41794323929442,2.75788533496165));
#99065=CARTESIAN_POINT('Ctrl Pts',(2.53190913403474,1.49826570974292,2.76292138377504));
#99066=CARTESIAN_POINT('Ctrl Pts',(2.48439535515141,1.57855892473471,2.76795559833324));
#99067=CARTESIAN_POINT('Ctrl Pts',(2.43303835243074,1.65662360909303,2.77298981289144));
#99068=CARTESIAN_POINT('Ctrl Pts',(2.37808192542616,1.7320768908918,2.77802402744964));
#99069=CARTESIAN_POINT('Ctrl Pts',(2.32313013727259,1.80752380370788,2.78305781707172));
#99070=CARTESIAN_POINT('Ctrl Pts',(2.26457979063128,1.88035939318863,2.78809160669379));
#99071=CARTESIAN_POINT('Ctrl Pts',(2.20271700564477,1.95023121527765,2.79312539631587));
#99072=CARTESIAN_POINT('Ctrl Pts',(2.14084213251709,2.0201166904935,2.79816016955288));
#99073=CARTESIAN_POINT('Ctrl Pts',(2.07565383037372,2.08703691577986,2.8031949427899));
#99074=CARTESIAN_POINT('Ctrl Pts',(2.00747656861298,2.15067473748818,2.80822971602691));
#99075=CARTESIAN_POINT('Ctrl Pts',(1.93922435458943,2.21438252092002,2.81327002435931));
#99076=CARTESIAN_POINT('Ctrl Pts',(1.86797694701256,2.27480039393622,2.81831033269171));
#99077=CARTESIAN_POINT('Ctrl Pts',(1.79409330408111,2.33165032032063,2.82335064102411));
#99078=CARTESIAN_POINT('Ctrl Pts',(1.72016429195138,2.38853515613128,2.82839404442246));
#99079=CARTESIAN_POINT('Ctrl Pts',(1.6435961860873,2.44184742988604,2.83343744782082));
#99080=CARTESIAN_POINT('Ctrl Pts',(1.56477661589871,2.49135267321521,2.83848085121917));
#99081=CARTESIAN_POINT('Ctrl Pts',(1.48582923287356,2.54093819363241,2.84353243293787));
#99082=CARTESIAN_POINT('Ctrl Pts',(1.40462348339911,2.58670414117156,2.84858401465657));
#99083=CARTESIAN_POINT('Ctrl Pts',(1.3215710731625,2.62846226881424,2.85363559637527));
#99084=CARTESIAN_POINT('Ctrl Pts',(1.27919749248292,2.6497673866989,2.85621292802534));
#99085=CARTESIAN_POINT('Ctrl Pts',(1.23634353110035,2.67003001851766,2.8587902596754));
#99086=CARTESIAN_POINT('Ctrl Pts',(1.19306555526398,2.68923010931431,2.86136759132546));
#99087=CARTESIAN_POINT('Ctrl Pts',(1.10823248422076,2.72686594220878,2.86641965198094));
#99088=CARTESIAN_POINT('Ctrl Pts',(1.02146437177055,2.76055131467093,2.87147171263642));
#99089=CARTESIAN_POINT('Ctrl Pts',(0.933164579460419,2.79008384598751,2.8765237732919));
#99090=CARTESIAN_POINT('Ctrl Pts',(0.844986651378412,2.81957561889415,2.88156886150207));
#99091=CARTESIAN_POINT('Ctrl Pts',(0.755281661707406,2.84492579996593,2.88661394971225));
#99092=CARTESIAN_POINT('Ctrl Pts',(0.66447448324842,2.86597935462064,2.89165903792242));
#99093=CARTESIAN_POINT('Ctrl Pts',(0.573764564393398,2.88701035973222,2.8966987225589));
#99094=CARTESIAN_POINT('Ctrl Pts',(0.481955233668257,2.90375378561528,2.90173840719537));
#99095=CARTESIAN_POINT('Ctrl Pts',(0.389487068874256,2.91610422021912,2.90677809183185));
#99096=CARTESIAN_POINT('Ctrl Pts',(0.297085638339161,2.92844574151639,2.91181413932877));
#99097=CARTESIAN_POINT('Ctrl Pts',(0.204026757938821,2.93640051452241,2.9168501868257));
#99098=CARTESIAN_POINT('Ctrl Pts',(0.110760724522029,2.93991429499286,2.92188623432262));
#99099=CARTESIAN_POINT('Ctrl Pts',(0.0175286610244393,2.94342679565292,
2.92692044755984));
#99100=CARTESIAN_POINT('Ctrl Pts',(-0.0759099620612917,2.94250150043816,
2.93195466079707));
#99101=CARTESIAN_POINT('Ctrl Pts',(-0.169101246227653,2.93713615083201,
2.93698887403429));
#99102=CARTESIAN_POINT('Ctrl Pts',(-0.262284664097959,2.93177125411615,
2.94202266233251));
#99103=CARTESIAN_POINT('Ctrl Pts',(-0.35522034100107,2.92196707388151,2.94705645063072));
#99104=CARTESIAN_POINT('Ctrl Pts',(-0.44745705450973,2.90777340664115,2.95209023892894));
#99105=CARTESIAN_POINT('Ctrl Pts',(-0.539711791282198,2.89357696592589,
2.95712501084085));
#99106=CARTESIAN_POINT('Ctrl Pts',(-0.631266854362369,2.8749894027189,2.96215978275276));
#99107=CARTESIAN_POINT('Ctrl Pts',(-0.721679935661107,2.85211186149214,
2.96719455466467));
#99108=CARTESIAN_POINT('Ctrl Pts',(-0.81219241482694,2.82920916927209,2.97223486167816));
#99109=CARTESIAN_POINT('Ctrl Pts',(-0.901559974745023,2.80200719387074,
2.97727516869166));
#99110=CARTESIAN_POINT('Ctrl Pts',(-0.989354529215947,2.7706572533462,2.98231547570515));
#99111=CARTESIAN_POINT('Ctrl Pts',(-1.07720299509999,2.73928806197398,2.98735887778616));
#99112=CARTESIAN_POINT('Ctrl Pts',(-1.16347612203295,2.7037660037187,2.99240227986716));
#99113=CARTESIAN_POINT('Ctrl Pts',(-1.24776693683108,2.66429008768775,2.99744568194817));
#99114=CARTESIAN_POINT('Ctrl Pts',(-1.33219443686009,2.62475015786467,3.00249726236486));
#99115=CARTESIAN_POINT('Ctrl Pts',(-1.41463281490386,2.5812437774486,3.00754884278154));
#99116=CARTESIAN_POINT('Ctrl Pts',(-1.49470092919749,2.53401521942078,3.01260042319823));
#99117=CARTESIAN_POINT('Ctrl Pts',(-1.53555213192007,2.50991894320259,3.01517776796889));
#99118=CARTESIAN_POINT('Ctrl Pts',(-1.57578681340149,2.48485443600691,3.01775511273955));
#99119=CARTESIAN_POINT('Ctrl Pts',(-1.61535759876261,2.45885823668627,3.02033245751021));
#99120=CARTESIAN_POINT('Ctrl Pts',(-1.69279677129895,2.40798423592767,3.02537626557617));
#99121=CARTESIAN_POINT('Ctrl Pts',(-1.76797166233162,2.35335543275332,3.03042007364213));
#99122=CARTESIAN_POINT('Ctrl Pts',(-1.84049449808849,2.29520020967801,3.0354638817081));
#99123=CARTESIAN_POINT('Ctrl Pts',(-1.91291716172288,2.23712531346898,3.04050072301725));
#99124=CARTESIAN_POINT('Ctrl Pts',(-1.98269470377326,2.17553395208789,3.04553756432641));
#99125=CARTESIAN_POINT('Ctrl Pts',(-2.04946744717991,2.11069826904507,3.05057440563557));
#99126=CARTESIAN_POINT('Ctrl Pts',(-2.11616878274353,2.04593192232185,3.05560586046583));
#99127=CARTESIAN_POINT('Ctrl Pts',(-2.17987138803306,1.97792845857669,3.06063731529608));
#99128=CARTESIAN_POINT('Ctrl Pts',(-2.24024876236389,1.90700012656714,3.06566877012634));
#99129=CARTESIAN_POINT('Ctrl Pts',(-2.30058291089747,1.83612257407114,3.07069662280184));
#99130=CARTESIAN_POINT('Ctrl Pts',(-2.35759627164869,1.76232465365258,3.07572447547733));
#99131=CARTESIAN_POINT('Ctrl Pts',(-2.41100007869985,1.68595451317921,3.08075232815283));
#99132=CARTESIAN_POINT('Ctrl Pts',(-2.46438478843362,1.60961168283393,3.08577838285729));
#99133=CARTESIAN_POINT('Ctrl Pts',(-2.51416225325748,1.5306988247474,3.09080443756175));
#99134=CARTESIAN_POINT('Ctrl Pts',(-2.56008545935699,1.44959526792443,3.09583049226621));
#99135=CARTESIAN_POINT('Ctrl Pts',(-2.60600520700394,1.36849781896778,3.10085616846112));
#99136=CARTESIAN_POINT('Ctrl Pts',(-2.64807105353741,1.28521038748975,3.10588184465604));
#99137=CARTESIAN_POINT('Ctrl Pts',(-2.68608120570729,1.20013822385011,3.11090752085096));
#99138=CARTESIAN_POINT('Ctrl Pts',(-2.72409922529679,1.11504845179871,3.11593423727069));
#99139=CARTESIAN_POINT('Ctrl Pts',(-2.75805970201213,1.02817362130149,3.12096095369042));
#99140=CARTESIAN_POINT('Ctrl Pts',(-2.78780885240135,0.939939254671624,
3.12598767011016));
#99141=CARTESIAN_POINT('Ctrl Pts',(-2.81759078275611,0.851607664441793,
3.1310199253634));
#99142=CARTESIAN_POINT('Ctrl Pts',(-2.84315198266542,0.761913971385346,
3.13605218061663));
#99143=CARTESIAN_POINT('Ctrl Pts',(-2.86438856994763,0.671298830889301,
3.14108443586987));
#99144=CARTESIAN_POINT('Ctrl Pts',(-2.88563851571135,0.58062669061914,3.14611985656998));
#99145=CARTESIAN_POINT('Ctrl Pts',(-2.90255835329817,0.489032387258456,
3.15115527727009));
#99146=CARTESIAN_POINT('Ctrl Pts',(-2.91509573348633,0.396964563418193,
3.1561906979702));
#99147=CARTESIAN_POINT('Ctrl Pts',(-2.92765312232409,0.304749806741967,
3.16123415479642));
#99148=CARTESIAN_POINT('Ctrl Pts',(-2.93581405508617,0.212060464610946,
3.16627761162265));
#99149=CARTESIAN_POINT('Ctrl Pts',(-2.93957821840217,0.119347802223257,
3.17132106844887));
#99150=CARTESIAN_POINT('Ctrl Pts',(-2.94119600136931,0.0795012404625306,
3.17348867326938));
#99151=CARTESIAN_POINT('Ctrl Pts',(-2.94200228753483,0.039650337272543,
3.17565627808989));
#99152=CARTESIAN_POINT('Ctrl Pts',(-2.9419999951247,-0.000169370168916156,
3.1778238829104));
#99153=CARTESIAN_POINT('',(-2.94199882825472,0.00262574710428596,4.1778238829104));
#99154=CARTESIAN_POINT('Ctrl Pts',(-2.94684115129537,-0.00016964887300896,
3.1778238829104));
#99155=CARTESIAN_POINT('Ctrl Pts',(-2.94684868498682,-0.00920704813743015,
3.17831502983859));
#99156=CARTESIAN_POINT('Ctrl Pts',(-2.94681071471912,-0.0182443822752739,
3.17880617676677));
#99157=CARTESIAN_POINT('Ctrl Pts',(-2.93770067493934,-1.00224504924923,
3.23228561242321));
#99158=CARTESIAN_POINT('Ctrl Pts',(-1.8559090678843,-2.94232426067285,3.33826218987969));
#99159=CARTESIAN_POINT('Ctrl Pts',(1.46936377327205,-3.15319532053511,3.49722705606445));
#99160=CARTESIAN_POINT('Ctrl Pts',(3.44666251240458,-0.471368358035674,
3.6561919222492));
#99161=CARTESIAN_POINT('Ctrl Pts',(2.26204048071215,2.64288544059278,3.81515678843395));
#99162=CARTESIAN_POINT('Ctrl Pts',(-0.997746363252262,3.33259250407305,
3.9741216546187));
#99163=CARTESIAN_POINT('Ctrl Pts',(-2.78065560741015,1.53211675139101,4.09501045424348));
#99164=CARTESIAN_POINT('Ctrl Pts',(-2.94296032021889,0.278545523598026,
4.16291096514003));
#99165=CARTESIAN_POINT('Ctrl Pts',(-2.94059221637238,0.00263736173236185,
4.17782318730832));
#99166=CARTESIAN_POINT('',(-2.94172483514234,-0.00113785794874115,5.17782393613833));
#99167=CARTESIAN_POINT('Ctrl Pts',(-2.94199882825472,0.00262574710428596,
4.1778238829104));
#99168=CARTESIAN_POINT('Ctrl Pts',(-2.94208135216831,-0.089837558549181,
4.18281897121202));
#99169=CARTESIAN_POINT('Ctrl Pts',(-2.93780060605179,-0.182391783495091,
4.18781405951365));
#99170=CARTESIAN_POINT('Ctrl Pts',(-2.92915763932824,-0.274589737544923,
4.19280914781527));
#99171=CARTESIAN_POINT('Ctrl Pts',(-2.92051856511877,-0.366746168603293,
4.19780198648987));
#99172=CARTESIAN_POINT('Ctrl Pts',(-2.90752121322561,-0.458546197651342,
4.20279482516447));
#99173=CARTESIAN_POINT('Ctrl Pts',(-2.89021866431506,-0.549545332474808,
4.20778766383907));
#99174=CARTESIAN_POINT('Ctrl Pts',(-2.87291886798999,-0.640529990651052,
4.21277970822519));
#99175=CARTESIAN_POINT('Ctrl Pts',(-2.85131531996351,-0.730713563401275,
4.21777175261131));
#99176=CARTESIAN_POINT('Ctrl Pts',(-2.82551242969851,-0.819660606360478,
4.22276379699744));
#99177=CARTESIAN_POINT('Ctrl Pts',(-2.79970612822732,-0.908619408339702,
4.22775650134423));
#99178=CARTESIAN_POINT('Ctrl Pts',(-2.76969950941865,-0.996340921799696,
4.23274920569102));
#99179=CARTESIAN_POINT('Ctrl Pts',(-2.73564681545867,-1.08240496168062,
4.23774191003781));
#99180=CARTESIAN_POINT('Ctrl Pts',(-2.70155783753926,-1.16856070485338,
4.24273993423043));
#99181=CARTESIAN_POINT('Ctrl Pts',(-2.66341434533288,-1.25305502767173,
4.24773795842306));
#99182=CARTESIAN_POINT('Ctrl Pts',(-2.62141855177141,-1.33548821650686,
4.25273598261568));
#99183=CARTESIAN_POINT('Ctrl Pts',(-2.57939850044922,-1.41796902069584,
4.25773689378494));
#99184=CARTESIAN_POINT('Ctrl Pts',(-2.53352194388529,-1.49838592910131,
4.2627378049542));
#99185=CARTESIAN_POINT('Ctrl Pts',(-2.4840356721738,-1.5763663214393,4.26773871612346));
#99186=CARTESIAN_POINT('Ctrl Pts',(-2.43446682871423,-1.6544768302134,4.27274797170751));
#99187=CARTESIAN_POINT('Ctrl Pts',(-2.3812765059411,-1.73014233713128,4.27775722729155));
#99188=CARTESIAN_POINT('Ctrl Pts',(-2.3247530445471,-1.80302170865162,4.2827664828756));
#99189=CARTESIAN_POINT('Ctrl Pts',(-2.28983002984959,-1.84805022070626,
4.28586145091313));
#99190=CARTESIAN_POINT('Ctrl Pts',(-2.25363540625622,-1.89201583751354,
4.28895641895067));
#99191=CARTESIAN_POINT('Ctrl Pts',(-2.21624406221831,-1.93484527977874,
4.2920513869882));
#99192=CARTESIAN_POINT('Ctrl Pts',(-2.15520842775417,-2.00475777556257,
4.29710344763693));
#99193=CARTESIAN_POINT('Ctrl Pts',(-2.09075174052333,-2.07190496479329,
4.30215550828566));
#99194=CARTESIAN_POINT('Ctrl Pts',(-2.02315432548813,-2.13593318604742,
4.30720756893439));
#99195=CARTESIAN_POINT('Ctrl Pts',(-1.95565020298429,-2.19987304068521,
4.31225265713416));
#99196=CARTESIAN_POINT('Ctrl Pts',(-1.8850142857745,-2.26070217812353,4.31729774533392));
#99197=CARTESIAN_POINT('Ctrl Pts',(-1.8115663767167,-2.31810078787561,4.32234283353369));
#99198=CARTESIAN_POINT('Ctrl Pts',(-1.73819713456054,-2.3754379204414,4.32738251815611));
#99199=CARTESIAN_POINT('Ctrl Pts',(-1.6620222351466,-2.42935155639337,4.33242220277854));
#99200=CARTESIAN_POINT('Ctrl Pts',(-1.58339665538604,-2.4795602496637,4.33746188740096));
#99201=CARTESIAN_POINT('Ctrl Pts',(-1.50482781977722,-2.52973270727486,
4.34249793487845));
#99202=CARTESIAN_POINT('Ctrl Pts',(-1.42381219265337,-2.57620529842616,
4.34753398235595));
#99203=CARTESIAN_POINT('Ctrl Pts',(-1.34073514975917,-2.61873886789047,
4.35257002983344));
#99204=CARTESIAN_POINT('Ctrl Pts',(-1.2576883657436,-2.66125694549239,4.35760424304789));
#99205=CARTESIAN_POINT('Ctrl Pts',(-1.17258205262342,-2.69983864929842,
4.36263845626234));
#99206=CARTESIAN_POINT('Ctrl Pts',(-1.08582678373008,-2.73429043734099,
4.36767266947679));
#99207=CARTESIAN_POINT('Ctrl Pts',(-0.999078837924667,-2.76873931727808,
4.37270645774891));
#99208=CARTESIAN_POINT('Ctrl Pts',(-0.910682626085935,-2.79905881074814,
4.37774024602103));
#99209=CARTESIAN_POINT('Ctrl Pts',(-0.82106825667028,-2.82510370037782,
4.38277403429315));
#99210=CARTESIAN_POINT('Ctrl Pts',(-0.731436376461401,-2.85115367922119,
4.38780880617567));
#99211=CARTESIAN_POINT('Ctrl Pts',(-0.640586292675597,-2.87292727175354,
4.39284357805819));
#99212=CARTESIAN_POINT('Ctrl Pts',(-0.548961694685599,-2.89032957597709,
4.3978783499407));
#99213=CARTESIAN_POINT('Ctrl Pts',(-0.457236367006165,-2.90775101183929,
4.4029186569199));
#99214=CARTESIAN_POINT('Ctrl Pts',(-0.364735262637199,-2.9207914836135,
4.4079589638991));
#99215=CARTESIAN_POINT('Ctrl Pts',(-0.271910344332595,-2.9294075791267,
4.4129992708783));
#99216=CARTESIAN_POINT('Ctrl Pts',(-0.179028425704788,-2.93802896546307,
4.41804267292219));
#99217=CARTESIAN_POINT('Ctrl Pts',(-0.0858227408153346,-2.9422205468955,
4.42308607496607));
#99218=CARTESIAN_POINT('Ctrl Pts',(0.00725376937796118,-2.94199105757135,
4.42812947700996));
#99219=CARTESIAN_POINT('Ctrl Pts',(0.100481211533062,-2.94176119610956,
4.43318105738545));
#99220=CARTESIAN_POINT('Ctrl Pts',(0.193578617611841,-2.93709597365207,
4.43823263776094));
#99221=CARTESIAN_POINT('Ctrl Pts',(0.286097370379745,-2.92805606071021,
4.44328421813642));
#99222=CARTESIAN_POINT('Ctrl Pts',(0.333300963761295,-2.92344384575977,
4.4458615631486));
#99223=CARTESIAN_POINT('Ctrl Pts',(0.380354074264874,-2.91769368304617,
4.44843890816077));
#99224=CARTESIAN_POINT('Ctrl Pts',(0.427198334233323,-2.91081871356295,
4.45101625317294));
#99225=CARTESIAN_POINT('Ctrl Pts',(0.519021524882117,-2.89734253453937,
4.45606831382199));
#99226=CARTESIAN_POINT('Ctrl Pts',(0.610371415746862,-2.87949296899236,
4.46112037447104));
#99227=CARTESIAN_POINT('Ctrl Pts',(0.700798897592339,-2.85731428182714,
4.46617243512009));
#99228=CARTESIAN_POINT('Ctrl Pts',(0.791101578678766,-2.83516620390744,
4.47121752332016));
#99229=CARTESIAN_POINT('Ctrl Pts',(0.880483952658862,-2.80870098174539,
4.47626261152022));
#99230=CARTESIAN_POINT('Ctrl Pts',(0.968504003358442,-2.77801439799701,
4.48130769972029));
#99231=CARTESIAN_POINT('Ctrl Pts',(1.05642977956102,-2.74736068133089,4.48634738434301));
#99232=CARTESIAN_POINT('Ctrl Pts',(1.14299571542804,-2.71249473532883,4.49138706896572));
#99233=CARTESIAN_POINT('Ctrl Pts',(1.22777301259506,-2.67356268479781,4.49642675358844));
#99234=CARTESIAN_POINT('Ctrl Pts',(1.31248912591017,-2.6346587315628,4.50146280106621));
#99235=CARTESIAN_POINT('Ctrl Pts',(1.39541876368871,-2.59169469141985,4.50649884854399));
#99236=CARTESIAN_POINT('Ctrl Pts',(1.47615223166918,-2.54486514160144,4.51153489602176));
#99237=CARTESIAN_POINT('Ctrl Pts',(1.55685629436347,-2.49805264835632,4.51656910923649));
#99238=CARTESIAN_POINT('Ctrl Pts',(1.6353653924079,-2.44737766511334,4.52160332245121));
#99239=CARTESIAN_POINT('Ctrl Pts',(1.71129454468778,-2.39308064663978,4.52663753566593));
#99240=CARTESIAN_POINT('Ctrl Pts',(1.78721728772137,-2.33878821142513,4.5316713239383));
#99241=CARTESIAN_POINT('Ctrl Pts',(1.86056015667526,-2.28087460744231,4.53670511221068));
#99242=CARTESIAN_POINT('Ctrl Pts',(1.93096822846941,-2.21962287351742,4.54173890048305));
#99243=CARTESIAN_POINT('Ctrl Pts',(2.00139005811468,-2.15835917090463,4.5467736723658));
#99244=CARTESIAN_POINT('Ctrl Pts',(2.0688756167543,-2.09375633480824,4.55180844424854));
#99245=CARTESIAN_POINT('Ctrl Pts',(2.13310493629589,-2.02613605928874,4.55684321613129));
#99246=CARTESIAN_POINT('Ctrl Pts',(2.19740486787352,-1.95844144380478,4.56188352311072));
#99247=CARTESIAN_POINT('Ctrl Pts',(2.25844110810705,-1.8877230898025,4.56692383009015));
#99248=CARTESIAN_POINT('Ctrl Pts',(2.31593250440341,-1.81433751960537,4.57196413706958));
#99249=CARTESIAN_POINT('Ctrl Pts',(2.37345920402358,-1.7409068860646,4.57700753911368));
#99250=CARTESIAN_POINT('Ctrl Pts',(2.42743646936108,-1.66480613785273,4.58205094115778));
#99251=CARTESIAN_POINT('Ctrl Pts',(2.47762646424981,-1.58642084695361,4.58709434320188));
#99252=CARTESIAN_POINT('Ctrl Pts',(2.52789784674495,-1.50790844723094,4.59214592357756));
#99253=CARTESIAN_POINT('Ctrl Pts',(2.5743694769285,-1.42710449368637,4.59719750395325));
#99254=CARTESIAN_POINT('Ctrl Pts',(2.61684952849433,-1.34441903631978,4.60224908432894));
#99255=CARTESIAN_POINT('Ctrl Pts',(2.63852309216503,-1.30223244617172,4.60482642933852));
#99256=CARTESIAN_POINT('Ctrl Pts',(2.65915838336976,-1.25955640685416,4.6074037743481));
#99257=CARTESIAN_POINT('Ctrl Pts',(2.67873485657155,-1.21644710866877,4.60998111935769));
#99258=CARTESIAN_POINT('Ctrl Pts',(2.71710827168217,-1.13194511602972,4.61503318000808));
#99259=CARTESIAN_POINT('Ctrl Pts',(2.7515482331647,-1.04547374152125,4.62008524065846));
#99260=CARTESIAN_POINT('Ctrl Pts',(2.78184885414436,-0.957434568362622,
4.62513730130885));
#99261=CARTESIAN_POINT('Ctrl Pts',(2.81210765663692,-0.869516899810421,
4.63018238951028));
#99262=CARTESIAN_POINT('Ctrl Pts',(2.83823832728488,-0.780036148702834,
4.63522747771172));
#99263=CARTESIAN_POINT('Ctrl Pts',(2.86008213615458,-0.689415821148189,
4.64027256591315));
#99264=CARTESIAN_POINT('Ctrl Pts',(2.88190254905858,-0.598892553135136,
4.64531225053724));
#99265=CARTESIAN_POINT('Ctrl Pts',(2.89944512284491,-0.507232564302514,
4.65035193516134));
#99266=CARTESIAN_POINT('Ctrl Pts',(2.91260061141582,-0.414875497444982,
4.65539161978543));
#99267=CARTESIAN_POINT('Ctrl Pts',(2.92574660565883,-0.322585084765346,
4.66042766726462));
#99268=CARTESIAN_POINT('Ctrl Pts',(2.93451174538845,-0.229599032598319,
4.66546371474381));
#99269=CARTESIAN_POINT('Ctrl Pts',(2.93883786570519,-0.136367148160329,
4.670499762223));
#99270=CARTESIAN_POINT('Ctrl Pts',(2.94316241033333,-0.0431692212654586,
4.67553397543915));
#99271=CARTESIAN_POINT('Ctrl Pts',(2.94305112692431,0.0502739166469684,
4.6805681886553));
#99272=CARTESIAN_POINT('Ctrl Pts',(2.93849780295818,0.143508403969707,4.68560240187145));
#99273=CARTESIAN_POINT('Ctrl Pts',(2.93394486334212,0.236735021287823,4.69063619014526));
#99274=CARTESIAN_POINT('Ctrl Pts',(2.92495065051577,0.329752579268602,4.69566997841907));
#99275=CARTESIAN_POINT('Ctrl Pts',(2.91156102832598,0.422109438811009,4.70070376669288));
#99276=CARTESIAN_POINT('Ctrl Pts',(2.89816878978224,0.514484345033981,4.70573853857711));
#99277=CARTESIAN_POINT('Ctrl Pts',(2.88037950026913,0.606197856795858,4.71077331046133));
#99278=CARTESIAN_POINT('Ctrl Pts',(2.85829044730042,0.696806801682629,4.71580808234556));
#99279=CARTESIAN_POINT('Ctrl Pts',(2.83617711020399,0.787515359676054,4.72084838932645));
#99280=CARTESIAN_POINT('Ctrl Pts',(2.80975467926251,0.877116494502331,4.72588869630734));
#99281=CARTESIAN_POINT('Ctrl Pts',(2.77917073756452,0.965180818015509,4.73092900328823));
#99282=CARTESIAN_POINT('Ctrl Pts',(2.74856801540762,1.0532992185481,4.73597240533382));
#99283=CARTESIAN_POINT('Ctrl Pts',(2.71379886059695,1.13987851705496,4.7410158073794));
#99284=CARTESIAN_POINT('Ctrl Pts',(2.6750587293848,1.22451002214852,4.74605920942499));
#99285=CARTESIAN_POINT('Ctrl Pts',(2.63625577755367,1.30927876486542,4.75111078980215));
#99286=CARTESIAN_POINT('Ctrl Pts',(2.5934691976648,1.39209301428078,4.75616237017931));
#99287=CARTESIAN_POINT('Ctrl Pts',(2.54693993315464,1.47256951513408,4.76121395055647));
#99288=CARTESIAN_POINT('Ctrl Pts',(2.52320043817133,1.51362908287912,4.76379129555179));
#99289=CARTESIAN_POINT('Ctrl Pts',(2.49848737801963,1.55408058727492,4.76636864054711));
#99290=CARTESIAN_POINT('Ctrl Pts',(2.47283687747492,1.59387633692206,4.76894598554244));
#99291=CARTESIAN_POINT('Ctrl Pts',(2.42255727397671,1.67188317775094,4.77399804619198));
#99292=CARTESIAN_POINT('Ctrl Pts',(2.36849255924784,1.74764871196324,4.77905010684153));
#99293=CARTESIAN_POINT('Ctrl Pts',(2.31086894656018,1.82078244494608,4.78410216749107));
#99294=CARTESIAN_POINT('Ctrl Pts',(2.25332486136184,1.89381524461534,4.78914725569163));
#99295=CARTESIAN_POINT('Ctrl Pts',(2.19223191093946,1.96422311472191,4.7941923438922));
#99296=CARTESIAN_POINT('Ctrl Pts',(2.12786026825709,2.03164334438229,4.79923743209277));
#99297=CARTESIAN_POINT('Ctrl Pts',(2.06355757127691,2.09899136312989,4.80427711671601));
#99298=CARTESIAN_POINT('Ctrl Pts',(1.99598346714828,2.16335778214007,4.80931680133925));
#99299=CARTESIAN_POINT('Ctrl Pts',(1.92544848290709,2.22441276288166,4.8143564859625));
#99300=CARTESIAN_POINT('Ctrl Pts',(1.85496440382756,2.28542368018864,4.81939253344081));
#99301=CARTESIAN_POINT('Ctrl Pts',(1.78152402691584,2.34312761946754,4.82442858091912));
#99302=CARTESIAN_POINT('Ctrl Pts',(1.7054740763129,2.39723219046981,4.82946462839743));
#99303=CARTESIAN_POINT('Ctrl Pts',(1.62945182513385,2.45131705514176,4.83449884161269));
#99304=CARTESIAN_POINT('Ctrl Pts',(1.55082225014268,2.5018048986372,4.83953305482796));
#99305=CARTESIAN_POINT('Ctrl Pts',(1.46996360669441,2.54844481890308,4.84456726804323));
#99306=CARTESIAN_POINT('Ctrl Pts',(1.38911178859481,2.59508080225258,4.84960105631616));
#99307=CARTESIAN_POINT('Ctrl Pts',(1.30603166109351,2.63786928631908,4.8546348445891));
#99308=CARTESIAN_POINT('Ctrl Pts',(1.22112780010209,2.67660435922417,4.85966863286203));
#99309=CARTESIAN_POINT('Ctrl Pts',(1.13620734875875,2.71534700102523,4.86470340474534));
#99310=CARTESIAN_POINT('Ctrl Pts',(1.04946286054611,2.75003447459957,4.86973817662866));
#99311=CARTESIAN_POINT('Ctrl Pts',(0.96131962835742,2.780508689455,4.87477294851197));
#99312=CARTESIAN_POINT('Ctrl Pts',(0.873079493801843,2.81101640686616,4.87981325549197));
#99313=CARTESIAN_POINT('Ctrl Pts',(0.783437966308261,2.83730147420214,4.88485356247197));
#99314=CARTESIAN_POINT('Ctrl Pts',(0.692835973951886,2.85925555227198,4.88989386945197));
#99315=CARTESIAN_POINT('Ctrl Pts',(0.602178346288217,2.88122311152306,4.89493727149666));
#99316=CARTESIAN_POINT('Ctrl Pts',(0.510559515593608,2.89885430307471,4.89998067354135));
#99317=CARTESIAN_POINT('Ctrl Pts',(0.418428921662,2.91209224399173,4.90502407558604));
#99318=CARTESIAN_POINT('Ctrl Pts',(0.326148929657618,2.92535165142466,4.91007565596231));
#99319=CARTESIAN_POINT('Ctrl Pts',(0.233355959421926,2.93420354369714,4.91512723633859));
#99320=CARTESIAN_POINT('Ctrl Pts',(0.14050268594035,2.93864305339106,4.92017881671486));
#99321=CARTESIAN_POINT('Ctrl Pts',(0.0931284183453548,2.9409081164561,4.92275616171897));
#99322=CARTESIAN_POINT('Ctrl Pts',(0.0457384281583306,2.94202543260133,
4.92533350672308));
#99323=CARTESIAN_POINT('Ctrl Pts',(-0.00160762990463156,2.94199956076239,
4.92791085172719));
#99324=CARTESIAN_POINT('Ctrl Pts',(-0.0944144355417648,2.94194884729591,
4.93296291237685));
#99325=CARTESIAN_POINT('Ctrl Pts',(-0.187385601049113,2.93750228257937,
4.9380149730265));
#99326=CARTESIAN_POINT('Ctrl Pts',(-0.280070337951304,2.92863869499121,
4.94306703367616));
#99327=CARTESIAN_POINT('Ctrl Pts',(-0.372627158812504,2.91978734021583,
4.94811212187687));
#99328=CARTESIAN_POINT('Ctrl Pts',(-0.464897898150164,2.90653111802456,
4.95315721007757));
#99329=CARTESIAN_POINT('Ctrl Pts',(-0.556431333062393,2.88890085873268,
4.95820229827827));
#99330=CARTESIAN_POINT('Ctrl Pts',(-0.647866730442982,2.87128948245447,
4.96324198290164));
#99331=CARTESIAN_POINT('Ctrl Pts',(-0.738565959096744,2.84931346445757,
4.968281667525));
#99332=CARTESIAN_POINT('Ctrl Pts',(-0.828083592084304,2.82305535980447,
4.97332135214837));
#99333=CARTESIAN_POINT('Ctrl Pts',(-0.917536620115285,2.79681620564922,
4.9783573996268));
#99334=CARTESIAN_POINT('Ctrl Pts',(-1.00580932234237,2.76630123209306,4.98339344710522));
#99335=CARTESIAN_POINT('Ctrl Pts',(-1.09246816554048,2.7316437006463,4.98842949458364));
#99336=CARTESIAN_POINT('Ctrl Pts',(-1.17909544527248,2.6969987923985,4.99346370779902));
#99337=CARTESIAN_POINT('Ctrl Pts',(-1.26410962160118,2.65821448851637,4.99849792101439));
#99338=CARTESIAN_POINT('Ctrl Pts',(-1.34709497755487,2.61547302059235,5.00353213422977));
#99339=CARTESIAN_POINT('Ctrl Pts',(-1.43007332864213,2.57273516051298,5.00856592250281));
#99340=CARTESIAN_POINT('Ctrl Pts',(-1.51102280493738,2.52604100410974,5.01359971077585));
#99341=CARTESIAN_POINT('Ctrl Pts',(-1.58955127083903,2.47561926745088,5.01863349904888));
#99342=CARTESIAN_POINT('Ctrl Pts',(-1.66809508132968,2.42518767830329,5.02366827093228));
#99343=CARTESIAN_POINT('Ctrl Pts',(-1.74421656826335,2.37102730269974,5.02870304281567));
#99344=CARTESIAN_POINT('Ctrl Pts',(-1.817552591216,2.3134101621122,5.03373781469906));
#99345=CARTESIAN_POINT('Ctrl Pts',(-1.89096923787689,2.25572967874514,5.03877812167917));
#99346=CARTESIAN_POINT('Ctrl Pts',(-1.9615939579699,2.19458511947457,5.04381842865927));
#99347=CARTESIAN_POINT('Ctrl Pts',(-2.02909697978266,2.1302885829476,5.04885873563937));
#99348=CARTESIAN_POINT('Ctrl Pts',(-2.09664145268573,2.06595256431345,5.05390213768417));
#99349=CARTESIAN_POINT('Ctrl Pts',(-2.16106010456226,1.99846103636965,5.05894553972897));
#99350=CARTESIAN_POINT('Ctrl Pts',(-2.22206182195982,1.92816110825538,5.06398894177377));
#99351=CARTESIAN_POINT('Ctrl Pts',(-2.28316245914736,1.8577471824633,5.06904052215014));
#99352=CARTESIAN_POINT('Ctrl Pts',(-2.34083482556924,1.78451611341707,5.07409210252651));
#99353=CARTESIAN_POINT('Ctrl Pts',(-2.39482979249436,1.70884588684334,5.07914368290288));
#99354=CARTESIAN_POINT('Ctrl Pts',(-2.42237833133254,1.67023850740831,5.0817210279059));
#99355=CARTESIAN_POINT('Ctrl Pts',(-2.44897032649087,1.63099662472023,5.08429837290891));
#99356=CARTESIAN_POINT('Ctrl Pts',(-2.47457731972873,1.59117286574532,5.08687571791193));
#99357=CARTESIAN_POINT('Ctrl Pts',(-2.52593063722472,1.51130866148183,5.09204443159132));
#99358=CARTESIAN_POINT('Ctrl Pts',(-2.57349750309413,1.42882627654237,5.09721314527072));
#99359=CARTESIAN_POINT('Ctrl Pts',(-2.61700801586616,1.34411050322966,5.10238185895011));
#99360=CARTESIAN_POINT('Ctrl Pts',(-2.66044994472782,1.25952826405923,5.10754242538938));
#99361=CARTESIAN_POINT('Ctrl Pts',(-2.69984804730073,1.17272000538954,5.11270299182864));
#99362=CARTESIAN_POINT('Ctrl Pts',(-2.73497600826104,1.08409881202615,5.11786355826791));
#99363=CARTESIAN_POINT('Ctrl Pts',(-2.77004439535526,0.995627912245485,
5.12301537285009));
#99364=CARTESIAN_POINT('Ctrl Pts',(-2.80085690770018,0.905350584992716,
5.12816718743227));
#99365=CARTESIAN_POINT('Ctrl Pts',(-2.82723399079956,0.813702624591811,
5.13331900201445));
#99366=CARTESIAN_POINT('Ctrl Pts',(-2.85358474443882,0.72214614668383,5.13846567408349));
#99367=CARTESIAN_POINT('Ctrl Pts',(-2.87550875792413,0.629222154936498,
5.14361234615252));
#99368=CARTESIAN_POINT('Ctrl Pts',(-2.89287532254258,0.535384318246417,
5.14875901822156));
#99369=CARTESIAN_POINT('Ctrl Pts',(-2.91022669374542,0.441628577082012,
5.15390118764258));
#99370=CARTESIAN_POINT('Ctrl Pts',(-2.9230284755394,0.346960990963471,5.1590433570636));
#99371=CARTESIAN_POINT('Ctrl Pts',(-2.93120059672715,0.251847298469479,
5.16418552648463));
#99372=CARTESIAN_POINT('Ctrl Pts',(-2.93842545277446,0.167758636467438,
5.16873164529322));
#99373=CARTESIAN_POINT('Ctrl Pts',(-2.94203242052034,0.0833216685275416,
5.17327776410181));
#99374=CARTESIAN_POINT('Ctrl Pts',(-2.94199978029974,-0.0011369768179453,
5.1778238829104));
#99375=CARTESIAN_POINT('',(-2.9447614944152,-0.00213938116747883,6.1778238829104));
#99376=CARTESIAN_POINT('Ctrl Pts',(-2.9375628487339,-0.00115119607926536,
5.17782474187691));
#99377=CARTESIAN_POINT('Ctrl Pts',(-2.93901668938036,-0.421720246351829,
5.2004966892835));
#99378=CARTESIAN_POINT('Ctrl Pts',(-2.65772642519255,-1.82337310569149,
5.27615692541833));
#99379=CARTESIAN_POINT('Ctrl Pts',(-0.501375558914218,-3.44242547455181,
5.40480545028144));
#99380=CARTESIAN_POINT('Ctrl Pts',(2.62307973245116,-2.28497774958579,5.56377031646618));
#99381=CARTESIAN_POINT('Ctrl Pts',(3.34115776752328,0.968677124442226,5.72273518265092));
#99382=CARTESIAN_POINT('Ctrl Pts',(0.994103636774833,3.33368093228121,5.88170004883567));
#99383=CARTESIAN_POINT('Ctrl Pts',(-2.1159090271005,2.67211129893139,6.0333962822555));
#99384=CARTESIAN_POINT('Ctrl Pts',(-2.93786789722844,0.840699408537156,
6.13210422694707));
#99385=CARTESIAN_POINT('Ctrl Pts',(-2.9447614944152,-0.00213938116747883,
6.1778238829104));
#99386=CARTESIAN_POINT('',(-2.94432271303247,0.00230217249621089,7.1778238829104));
#99387=CARTESIAN_POINT('Ctrl Pts',(-2.9447614944152,-0.00213938116747883,
6.1778238829104));
#99388=CARTESIAN_POINT('Ctrl Pts',(-2.94585745686995,-0.136136138433291,
6.18509251567532));
#99389=CARTESIAN_POINT('Ctrl Pts',(-2.8766146460885,-1.24582928930445,6.24534943716847));
#99390=CARTESIAN_POINT('Ctrl Pts',(-1.46591682683645,-3.1547992734402,6.35859464738994));
#99391=CARTESIAN_POINT('Ctrl Pts',(1.85912357706067,-2.94029422407329,6.51755951357464));
#99392=CARTESIAN_POINT('Ctrl Pts',(3.47862959055127,-0.0284037082704225,
6.67652437975942));
#99393=CARTESIAN_POINT('Ctrl Pts',(1.90688867921259,2.90954397870054,6.83548924594416));
#99394=CARTESIAN_POINT('Ctrl Pts',(-1.4142056700595,3.17831605125627,6.99445411212891));
#99395=CARTESIAN_POINT('Ctrl Pts',(-2.86691655368935,1.2782107101568,7.10856565778431));
#99396=CARTESIAN_POINT('Ctrl Pts',(-2.94561300180491,0.152327949348626,
7.16968891471148));
#99397=CARTESIAN_POINT('Ctrl Pts',(-2.94432271303247,0.00230217249621089,
7.1778238829104));
#99398=CARTESIAN_POINT('',(-2.94164226802472,0.000891056651905342,8.17782382888466));
#99399=CARTESIAN_POINT('Ctrl Pts',(-2.94432271303247,0.00230217249621089,
7.1778238829104));
#99400=CARTESIAN_POINT('Ctrl Pts',(-2.93720851977804,-0.824886587469865,
7.22267720343973));
#99401=CARTESIAN_POINT('Ctrl Pts',(-2.14156346621365,-2.64127142281798,
7.32051881269732));
#99402=CARTESIAN_POINT('Ctrl Pts',(0.939534373351018,-3.34946947443834,
7.47134871068315));
#99403=CARTESIAN_POINT('Ctrl Pts',(3.32489445249589,-1.02310677774301,7.63031357686789));
#99404=CARTESIAN_POINT('Ctrl Pts',(2.66004210726286,2.24184000019857,7.78927844305266));
#99405=CARTESIAN_POINT('Ctrl Pts',(-0.445096268358593,3.45015360684055,
7.94824330923738));
#99406=CARTESIAN_POINT('Ctrl Pts',(-2.64229580147289,1.85586383567465,8.07775822408788));
#99407=CARTESIAN_POINT('Ctrl Pts',(-2.93857546330054,0.437603748156834,
8.15428485021008));
#99408=CARTESIAN_POINT('Ctrl Pts',(-2.93739762163734,0.000901669888460307,
8.17782318760405));
#99409=CARTESIAN_POINT('',(-2.94199878001864,-0.00267924781501915,9.17782388293972));
#99410=CARTESIAN_POINT('Ctrl Pts',(-2.94199986533152,0.000890162522109321,
8.17782388291041));
#99411=CARTESIAN_POINT('Ctrl Pts',(-2.94202891373335,-0.0951152209337257,
8.18299050364209));
#99412=CARTESIAN_POINT('Ctrl Pts',(-2.93735424679165,-0.191077943521917,
8.18815712437376));
#99413=CARTESIAN_POINT('Ctrl Pts',(-2.92801456306122,-0.286521759211059,
8.19332374510544));
#99414=CARTESIAN_POINT('Ctrl Pts',(-2.91866794100087,-0.382036478873143,
8.19849420405265));
#99415=CARTESIAN_POINT('Ctrl Pts',(-2.90464944199645,-0.477031115879893,
8.20366466299987));
#99416=CARTESIAN_POINT('Ctrl Pts',(-2.88604933563209,-0.571036979798659,
8.20883512194709));
#99417=CARTESIAN_POINT('Ctrl Pts',(-2.86741566602941,-0.66521247399547,
8.21401491080578));
#99418=CARTESIAN_POINT('Ctrl Pts',(-2.84418395519744,-0.758395227740191,
8.21919469966447));
#99419=CARTESIAN_POINT('Ctrl Pts',(-2.81649520403065,-0.850128675949902,
8.22437448852317));
#99420=CARTESIAN_POINT('Ctrl Pts',(-2.78877986988186,-0.941950194170039,
8.22955925031232));
#99421=CARTESIAN_POINT('Ctrl Pts',(-2.75659910502718,-1.03231924749004,
8.23474401210148));
#99422=CARTESIAN_POINT('Ctrl Pts',(-2.72014243688788,-1.12079843104891,
8.23992877389063));
#99423=CARTESIAN_POINT('Ctrl Pts',(-2.6836082499766,-1.20946575022204,8.2451245601751));
#99424=CARTESIAN_POINT('Ctrl Pts',(-2.64278016627184,-1.29623479789819,
8.25032034645956));
#99425=CARTESIAN_POINT('Ctrl Pts',(-2.59789436989746,-1.3806914365111,8.25551613274402));
#99426=CARTESIAN_POINT('Ctrl Pts',(-2.56720643580305,-1.43843352797297,
8.25906843569831));
#99427=CARTESIAN_POINT('Ctrl Pts',(-2.5346227496621,-1.49509527446311,8.2626207386526));
#99428=CARTESIAN_POINT('Ctrl Pts',(-2.50023013796568,-1.55055256512255,
8.26617304160688));
#99429=CARTESIAN_POINT('Ctrl Pts',(-2.45131720389756,-1.62942353966689,
8.27122510225662));
#99430=CARTESIAN_POINT('Ctrl Pts',(-2.39858068495313,-1.70611949212522,
8.27627716290635));
#99431=CARTESIAN_POINT('Ctrl Pts',(-2.3422399568583,-1.78024604605555,8.28132922355608));
#99432=CARTESIAN_POINT('Ctrl Pts',(-2.28597698571825,-1.85427029646059,
8.28637431175685));
#99433=CARTESIAN_POINT('Ctrl Pts',(-2.22611995635826,-1.92573184417074,
8.29141939995761));
#99434=CARTESIAN_POINT('Ctrl Pts',(-2.16293268157365,-1.99426332638912,
8.29646448815837));
#99435=CARTESIAN_POINT('Ctrl Pts',(-2.09981308396582,-2.06272140747962,
8.3015041727818));
#99436=CARTESIAN_POINT('Ctrl Pts',(-2.03337063018068,-2.12825533594879,
8.30654385740523));
#99437=CARTESIAN_POINT('Ctrl Pts',(-1.96391005366405,-2.19052991331259,
8.31158354202866));
#99438=CARTESIAN_POINT('Ctrl Pts',(-1.89449960690803,-2.25275954705785,
8.31661958950715));
#99439=CARTESIAN_POINT('Ctrl Pts',(-1.82207569671189,-2.31173420942861,
8.32165563698566));
#99440=CARTESIAN_POINT('Ctrl Pts',(-1.74697990055814,-2.3671555139124,8.32669168446415));
#99441=CARTESIAN_POINT('Ctrl Pts',(-1.67191145629963,-2.42255663247644,
8.33172589767961));
#99442=CARTESIAN_POINT('Ctrl Pts',(-1.59417341651241,-2.47440670069988,
8.33676011089507));
#99443=CARTESIAN_POINT('Ctrl Pts',(-1.51413960791633,-2.52244826463081,
8.34179432411054));
#99444=CARTESIAN_POINT('Ctrl Pts',(-1.43411255504405,-2.5704857733313,8.34682811238366));
#99445=CARTESIAN_POINT('Ctrl Pts',(-1.35179049968913,-2.6147151883972,8.35186190065678));
#99446=CARTESIAN_POINT('Ctrl Pts',(-1.26757436895377,-2.65492358066507,
8.3568956889299));
#99447=CARTESIAN_POINT('Ctrl Pts',(-1.18334178224989,-2.695139829718,8.36193046081341));
#99448=CARTESIAN_POINT('Ctrl Pts',(-1.09721478622076,-2.73133330445973,
8.36696523269692));
#99449=CARTESIAN_POINT('Ctrl Pts',(-1.00961585495202,-2.76333852892285,
8.37200000458044));
#99450=CARTESIAN_POINT('Ctrl Pts',(-0.921920619706692,-2.79537893909364,
8.37704031156063));
#99451=CARTESIAN_POINT('Ctrl Pts',(-0.832750637045269,-2.82322175520524,
8.38208061854082));
#99452=CARTESIAN_POINT('Ctrl Pts',(-0.742544880631375,-2.84675097264375,
8.38712092552101));
#99453=CARTESIAN_POINT('Ctrl Pts',(-0.652283732224084,-2.87029463849784,
8.39216432756589));
#99454=CARTESIAN_POINT('Ctrl Pts',(-0.560985978304944,-2.88951934092225,
8.39720772961076));
#99455=CARTESIAN_POINT('Ctrl Pts',(-0.46909999943738,-2.90436037545754,
8.40225113165564));
#99456=CARTESIAN_POINT('Ctrl Pts',(-0.377065019162338,-2.91922547606973,
8.4073027120321));
#99457=CARTESIAN_POINT('Ctrl Pts',(-0.284440350611836,-2.92969266759963,
8.41235429240856));
#99458=CARTESIAN_POINT('Ctrl Pts',(-0.191678515266118,-2.93574919684659,
8.41740587278502));
#99459=CARTESIAN_POINT('Ctrl Pts',(-0.144350899964211,-2.93883927247086,
8.41998321778722));
#99460=CARTESIAN_POINT('Ctrl Pts',(-0.0969875683649003,-2.94078204929621,
8.42256056278943));
#99461=CARTESIAN_POINT('Ctrl Pts',(-0.0496482455559902,-2.94158104625951,
8.42513790779164));
#99462=CARTESIAN_POINT('Ctrl Pts',(0.0431453578393812,-2.94314722428927,
8.43018996844137));
#99463=CARTESIAN_POINT('Ctrl Pts',(0.136179880851625,-2.94032108173428,
8.4352420290911));
#99464=CARTESIAN_POINT('Ctrl Pts',(0.229004972276714,-2.93307359653189,
8.44029408974083));
#99465=CARTESIAN_POINT('Ctrl Pts',(0.321701953954428,-2.92583611372739,
8.44533917794158));
#99466=CARTESIAN_POINT('Ctrl Pts',(0.4141896393011,-2.91418944793322,8.45038426614234));
#99467=CARTESIAN_POINT('Ctrl Pts',(0.506016336772334,-2.89815656356235,
8.45542935434309));
#99468=CARTESIAN_POINT('Ctrl Pts',(0.597744682611139,-2.88214085132543,
8.46046903896652));
#99469=CARTESIAN_POINT('Ctrl Pts',(0.688813012414029,-2.8617483342539,8.46550872358996));
#99470=CARTESIAN_POINT('Ctrl Pts',(0.778774528568876,-2.83705379463491,
8.47054840821339));
#99471=CARTESIAN_POINT('Ctrl Pts',(0.868671119416541,-2.81237707708738,
8.47558445569189));
#99472=CARTESIAN_POINT('Ctrl Pts',(0.95746205709736,-2.78340462542002,8.48062050317039));
#99473=CARTESIAN_POINT('Ctrl Pts',(1.04471155249861,-2.75026212788453,8.48565655064889));
#99474=CARTESIAN_POINT('Ctrl Pts',(1.13192926930258,-2.71713170173212,8.49069076386435));
#99475=CARTESIAN_POINT('Ctrl Pts',(1.21760624424501,-2.67983440465244,8.49572497707981));
#99476=CARTESIAN_POINT('Ctrl Pts',(1.30132364860379,-2.63854519794233,8.50075919029527));
#99477=CARTESIAN_POINT('Ctrl Pts',(1.38503398630335,-2.59725947649022,8.5057929785684));
#99478=CARTESIAN_POINT('Ctrl Pts',(1.46678468389312,-2.55198271204595,8.51082676684153));
#99479=CARTESIAN_POINT('Ctrl Pts',(1.54617968058766,-2.50293675416257,8.51586055511465));
#99480=CARTESIAN_POINT('Ctrl Pts',(1.62559019119318,-2.45388121261956,8.52089532699816));
#99481=CARTESIAN_POINT('Ctrl Pts',(1.70264370895385,-2.40105524874215,8.52593009888167));
#99482=CARTESIAN_POINT('Ctrl Pts',(1.77697240939263,-2.3447245160695,8.53096487076518));
#99483=CARTESIAN_POINT('Ctrl Pts',(1.8513828248629,-2.28833185486094,8.53600517774537));
#99484=CARTESIAN_POINT('Ctrl Pts',(1.92306208877641,-2.22842700245585,8.54104548472556));
#99485=CARTESIAN_POINT('Ctrl Pts',(1.99167504207716,-2.16531626483683,8.54608579170575));
#99486=CARTESIAN_POINT('Ctrl Pts',(2.06033012803545,-2.10216677326587,8.55112919375062));
#99487=CARTESIAN_POINT('Ctrl Pts',(2.12591484279603,-2.03580779313716,8.55617259579548));
#99488=CARTESIAN_POINT('Ctrl Pts',(2.18813206974124,-1.96658130911741,8.56121599784034));
#99489=CARTESIAN_POINT('Ctrl Pts',(2.25045018753521,-1.89724256810593,8.5662675782168));
#99490=CARTESIAN_POINT('Ctrl Pts',(2.30938963527,-1.82502738394544,8.57131915859326));
#99491=CARTESIAN_POINT('Ctrl Pts',(2.36469473674397,-1.75030934466321,8.57637073896973));
#99492=CARTESIAN_POINT('Ctrl Pts',(2.3929117136618,-1.71218777660562,8.57894808397194));
#99493=CARTESIAN_POINT('Ctrl Pts',(2.42018334642052,-1.67341513665586,8.58152542897416));
#99494=CARTESIAN_POINT('Ctrl Pts',(2.44648026422972,-1.63404354799206,8.58410277397638));
#99495=CARTESIAN_POINT('Ctrl Pts',(2.49802696192011,-1.55686813933131,8.58915483462612));
#99496=CARTESIAN_POINT('Ctrl Pts',(2.54601089762617,-1.47711256605875,8.59420689527585));
#99497=CARTESIAN_POINT('Ctrl Pts',(2.59016389066404,-1.39513978493201,8.59925895592559));
#99498=CARTESIAN_POINT('Ctrl Pts',(2.63425594728163,-1.31328013606424,8.60430404412635));
#99499=CARTESIAN_POINT('Ctrl Pts',(2.67452735859163,-1.22920974772194,8.60934913232711));
#99500=CARTESIAN_POINT('Ctrl Pts',(2.71075292990872,-1.14332084429144,8.61439422052787));
#99501=CARTESIAN_POINT('Ctrl Pts',(2.74693970157195,-1.05752393277721,8.61943390515131));
#99502=CARTESIAN_POINT('Ctrl Pts',(2.77908907461641,-0.969912784751068,
8.62447358977474));
#99503=CARTESIAN_POINT('Ctrl Pts',(2.80702207324564,-0.880903559030014,
8.62951327439817));
#99504=CARTESIAN_POINT('Ctrl Pts',(2.8349349126046,-0.791958571347312,8.63454932187667));
#99505=CARTESIAN_POINT('Ctrl Pts',(2.85863729319264,-0.701617934177094,
8.63958536935518));
#99506=CARTESIAN_POINT('Ctrl Pts',(2.8779990012029,-0.610316105862478,8.64462141683368));
#99507=CARTESIAN_POINT('Ctrl Pts',(2.8973536571618,-0.519047532113093,8.64965563004914));
#99508=CARTESIAN_POINT('Ctrl Pts',(2.91237068925402,-0.426818896907573,
8.6546898432646));
#99509=CARTESIAN_POINT('Ctrl Pts',(2.92297049446232,-0.334077069705039,
8.65972405648006));
#99510=CARTESIAN_POINT('Ctrl Pts',(2.9335694049318,-0.241343070921145,8.66475784475319));
#99511=CARTESIAN_POINT('Ctrl Pts',(2.93975177957361,-0.14809640771684,8.66979163302631));
#99512=CARTESIAN_POINT('Ctrl Pts',(2.94148976463434,-0.0547901866340656,
8.67482542129943));
#99513=CARTESIAN_POINT('Ctrl Pts',(2.94322808930017,0.0385342666353106,
8.67986019318294));
#99514=CARTESIAN_POINT('Ctrl Pts',(2.94052029175772,0.13191785668895,8.68489496506644));
#99515=CARTESIAN_POINT('Ctrl Pts',(2.93339063425293,0.224907507382898,8.68992973694994));
#99516=CARTESIAN_POINT('Ctrl Pts',(2.92625313858892,0.317999388469715,8.69497004393013));
#99517=CARTESIAN_POINT('Ctrl Pts',(2.91468411325629,0.41069602201003,8.70001035091032));
#99518=CARTESIAN_POINT('Ctrl Pts',(2.89875968411325,0.502549792318768,8.70505065789051));
#99519=CARTESIAN_POINT('Ctrl Pts',(2.88282547637173,0.594459966604765,8.71009405993538));
#99520=CARTESIAN_POINT('Ctrl Pts',(2.86253063701528,0.685525813932192,8.71513746198024));
#99521=CARTESIAN_POINT('Ctrl Pts',(2.83800188406911,0.775312392536198,8.72018086402512));
#99522=CARTESIAN_POINT('Ctrl Pts',(2.8134333555363,0.865244568180685,8.72523244440157));
#99523=CARTESIAN_POINT('Ctrl Pts',(2.78461734403574,0.953892911672233,8.73028402477803));
#99524=CARTESIAN_POINT('Ctrl Pts',(2.75172957247402,1.04084021827174,8.73533560515448));
#99525=CARTESIAN_POINT('Ctrl Pts',(2.73495004461305,1.08520122797968,8.7379129501567));
#99526=CARTESIAN_POINT('Ctrl Pts',(2.7171113578613,1.12911979827709,8.74049029515891));
#99527=CARTESIAN_POINT('Ctrl Pts',(2.69824144008475,1.17254301883102,8.74306764016113));
#99528=CARTESIAN_POINT('Ctrl Pts',(2.66125300082632,1.25766035611273,8.74811970081085));
#99529=CARTESIAN_POINT('Ctrl Pts',(2.6201665468077,1.34117869451823,8.75317176146058));
#99530=CARTESIAN_POINT('Ctrl Pts',(2.57514209313475,1.42267607000525,8.75822382211031));
#99531=CARTESIAN_POINT('Ctrl Pts',(2.53017977860204,1.50406096935028,8.76326891031107));
#99532=CARTESIAN_POINT('Ctrl Pts',(2.48129047722312,1.58343006267773,8.76831399851184));
#99533=CARTESIAN_POINT('Ctrl Pts',(2.42868208167767,1.66038168688341,8.7733590867126));
#99534=CARTESIAN_POINT('Ctrl Pts',(2.37613003272558,1.73725089150886,8.77839877133604));
#99535=CARTESIAN_POINT('Ctrl Pts',(2.31986705651522,1.81170740870906,8.78343845595948));
#99536=CARTESIAN_POINT('Ctrl Pts',(2.26014618899899,1.88337548151009,8.78847814058292));
#99537=CARTESIAN_POINT('Ctrl Pts',(2.20046842208674,1.95499183139829,8.79351418806142));
#99538=CARTESIAN_POINT('Ctrl Pts',(2.13733800774534,2.02382339650421,8.79855023553992));
#99539=CARTESIAN_POINT('Ctrl Pts',(2.07104976382865,2.08952551449971,8.80358628301842));
#99540=CARTESIAN_POINT('Ctrl Pts',(2.00478566386137,2.15520370202852,8.80862049623388));
#99541=CARTESIAN_POINT('Ctrl Pts',(1.93536633447734,2.21775439437172,8.81365470944934));
#99542=CARTESIAN_POINT('Ctrl Pts',(1.86312442507697,2.27686876580132,8.8186889226648));
#99543=CARTESIAN_POINT('Ctrl Pts',(1.7908886136794,2.33597814733508,8.82372271093792));
#99544=CARTESIAN_POINT('Ctrl Pts',(1.71583103993865,2.39165150343185,8.82875649921104));
#99545=CARTESIAN_POINT('Ctrl Pts',(1.63831760978349,2.44362014426819,8.83379028748416));
#99546=CARTESIAN_POINT('Ctrl Pts',(1.56078903337859,2.49559893986109,8.83882505936766));
#99547=CARTESIAN_POINT('Ctrl Pts',(1.48080401674281,2.5438713354159,8.84385983125116));
#99548=CARTESIAN_POINT('Ctrl Pts',(1.39875665099451,2.58821247800458,8.84889460313465));
#99549=CARTESIAN_POINT('Ctrl Pts',(1.31661908451552,2.63260236808717,8.85393491011484));
#99550=CARTESIAN_POINT('Ctrl Pts',(1.23241503460177,2.67305216654127,8.85897521709503));
#99551=CARTESIAN_POINT('Ctrl Pts',(1.1465620752108,2.70938358445022,8.86401552407522));
#99552=CARTESIAN_POINT('Ctrl Pts',(1.0606563967169,2.74573731212896,8.86905892612009));
#99553=CARTESIAN_POINT('Ctrl Pts',(0.973100209637635,2.77796747126774,8.87410232816496));
#99554=CARTESIAN_POINT('Ctrl Pts',(0.884327817268211,2.80594517259437,8.87914573020983));
#99555=CARTESIAN_POINT('Ctrl Pts',(0.795411472452718,2.83396824228872,8.88419731058629));
#99556=CARTESIAN_POINT('Ctrl Pts',(0.705275414195521,2.85772497448137,8.88924889096275));
#99557=CARTESIAN_POINT('Ctrl Pts',(0.614365558734634,2.87713728560885,8.89430047133921));
#99558=CARTESIAN_POINT('Ctrl Pts',(0.567982834089371,2.88704155701254,8.89687781634143));
#99559=CARTESIAN_POINT('Ctrl Pts',(0.521398793615352,2.89581576553078,8.89945516134366));
#99560=CARTESIAN_POINT('Ctrl Pts',(0.474673043194979,2.90345475288733,8.90203250634588));
#99561=CARTESIAN_POINT('Ctrl Pts',(0.383082152249367,2.9184285446748,8.90708456699561));
#99562=CARTESIAN_POINT('Ctrl Pts',(0.290617456125183,2.92909107366691,8.91213662764533));
#99563=CARTESIAN_POINT('Ctrl Pts',(0.197720370061504,2.93534847254338,8.91718868829506));
#99564=CARTESIAN_POINT('Ctrl Pts',(0.10495149310619,2.94159723545973,8.92223377649582));
#99565=CARTESIAN_POINT('Ctrl Pts',(0.0117518514684078,2.94345291957198,
8.92727886469659));
#99566=CARTESIAN_POINT('Ctrl Pts',(-0.0814282926911858,2.94087290326349,
8.93232395289735));
#99567=CARTESIAN_POINT('Ctrl Pts',(-0.174508635599422,2.93829565029967,
8.93736363752078));
#99568=CARTESIAN_POINT('Ctrl Pts',(-0.267569080796354,2.93129215222189,
8.9424033221442));
#99569=CARTESIAN_POINT('Ctrl Pts',(-0.360156712281988,2.9198717681772,8.94744300676762));
#99570=CARTESIAN_POINT('Ctrl Pts',(-0.452677523190822,2.90845962623393,
8.95247905424613));
#99571=CARTESIAN_POINT('Ctrl Pts',(-0.544725758939587,2.89263698848272,
8.95751510172463));
#99572=CARTESIAN_POINT('Ctrl Pts',(-0.63585203185653,2.87246517708813,8.96255114920313));
#99573=CARTESIAN_POINT('Ctrl Pts',(-0.72694511415023,2.85230071280618,8.9675853624186));
#99574=CARTESIAN_POINT('Ctrl Pts',(-0.817116467355787,2.82779031774977,
8.97261957563406));
#99575=CARTESIAN_POINT('Ctrl Pts',(-0.905926357638238,2.79904652239585,
8.97765378884953));
#99576=CARTESIAN_POINT('Ctrl Pts',(-0.994728751400297,2.7703051533308,8.98268757712266));
#99577=CARTESIAN_POINT('Ctrl Pts',(-1.08216948807129,2.73733123143188,8.98772136539578));
#99578=CARTESIAN_POINT('Ctrl Pts',(-1.16782457910494,2.70028697594133,8.99275515366891));
#99579=CARTESIAN_POINT('Ctrl Pts',(-1.25349640728163,2.66323548194347,8.99778992555239));
#99580=CARTESIAN_POINT('Ctrl Pts',(-1.3373814892415,2.62211225148476,9.00282469743588));
#99581=CARTESIAN_POINT('Ctrl Pts',(-1.41907743876359,2.57712693183556,9.00785946931936));
#99582=CARTESIAN_POINT('Ctrl Pts',(-1.50086320267885,2.53209215650087,9.01289977629955));
#99583=CARTESIAN_POINT('Ctrl Pts',(-1.58045464032414,2.48318703130501,9.01794008327975));
#99584=CARTESIAN_POINT('Ctrl Pts',(-1.65747580624598,2.43066615389881,9.02298039025994));
#99585=CARTESIAN_POINT('Ctrl Pts',(-1.7345442679953,2.37811302537921,9.0280237923048));
#99586=CARTESIAN_POINT('Ctrl Pts',(-1.80903896143313,2.32193999178175,9.03306719434966));
#99587=CARTESIAN_POINT('Ctrl Pts',(-1.88061642186181,2.26244245757183,9.03811059639453));
#99588=CARTESIAN_POINT('Ctrl Pts',(-1.95230995160258,2.20284844274043,9.04316217677098));
#99589=CARTESIAN_POINT('Ctrl Pts',(-2.0210764769293,2.13991946438324,9.04821375714744));
#99590=CARTESIAN_POINT('Ctrl Pts',(-2.08660896569403,2.0739881928992,9.05326533752389));
#99591=CARTESIAN_POINT('Ctrl Pts',(-2.12004401370196,2.04034968368269,9.05584268252614));
#99592=CARTESIAN_POINT('Ctrl Pts',(-2.15263785010515,2.0059301922487,9.05842002752838));
#99593=CARTESIAN_POINT('Ctrl Pts',(-2.18435387262118,1.97077704450931,9.06099737253063));
#99594=CARTESIAN_POINT('Ctrl Pts',(-2.24587576570944,1.90258790774585,9.06599683750452));
#99595=CARTESIAN_POINT('Ctrl Pts',(-2.304323743165,1.83137957052598,9.0709963024784));
#99596=CARTESIAN_POINT('Ctrl Pts',(-2.35938251168991,1.75746355965972,9.07599576745229));
#99597=CARTESIAN_POINT('Ctrl Pts',(-2.41437124025441,1.68364157694944,9.08098887263393));
#99598=CARTESIAN_POINT('Ctrl Pts',(-2.46597904899703,1.60711911752429,9.08598197781558));
#99599=CARTESIAN_POINT('Ctrl Pts',(-2.51392844109951,1.52824336839097,9.09097508299722));
#99600=CARTESIAN_POINT('Ctrl Pts',(-2.56183092720743,1.44944477863962,9.09596330372561));
#99601=CARTESIAN_POINT('Ctrl Pts',(-2.60608186788051,1.36829785550792,9.10095152445399));
#99602=CARTESIAN_POINT('Ctrl Pts',(-2.64644571237268,1.28518056764964,9.10593974518238));
#99603=CARTESIAN_POINT('Ctrl Pts',(-2.68678192713052,1.2021201749809,9.1109245513893));
#99604=CARTESIAN_POINT('Ctrl Pts',(-2.72323613318865,1.11709250390312,9.11590935759621));
#99605=CARTESIAN_POINT('Ctrl Pts',(-2.75561822778716,1.03050093774199,9.12089416380313));
#99606=CARTESIAN_POINT('Ctrl Pts',(-2.78799587501206,0.94392126411135,9.12587828539419));
#99607=CARTESIAN_POINT('Ctrl Pts',(-2.81630234981916,0.855778542245091,
9.13086240698524));
#99608=CARTESIAN_POINT('Ctrl Pts',(-2.84039569224437,0.766496126200019,
9.1358465285763));
#99609=CARTESIAN_POINT('Ctrl Pts',(-2.86448612171046,0.677224504673327,
9.14083004757174));
#99610=CARTESIAN_POINT('Ctrl Pts',(-2.88436431870589,0.586813903109782,
9.14581356656718));
#99611=CARTESIAN_POINT('Ctrl Pts',(-2.8999386703983,0.495701228492089,9.15079708556263));
#99612=CARTESIAN_POINT('Ctrl Pts',(-2.9155237877027,0.404525573165936,9.15578404936483));
#99613=CARTESIAN_POINT('Ctrl Pts',(-2.92679904500027,0.312647324569952,
9.16077101316702));
#99614=CARTESIAN_POINT('Ctrl Pts',(-2.93372438166545,0.220511343068046,
9.16575797696922));
#99615=CARTESIAN_POINT('Ctrl Pts',(-2.93930964116251,0.146204000250804,
9.16977994561628));
#99616=CARTESIAN_POINT('Ctrl Pts',(-2.94206654305182,0.0717292485551678,
9.17380191426335));
#99617=CARTESIAN_POINT('Ctrl Pts',(-2.94199878001913,-0.00267924727273255,
9.17782388291041));
#99618=CARTESIAN_POINT('',(-2.941999963151,0.000465638797190243,10.1778238829398));
#99619=CARTESIAN_POINT('Ctrl Pts',(-2.94199878001864,-0.00267924781502314,
9.17782388293972));
#99620=CARTESIAN_POINT('Ctrl Pts',(-2.94189214524261,-0.119771582166532,
9.18415302173411));
#99621=CARTESIAN_POINT('Ctrl Pts',(-2.93479142724456,-0.236551798411417,
9.19048216052851));
#99622=CARTESIAN_POINT('Ctrl Pts',(-2.92082967268118,-0.352303879037908,
9.19681129932291));
#99623=CARTESIAN_POINT('Ctrl Pts',(-2.90659295952955,-0.470335546268701,
9.20326508227));
#99624=CARTESIAN_POINT('Ctrl Pts',(-2.8852223297207,-0.587298377518235,
9.20971886521709));
#99625=CARTESIAN_POINT('Ctrl Pts',(-2.85690708185129,-0.70245706322021,
9.21617264816419));
#99626=CARTESIAN_POINT('Ctrl Pts',(-2.85136494753718,-0.724997035553822,
9.21743584501458));
#99627=CARTESIAN_POINT('Ctrl Pts',(-2.84555690974658,-0.747467957434179,
9.21869904186498));
#99628=CARTESIAN_POINT('Ctrl Pts',(-2.83948459964082,-0.769864409102424,
9.21996223871538));
#99629=CARTESIAN_POINT('Ctrl Pts',(-2.81519885278461,-0.859437330481364,
9.22501429936511));
#99630=CARTESIAN_POINT('Ctrl Pts',(-2.78662687917521,-0.94802091743699,
9.23006636001484));
#99631=CARTESIAN_POINT('Ctrl Pts',(-2.75386596675008,-1.03517449600328,
9.23511842066457));
#99632=CARTESIAN_POINT('Ctrl Pts',(-2.72115026830903,-1.12220779218968,
9.24016350886534));
#99633=CARTESIAN_POINT('Ctrl Pts',(-2.68425727404025,-1.20781458945974,
9.24520859706611));
#99634=CARTESIAN_POINT('Ctrl Pts',(-2.64333458266587,-1.29156737496835,
9.25025368526688));
#99635=CARTESIAN_POINT('Ctrl Pts',(-2.60245572182898,-1.37523045646481,
9.25529336989032));
#99636=CARTESIAN_POINT('Ctrl Pts',(-2.55755593663263,-1.45704307612064,
9.26033305451376));
#99637=CARTESIAN_POINT('Ctrl Pts',(-2.50883124192735,-1.53659682400078,
9.2653727391372));
#99638=CARTESIAN_POINT('Ctrl Pts',(-2.46014171187815,-1.61609315786937,
9.2704087866157));
#99639=CARTESIAN_POINT('Ctrl Pts',(-2.40763299045645,-1.69333348247071,
9.2754448340942));
#99640=CARTESIAN_POINT('Ctrl Pts',(-2.35154693323202,-1.76793411099143,
9.28048088157271));
#99641=CARTESIAN_POINT('Ctrl Pts',(-2.29548130404812,-1.8425075679701,9.28551509478817));
#99642=CARTESIAN_POINT('Ctrl Pts',(-2.2358411942451,-1.91444288410493,9.29054930800362));
#99643=CARTESIAN_POINT('Ctrl Pts',(-2.17291107731279,-1.98338635925817,
9.29558352121908));
#99644=CARTESIAN_POINT('Ctrl Pts',(-2.1099862723666,-2.05232401483247,9.30061730949221));
#99645=CARTESIAN_POINT('Ctrl Pts',(-2.04377231210823,-2.11827000350394,
9.30565109776534));
#99646=CARTESIAN_POINT('Ctrl Pts',(-1.97459238301976,-2.1809055277385,9.31068488603846));
#99647=CARTESIAN_POINT('Ctrl Pts',(-1.90539893606111,-2.24355329105593,
9.31571965792197));
#99648=CARTESIAN_POINT('Ctrl Pts',(-1.83323869886711,-2.30288900734021,
9.32075442980548));
#99649=CARTESIAN_POINT('Ctrl Pts',(-1.75846908832904,-2.35863317737016,
9.32578920168899));
#99650=CARTESIAN_POINT('Ctrl Pts',(-1.68361727803433,-2.41443863108444,
9.33082950866918));
#99651=CARTESIAN_POINT('Ctrl Pts',(-1.60615072490937,-2.46664439095639,
9.33586981564937));
#99652=CARTESIAN_POINT('Ctrl Pts',(-1.52645681789169,-2.51501363477656,
9.34091012262956));
#99653=CARTESIAN_POINT('Ctrl Pts',(-1.44671397381565,-2.56341258034679,
9.34595352467444));
#99654=CARTESIAN_POINT('Ctrl Pts',(-1.36474144303353,-2.60797010778216,
9.35099692671931));
#99655=CARTESIAN_POINT('Ctrl Pts',(-1.28095031429092,-2.64849585469149,
9.35604032876418));
#99656=CARTESIAN_POINT('Ctrl Pts',(-1.19702331067083,-2.68908731775692,
9.36109190914064));
#99657=CARTESIAN_POINT('Ctrl Pts',(-1.11127222992197,-2.72563377412438,
9.3661434895171));
#99658=CARTESIAN_POINT('Ctrl Pts',(-1.02412700143469,-2.75799345266307,
9.37119506989356));
#99659=CARTESIAN_POINT('Ctrl Pts',(-0.979665010855948,-2.77450354446379,
9.37377241489575));
#99660=CARTESIAN_POINT('Ctrl Pts',(-0.934840340388964,-2.78992458461901,
9.37634975989794));
#99661=CARTESIAN_POINT('Ctrl Pts',(-0.889711222666078,-2.80424284616401,
9.37892710490012));
#99662=CARTESIAN_POINT('Ctrl Pts',(-0.801250019524294,-2.8323092189867,
9.38397916554985));
#99663=CARTESIAN_POINT('Ctrl Pts',(-0.711300509577873,-2.85623609120711,
9.38903122619958));
#99664=CARTESIAN_POINT('Ctrl Pts',(-0.620285885191738,-2.87586672511643,
9.39408328684931));
#99665=CARTESIAN_POINT('Ctrl Pts',(-0.529396871891344,-2.89547026639909,
9.39912837505008));
#99666=CARTESIAN_POINT('Ctrl Pts',(-0.437446095727711,-2.91078925878916,
9.40417346325084));
#99667=CARTESIAN_POINT('Ctrl Pts',(-0.344872916438735,-2.92171639135407,
9.40921855145161));
#99668=CARTESIAN_POINT('Ctrl Pts',(-0.252398888306911,-2.93263182033651,
9.41425823607504));
#99669=CARTESIAN_POINT('Ctrl Pts',(-0.159304220935015,-2.93916468743556,
9.41929792069848));
#99670=CARTESIAN_POINT('Ctrl Pts',(-0.06603841983787,-2.94125873175165,
9.42433760532191));
#99671=CARTESIAN_POINT('Ctrl Pts',(0.0271600712465363,-2.94335126479407,
9.42937365280041));
#99672=CARTESIAN_POINT('Ctrl Pts',(0.120529007658576,-2.94101133250171,
9.43440970027891));
#99673=CARTESIAN_POINT('Ctrl Pts',(0.213614857808199,-2.93423460079858,
9.43944574775741));
#99674=CARTESIAN_POINT('Ctrl Pts',(0.306666803604203,-2.92746033736218,
9.44447996097287));
#99675=CARTESIAN_POINT('Ctrl Pts',(0.399435425289394,-2.91625251708545,
9.44951417418833));
#99676=CARTESIAN_POINT('Ctrl Pts',(0.491469335450193,-2.9006588721034,9.45454838740379));
#99677=CARTESIAN_POINT('Ctrl Pts',(0.583495476948213,-2.88506654339455,
9.45958217567691));
#99678=CARTESIAN_POINT('Ctrl Pts',(0.674786592197164,-2.86508920043962,
9.46461596395003));
#99679=CARTESIAN_POINT('Ctrl Pts',(0.76489968515994,-2.84082601924902,9.46964975222316));
#99680=CARTESIAN_POINT('Ctrl Pts',(0.855030386367092,-2.8165580969935,9.47468452410666));
#99681=CARTESIAN_POINT('Ctrl Pts',(0.943982179233714,-2.78800278917391,
9.47971929599017));
#99682=CARTESIAN_POINT('Ctrl Pts',(1.03132658157492,-2.75530932603528,9.48475406787368));
#99683=CARTESIAN_POINT('Ctrl Pts',(1.11876700807031,-2.72257992055734,9.48979437485387));
#99684=CARTESIAN_POINT('Ctrl Pts',(1.20459609988353,-2.68570343461613,9.49483468183406));
#99685=CARTESIAN_POINT('Ctrl Pts',(1.28840503465784,-2.64487740106575,9.49987498881425));
#99686=CARTESIAN_POINT('Ctrl Pts',(1.37226543337574,-2.60402629776961,9.50491839085912));
#99687=CARTESIAN_POINT('Ctrl Pts',(1.45410281602812,-2.55922103184496,9.50996179290399));
#99688=CARTESIAN_POINT('Ctrl Pts',(1.53353459597083,-2.51070421255882,9.51500519494886));
#99689=CARTESIAN_POINT('Ctrl Pts',(1.61309518171351,-2.46210871887151,9.52005677532532));
#99690=CARTESIAN_POINT('Ctrl Pts',(1.69024200976055,-2.40978990538259,9.52510835570178));
#99691=CARTESIAN_POINT('Ctrl Pts',(1.76462315164894,-2.35403252582978,9.53015993607824));
#99692=CARTESIAN_POINT('Ctrl Pts',(1.80257283274249,-2.32558479406713,9.53273728108045));
#99693=CARTESIAN_POINT('Ctrl Pts',(1.83980313298703,-2.29624260080055,9.53531462608267));
#99694=CARTESIAN_POINT('Ctrl Pts',(1.87627098868146,-2.26604747898897,9.53789197108488));
#99695=CARTESIAN_POINT('Ctrl Pts',(1.94775455746084,-2.20685959898569,9.54294403173461));
#99696=CARTESIAN_POINT('Ctrl Pts',(2.01656316091093,-2.1441795730994,9.54799609238434));
#99697=CARTESIAN_POINT('Ctrl Pts',(2.08233593309237,-2.07827838889605,9.55304815303407));
#99698=CARTESIAN_POINT('Ctrl Pts',(2.14801793096823,-2.01246815622223,9.55809324123484));
#99699=CARTESIAN_POINT('Ctrl Pts',(2.21067211210061,-1.94344591088365,9.56313832943561));
#99700=CARTESIAN_POINT('Ctrl Pts',(2.26997041831439,-1.87152298943336,9.56818341763638));
#99701=CARTESIAN_POINT('Ctrl Pts',(2.32920521265868,-1.79967710153584,9.57322310225981));
#99702=CARTESIAN_POINT('Ctrl Pts',(2.38509099522403,-1.72493705368548,9.57826278688325));
#99703=CARTESIAN_POINT('Ctrl Pts',(2.43733714000599,-1.64765034699338,9.58330247150668));
#99704=CARTESIAN_POINT('Ctrl Pts',(2.48954557869818,-1.57041941818715,9.58833851898518));
#99705=CARTESIAN_POINT('Ctrl Pts',(2.53811935247468,-1.49064585069163,9.59337456646368));
#99706=CARTESIAN_POINT('Ctrl Pts',(2.58280931736585,-1.40870863918986,9.59841061394218));
#99707=CARTESIAN_POINT('Ctrl Pts',(2.6274830049778,-1.32680127140968,9.60344482715764));
#99708=CARTESIAN_POINT('Ctrl Pts',(2.6682754813901,-1.24273221483784,9.60847904037309));
#99709=CARTESIAN_POINT('Ctrl Pts',(2.7049825418681,-1.15690684507821,9.61351325358855));
#99710=CARTESIAN_POINT('Ctrl Pts',(2.74168650387106,-1.07108871991301,9.61854704186167));
#99711=CARTESIAN_POINT('Ctrl Pts',(2.77430556103156,-0.983514984895593,
9.6235808301348));
#99712=CARTESIAN_POINT('Ctrl Pts',(2.80268330622685,-0.894611806873418,
9.62861461840792));
#99713=CARTESIAN_POINT('Ctrl Pts',(2.83106659647952,-0.805691257026247,
9.63364939029142));
#99714=CARTESIAN_POINT('Ctrl Pts',(2.85520679410711,-0.715441171611568,
9.63868416217493));
#99715=CARTESIAN_POINT('Ctrl Pts',(2.87499743529214,-0.624302608567035,
9.64371893405843));
#99716=CARTESIAN_POINT('Ctrl Pts',(2.8948098337911,-0.533063850167109,9.64875924103862));
#99717=CARTESIAN_POINT('Ctrl Pts',(2.91026303636294,-0.440935099241388,
9.65379954801881));
#99718=CARTESIAN_POINT('Ctrl Pts',(2.92130183523695,-0.348367029784977,
9.658839854999));
#99719=CARTESIAN_POINT('Ctrl Pts',(2.93234741262598,-0.255742117726806,
9.66388325704388));
#99720=CARTESIAN_POINT('Ctrl Pts',(2.93897315828224,-0.162677792937583,
9.66892665908875));
#99721=CARTESIAN_POINT('Ctrl Pts',(2.94117596738647,-0.0696270699389575,
9.67397006113362));
#99722=CARTESIAN_POINT('Ctrl Pts',(2.94338234854446,0.0235745432049082,
9.67902164151007));
#99723=CARTESIAN_POINT('Ctrl Pts',(2.94115148528214,0.116762066896197,9.68407322188653));
#99724=CARTESIAN_POINT('Ctrl Pts',(2.93453230439372,0.209485451689823,9.68912480226299));
#99725=CARTESIAN_POINT('Ctrl Pts',(2.93115516070598,0.256793449301686,9.6917021472652));
#99726=CARTESIAN_POINT('Ctrl Pts',(2.92663652552509,0.303980751598852,9.69427949226741));
#99727=CARTESIAN_POINT('Ctrl Pts',(2.92098801012808,0.3509886674638,9.69685683726962));
#99728=CARTESIAN_POINT('Ctrl Pts',(2.9099159020703,0.443132653528412,9.70190889791935));
#99729=CARTESIAN_POINT('Ctrl Pts',(2.89445953293827,0.534917784171193,9.70696095856908));
#99730=CARTESIAN_POINT('Ctrl Pts',(2.87465141666587,0.625893946815999,9.71201301921881));
#99731=CARTESIAN_POINT('Ctrl Pts',(2.85487063796707,0.716744551456834,9.71705810741957));
#99732=CARTESIAN_POINT('Ctrl Pts',(2.8307501403396,0.806787976309188,9.72210319562034));
#99733=CARTESIAN_POINT('Ctrl Pts',(2.80237412322733,0.895579853204544,9.7271482838211));
#99734=CARTESIAN_POINT('Ctrl Pts',(2.77402849844848,0.984276628933381,9.73218796844454));
#99735=CARTESIAN_POINT('Ctrl Pts',(2.74143654819952,1.07172410016375,9.73722765306797));
#99736=CARTESIAN_POINT('Ctrl Pts',(2.7047331422842,1.15748979651202,9.74226733769141));
#99737=CARTESIAN_POINT('Ctrl Pts',(2.66805622525,1.24319359567996,9.74730338516991));
#99738=CARTESIAN_POINT('Ctrl Pts',(2.62727392464204,1.32721762514166,9.75233943264841));
#99739=CARTESIAN_POINT('Ctrl Pts',(2.58257004536095,1.40914724596273,9.75737548012691));
#99740=CARTESIAN_POINT('Ctrl Pts',(2.53788244842707,1.49104702582694,9.76240969334237));
#99741=CARTESIAN_POINT('Ctrl Pts',(2.48927632295869,1.57085352287876,9.76744390655783));
#99742=CARTESIAN_POINT('Ctrl Pts',(2.43698198151407,1.64817560404701,9.77247811977329));
#99743=CARTESIAN_POINT('Ctrl Pts',(2.38469205428051,1.72549115839084,9.77751190804642));
#99744=CARTESIAN_POINT('Ctrl Pts',(2.32871477911046,1.80032234586958,9.78254569631954));
#99745=CARTESIAN_POINT('Ctrl Pts',(2.26932382353795,1.87230696840104,9.78757948459266));
#99746=CARTESIAN_POINT('Ctrl Pts',(2.20992126287648,1.9443056568444,9.79261425647617));
#99747=CARTESIAN_POINT('Ctrl Pts',(2.14710398010003,2.01345633322179,9.79764902835968));
#99748=CARTESIAN_POINT('Ctrl Pts',(2.08118519819989,2.07943073238655,9.80268380024319));
#99749=CARTESIAN_POINT('Ctrl Pts',(2.01519394691296,2.14547766208227,9.80772410722339));
#99750=CARTESIAN_POINT('Ctrl Pts',(1.9460947048205,2.20834102946829,9.81276441420358));
#99751=CARTESIAN_POINT('Ctrl Pts',(1.87423652558705,2.26773046153095,9.81780472118377));
#99752=CARTESIAN_POINT('Ctrl Pts',(1.80233422092363,2.32715636243061,9.82284812322864));
#99753=CARTESIAN_POINT('Ctrl Pts',(1.72766996168055,2.38310381497015,9.82789152527352));
#99754=CARTESIAN_POINT('Ctrl Pts',(1.65062297318189,2.43532498866254,9.83293492731839));
#99755=CARTESIAN_POINT('Ctrl Pts',(1.57345104603785,2.48763084370106,9.83798650769485));
#99756=CARTESIAN_POINT('Ctrl Pts',(1.49388905472915,2.53619812550275,9.84303808807131));
#99757=CARTESIAN_POINT('Ctrl Pts',(1.41234189653937,2.58082435808398,9.84808966844777));
#99758=CARTESIAN_POINT('Ctrl Pts',(1.37073607322446,2.60359291543411,9.85066701344997));
#99759=CARTESIAN_POINT('Ctrl Pts',(1.3286138363626,2.62533634487202,9.85324435845217));
#99760=CARTESIAN_POINT('Ctrl Pts',(1.28603082018315,2.6460326395453,9.85582170345437));
#99761=CARTESIAN_POINT('Ctrl Pts',(1.20256043488224,2.68660110664024,9.8608737641041));
#99762=CARTESIAN_POINT('Ctrl Pts',(1.11701855354975,2.72328892603511,9.86592582475383));
#99763=CARTESIAN_POINT('Ctrl Pts',(1.02980124215722,2.75587978722793,9.87097788540356));
#99764=CARTESIAN_POINT('Ctrl Pts',(0.942704301103581,2.78842566912772,9.87602297360433));
#99765=CARTESIAN_POINT('Ctrl Pts',(0.853936937372214,2.81688567441796,9.88106806180509));
#99766=CARTESIAN_POINT('Ctrl Pts',(0.763918364614622,2.84109006055854,9.88611315000585));
#99767=CARTESIAN_POINT('Ctrl Pts',(0.673996206884852,2.86526852242048,9.89115283462929));
#99768=CARTESIAN_POINT('Ctrl Pts',(0.582825930556004,2.88520031009069,9.89619251925272));
#99769=CARTESIAN_POINT('Ctrl Pts',(0.49084417353772,2.90076472629272,9.90123220387616));
#99770=CARTESIAN_POINT('Ctrl Pts',(0.398928799836315,2.91631790964156,9.90626825135466));
#99771=CARTESIAN_POINT('Ctrl Pts',(0.306203546308772,2.92750991250561,9.91130429883316));
#99772=CARTESIAN_POINT('Ctrl Pts',(0.213116546639057,2.93427083575267,9.91634034631166));
#99773=CARTESIAN_POINT('Ctrl Pts',(0.120063451741682,2.94102929649084,9.92137455952712));
#99774=CARTESIAN_POINT('Ctrl Pts',(0.0266493151385261,2.94335985166373,
9.92640877274257));
#99775=CARTESIAN_POINT('Ctrl Pts',(-0.0666723188913893,2.94124443083088,
9.93144298595803));
#99776=CARTESIAN_POINT('Ctrl Pts',(-0.159986075560635,2.93912918856254,
9.93647677423115));
#99777=CARTESIAN_POINT('Ctrl Pts',(-0.253206900996718,2.93256872669209,
9.94151056250427));
#99778=CARTESIAN_POINT('Ctrl Pts',(-0.345882111839208,2.92159709143983,
9.9465443507774));
#99779=CARTESIAN_POINT('Ctrl Pts',(-0.438575431567919,2.91062331231228,
9.9515791226609));
#99780=CARTESIAN_POINT('Ctrl Pts',(-0.530722483815477,2.89523670056958,
9.95661389454439));
#99781=CARTESIAN_POINT('Ctrl Pts',(-0.62187770524449,2.87552292978509,9.96164866642789));
#99782=CARTESIAN_POINT('Ctrl Pts',(-0.713133140342792,2.85578748619597,
9.96668897340808));
#99783=CARTESIAN_POINT('Ctrl Pts',(-0.803394133122073,2.83171548172278,
9.97172928038827));
#99784=CARTESIAN_POINT('Ctrl Pts',(-0.892227585511837,2.80344322854088,
9.97676958736846));
#99785=CARTESIAN_POINT('Ctrl Pts',(-0.981115587214204,2.77515361442191,
9.98181298941333));
#99786=CARTESIAN_POINT('Ctrl Pts',(-1.06857388721276,2.74265877151817,9.98685639145821));
#99787=CARTESIAN_POINT('Ctrl Pts',(-1.1541888261347,2.70614340965622,9.99189979350308));
#99788=CARTESIAN_POINT('Ctrl Pts',(-1.23994259740693,2.66956883483947,9.99695137387954));
#99789=CARTESIAN_POINT('Ctrl Pts',(-1.32384664060778,2.62896091865108,10.002002954256));
#99790=CARTESIAN_POINT('Ctrl Pts',(-1.40551153516136,2.58455050725041,10.0070545346325));
#99791=CARTESIAN_POINT('Ctrl Pts',(-1.44717742823815,2.56189206309235,10.0096318796347));
#99792=CARTESIAN_POINT('Ctrl Pts',(-1.48826090623292,2.53824449666673,10.0122092246369));
#99793=CARTESIAN_POINT('Ctrl Pts',(-1.52871335004053,2.51364267416987,10.0147865696391));
#99794=CARTESIAN_POINT('Ctrl Pts',(-1.60800742955645,2.46541866875304,10.0198386302888));
#99795=CARTESIAN_POINT('Ctrl Pts',(-1.68515987810307,2.41335227616514,10.0248906909386));
#99796=CARTESIAN_POINT('Ctrl Pts',(-1.75977442314413,2.35765942825671,10.0299427515883));
#99797=CARTESIAN_POINT('Ctrl Pts',(-1.83428599117365,2.3020434431508,10.0349878397891));
#99798=CARTESIAN_POINT('Ctrl Pts',(-1.90626626284834,2.2428112115994,10.0400329279898));
#99799=CARTESIAN_POINT('Ctrl Pts',(-1.97534559114506,2.18022333616164,10.0450780161906));
#99800=CARTESIAN_POINT('Ctrl Pts',(-2.04435093153967,2.11770249590958,10.050117700814));
#99801=CARTESIAN_POINT('Ctrl Pts',(-2.11046117683206,2.05183345224717,10.0551573854375));
#99802=CARTESIAN_POINT('Ctrl Pts',(-2.17333848661742,1.98291800702588,10.0601970700609));
#99803=CARTESIAN_POINT('Ctrl Pts',(-2.23617041779166,1.91405229814351,10.0652331175394));
#99804=CARTESIAN_POINT('Ctrl Pts',(-2.29577375243484,1.84214488497022,10.0702691650179));
#99805=CARTESIAN_POINT('Ctrl Pts',(-2.35184713975556,1.76753473267814,10.0753052124964));
#99806=CARTESIAN_POINT('Ctrl Pts',(-2.40790010365047,1.69295175539695,10.0803394257119));
#99807=CARTESIAN_POINT('Ctrl Pts',(-2.46042540772903,1.6156683494408,10.0853736389273));
#99808=CARTESIAN_POINT('Ctrl Pts',(-2.50916235127285,1.53605608457338,10.0904078521428));
#99809=CARTESIAN_POINT('Ctrl Pts',(-2.55789518088868,1.45645053984681,10.0954416404159));
#99810=CARTESIAN_POINT('Ctrl Pts',(-2.60284005393637,1.37451690608349,10.100475428689));
#99811=CARTESIAN_POINT('Ctrl Pts',(-2.64378055671563,1.29065424027213,10.1055092169621));
#99812=CARTESIAN_POINT('Ctrl Pts',(-2.68472905933543,1.20677518756004,10.1105439888456));
#99813=CARTESIAN_POINT('Ctrl Pts',(-2.72167144314922,1.12096675360975,10.1155787607291));
#99814=CARTESIAN_POINT('Ctrl Pts',(-2.75443855814882,1.0336499549572,10.1206135326126));
#99815=CARTESIAN_POINT('Ctrl Pts',(-2.78724169645872,0.94623716249711,10.1256538395928));
#99816=CARTESIAN_POINT('Ctrl Pts',(-2.81586024702623,0.857313111868039,
10.130694146573));
#99817=CARTESIAN_POINT('Ctrl Pts',(-2.84017438558591,0.767315749520159,
10.1357344535532));
#99818=CARTESIAN_POINT('Ctrl Pts',(-2.86450345455197,0.67726312314598,10.1407778555981));
#99819=CARTESIAN_POINT('Ctrl Pts',(-2.88452275420294,0.586136306590904,
10.145821257643));
#99820=CARTESIAN_POINT('Ctrl Pts',(-2.90016367653447,0.494383099741565,
10.1508646596878));
#99821=CARTESIAN_POINT('Ctrl Pts',(-2.91582996203316,0.40248110678653,10.1559162400643));
#99822=CARTESIAN_POINT('Ctrl Pts',(-2.92710364230719,0.309951136205699,
10.1609678204407));
#99823=CARTESIAN_POINT('Ctrl Pts',(-2.93396802256676,0.21724558121101,10.1660194008172));
#99824=CARTESIAN_POINT('Ctrl Pts',(-2.93747026836645,0.169946680463769,
10.1685967458194));
#99825=CARTESIAN_POINT('Ctrl Pts',(-2.93982557003811,0.122602070252842,
10.1711740908216));
#99826=CARTESIAN_POINT('Ctrl Pts',(-2.94103692609892,0.0752715040544825,
10.1737514358238));
#99827=CARTESIAN_POINT('Ctrl Pts',(-2.94167494486841,0.0503425912581443,
10.175108918186));
#99828=CARTESIAN_POINT('Ctrl Pts',(-2.94199601583779,0.0254055319659734,
10.1764664005482));
#99829=CARTESIAN_POINT('Ctrl Pts',(-2.94199996315092,0.000465639337999335,
10.1778238829104));
#99830=CARTESIAN_POINT('',(-2.94199900023815,0.00242540671930449,11.1778238494769));
#99831=CARTESIAN_POINT('Ctrl Pts',(-2.941999963151,0.000465638797186323,
10.1778238829398));
#99832=CARTESIAN_POINT('Ctrl Pts',(-2.94201459018696,-0.0919509285156992,
10.1828541315448));
#99833=CARTESIAN_POINT('Ctrl Pts',(-2.9376703396371,-0.184540249590128,
10.1878843801497));
#99834=CARTESIAN_POINT('Ctrl Pts',(-2.92894441554051,-0.276854854886246,
10.1929146287547));
#99835=CARTESIAN_POINT('Ctrl Pts',(-2.92023046815804,-0.369042754331495,
10.1979379731225));
#99836=CARTESIAN_POINT('Ctrl Pts',(-2.90714683721503,-0.460956244507401,
10.2029613174902));
#99837=CARTESIAN_POINT('Ctrl Pts',(-2.88972272958064,-0.552147214196571,
10.207984661858));
#99838=CARTESIAN_POINT('Ctrl Pts',(-2.87169574924409,-0.646493383994814,
10.213181813531));
#99839=CARTESIAN_POINT('Ctrl Pts',(-2.84902243369197,-0.740065636381678,
10.2183789652039));
#99840=CARTESIAN_POINT('Ctrl Pts',(-2.8217937359022,-0.832372580052397,
10.2235761168768));
#99841=CARTESIAN_POINT('Ctrl Pts',(-2.79552210425161,-0.921435011228237,
10.2285905929799));
#99842=CARTESIAN_POINT('Ctrl Pts',(-2.76501010197364,-1.00931912350969,
10.2336050690829));
#99843=CARTESIAN_POINT('Ctrl Pts',(-2.73039119609779,-1.09559477740251,
10.238619545186));
#99844=CARTESIAN_POINT('Ctrl Pts',(-2.69578363629902,-1.18184215512096,
10.2436323778335));
#99845=CARTESIAN_POINT('Ctrl Pts',(-2.65707201338557,-1.266481705588,10.248645210481));
#99846=CARTESIAN_POINT('Ctrl Pts',(-2.61443869955637,-1.34910128836273,
10.2536580431285));
#99847=CARTESIAN_POINT('Ctrl Pts',(-2.5718071616241,-1.43171742960666,10.2586706669657));
#99848=CARTESIAN_POINT('Ctrl Pts',(-2.52525446385776,-1.51231337209969,
10.263683290803));
#99849=CARTESIAN_POINT('Ctrl Pts',(-2.47500934673925,-1.59050078074592,
10.2686959146402));
#99850=CARTESIAN_POINT('Ctrl Pts',(-2.42475194795028,-1.66870730113954,
10.2737097637386));
#99851=CARTESIAN_POINT('Ctrl Pts',(-2.37080058059845,-1.74450374171304,
10.2787236128371));
#99852=CARTESIAN_POINT('Ctrl Pts',(-2.31342711202098,-1.8175310168925,10.2837374619356));
#99853=CARTESIAN_POINT('Ctrl Pts',(-2.25598943837909,-1.89064001487909,
10.2887569218941));
#99854=CARTESIAN_POINT('Ctrl Pts',(-2.19512230010199,-1.96097331145026,
10.2937763818527));
#99855=CARTESIAN_POINT('Ctrl Pts',(-2.1311373570192,-2.0282055037686,10.2987958418112));
#99856=CARTESIAN_POINT('Ctrl Pts',(-2.06710957764277,-2.09548270633143,
10.3038186621706));
#99857=CARTESIAN_POINT('Ctrl Pts',(-1.99996016392209,-2.15965436438974,
10.3088414825301));
#99858=CARTESIAN_POINT('Ctrl Pts',(-1.93003544668252,-2.22043400589817,
10.3138643028895));
#99859=CARTESIAN_POINT('Ctrl Pts',(-1.86000269536138,-2.28130755229472,
10.3188948835347));
#99860=CARTESIAN_POINT('Ctrl Pts',(-1.78718643750142,-2.33877835063966,
10.3239254641799));
#99861=CARTESIAN_POINT('Ctrl Pts',(-1.71196329883252,-2.39260227857672,
10.328956044825));
#99862=CARTESIAN_POINT('Ctrl Pts',(-1.69322070776798,-2.40601304404945,
10.3302094638862));
#99863=CARTESIAN_POINT('Ctrl Pts',(-1.67432881903902,-2.41919763059321,
10.3314628829474));
#99864=CARTESIAN_POINT('Ctrl Pts',(-1.65529369110195,-2.43215270823978,
10.3327163020086));
#99865=CARTESIAN_POINT('Ctrl Pts',(-1.57857025215669,-2.48436975201975,
10.3377683626583));
#99866=CARTESIAN_POINT('Ctrl Pts',(-1.49923571003575,-2.53304664572001,
10.342820423308));
#99867=CARTESIAN_POINT('Ctrl Pts',(-1.41765067150871,-2.57791205698932,
10.3478724839577));
#99868=CARTESIAN_POINT('Ctrl Pts',(-1.33617823010909,-2.622715548616,10.3529175721585));
#99869=CARTESIAN_POINT('Ctrl Pts',(-1.25246185014146,-2.66371779843324,
10.3579626603593));
#99870=CARTESIAN_POINT('Ctrl Pts',(-1.16689177935965,-2.70069020349667,
10.3630077485601));
#99871=CARTESIAN_POINT('Ctrl Pts',(-1.08141335900638,-2.73762300900458,
10.3680474331835));
#99872=CARTESIAN_POINT('Ctrl Pts',(-0.994085599788648,-2.77053437354037,
10.3730871178069));
#99873=CARTESIAN_POINT('Ctrl Pts',(-0.905323085611669,-2.79924170279356,
10.3781268024303));
#99874=CARTESIAN_POINT('Ctrl Pts',(-0.816624631421044,-2.82792831394139,
10.3831628499088));
#99875=CARTESIAN_POINT('Ctrl Pts',(-0.72649390191969,-2.85241678407349,
10.3881988973874));
#99876=CARTESIAN_POINT('Ctrl Pts',(-0.635364204627327,-2.87257311960519,
10.3932349448659));
#99877=CARTESIAN_POINT('Ctrl Pts',(-0.544267699205483,-2.89272211366095,
10.3982691580813));
#99878=CARTESIAN_POINT('Ctrl Pts',(-0.452173382196428,-2.90854201187061,
10.4033033712968));
#99879=CARTESIAN_POINT('Ctrl Pts',(-0.359527412653276,-2.91994932140112,
10.4083375845122));
#99880=CARTESIAN_POINT('Ctrl Pts',(-0.266889263437537,-2.93135566803063,
10.4133713727854));
#99881=CARTESIAN_POINT('Ctrl Pts',(-0.173699995264317,-2.93835011241512,
10.4184051610585));
#99882=CARTESIAN_POINT('Ctrl Pts',(-0.0804124548388498,-2.94090085468837,
10.4234389493316));
#99883=CARTESIAN_POINT('Ctrl Pts',(0.0128933141230999,-2.94345209538079,
10.4284737212151));
#99884=CARTESIAN_POINT('Ctrl Pts',(0.106296949352597,-2.94155789773219,
10.4335084930986));
#99885=CARTESIAN_POINT('Ctrl Pts',(0.19934518054053,-2.93523857616298,10.4385432649821));
#99886=CARTESIAN_POINT('Ctrl Pts',(0.292495706523349,-2.9289123072967,10.4435835719623));
#99887=CARTESIAN_POINT('Ctrl Pts',(0.385289604563623,-2.91815123377434,
10.4486238789425));
#99888=CARTESIAN_POINT('Ctrl Pts',(0.477278612801847,-2.90302757922861,
10.4536641859227));
#99889=CARTESIAN_POINT('Ctrl Pts',(0.569324108061952,-2.88789463781024,
10.4587075879675));
#99890=CARTESIAN_POINT('Ctrl Pts',(0.660563295389788,-2.86839387501129,
10.4637509900124));
#99891=CARTESIAN_POINT('Ctrl Pts',(0.750560145639077,-2.84464821511874,
10.4687943920573));
#99892=CARTESIAN_POINT('Ctrl Pts',(0.840702933903302,-2.82086404949562,
10.4738459724338));
#99893=CARTESIAN_POINT('Ctrl Pts',(0.929598940040217,-2.79282137816211,
10.4788975528102));
#99894=CARTESIAN_POINT('Ctrl Pts',(1.01682944435761,-2.76069228294053,10.4839491331867));
#99895=CARTESIAN_POINT('Ctrl Pts',(1.06133494315002,-2.7442998360577,10.4865264781889));
#99896=CARTESIAN_POINT('Ctrl Pts',(1.10540724602397,-2.72684441622875,10.4891038231911));
#99897=CARTESIAN_POINT('Ctrl Pts',(1.14899320136477,-2.70835348933952,10.4916811681934));
#99898=CARTESIAN_POINT('Ctrl Pts',(1.23442952815362,-2.67210794051572,10.4967332288431));
#99899=CARTESIAN_POINT('Ctrl Pts',(1.31830261598088,-2.63175060298992,10.5017852894928));
#99900=CARTESIAN_POINT('Ctrl Pts',(1.40018912286786,-2.58743780991979,10.5068373501426));
#99901=CARTESIAN_POINT('Ctrl Pts',(1.48196261656491,-2.54318617381301,10.5118824383433));
#99902=CARTESIAN_POINT('Ctrl Pts',(1.5617545900905,-2.49499013947571,10.5169275265441));
#99903=CARTESIAN_POINT('Ctrl Pts',(1.63916158455543,-2.44305409267125,10.5219726147449));
#99904=CARTESIAN_POINT('Ctrl Pts',(1.71648567171248,-2.39117367233636,10.5270122993683));
#99905=CARTESIAN_POINT('Ctrl Pts',(1.79142949017917,-2.33556144778772,10.5320519839918));
#99906=CARTESIAN_POINT('Ctrl Pts',(1.86361509295472,-2.27646717202585,10.5370916686152));
#99907=CARTESIAN_POINT('Ctrl Pts',(1.93574859931567,-2.21741554465607,10.5421277160937));
#99908=CARTESIAN_POINT('Ctrl Pts',(2.00512750378226,-2.15488714163099,10.5471637635722));
#99909=CARTESIAN_POINT('Ctrl Pts',(2.07140458884285,-2.08917376714355,10.5521998110507));
#99910=CARTESIAN_POINT('Ctrl Pts',(2.13765753401841,-2.0234843272227,10.5572340242662));
#99911=CARTESIAN_POINT('Ctrl Pts',(2.20081058898781,-1.95461253290325,10.5622682374816));
#99912=CARTESIAN_POINT('Ctrl Pts',(2.26055204191595,-1.88288833067435,10.5673024506971));
#99913=CARTESIAN_POINT('Ctrl Pts',(2.32028845201586,-1.81117018274801,10.5723362389702));
#99914=CARTESIAN_POINT('Ctrl Pts',(2.37661354841684,-1.73660044712834,10.5773700272433));
#99915=CARTESIAN_POINT('Ctrl Pts',(2.4292554639561,-1.65954267520887,10.5824038155165));
#99916=CARTESIAN_POINT('Ctrl Pts',(2.48190766581084,-1.58246984607609,10.5874385874));
#99917=CARTESIAN_POINT('Ctrl Pts',(2.53087500717596,-1.50290838217252,10.5924733592835));
#99918=CARTESIAN_POINT('Ctrl Pts',(2.57592921058967,-1.42125040089031,10.597508131167));
#99919=CARTESIAN_POINT('Ctrl Pts',(2.6210329454177,-1.33950264695657,10.6025484381472));
#99920=CARTESIAN_POINT('Ctrl Pts',(2.66221473998287,-1.25565416448217,10.6075887451274));
#99921=CARTESIAN_POINT('Ctrl Pts',(2.69929267450065,-1.17012095844282,10.6126290521076));
#99922=CARTESIAN_POINT('Ctrl Pts',(2.73639337719623,-1.0845352296492,10.6176724541524));
#99923=CARTESIAN_POINT('Ctrl Pts',(2.76938504597688,-0.997263133048711,
10.6227158561973));
#99924=CARTESIAN_POINT('Ctrl Pts',(2.79813501309297,-0.908737832657571,
10.6277592582422));
#99925=CARTESIAN_POINT('Ctrl Pts',(2.82693160087547,-0.820068980502306,
10.6328108386186));
#99926=CARTESIAN_POINT('Ctrl Pts',(2.85147263839126,-0.730143295627111,
10.6378624189951));
#99927=CARTESIAN_POINT('Ctrl Pts',(2.87167616050725,-0.639405997136669,
10.6429139993716));
#99928=CARTESIAN_POINT('Ctrl Pts',(2.88198411225141,-0.593111312038459,
10.6454913443738));
#99929=CARTESIAN_POINT('Ctrl Pts',(2.89116379772252,-0.546605474376901,
10.648068689376));
#99930=CARTESIAN_POINT('Ctrl Pts',(2.89920953959236,-0.499948042837104,
10.6506460343781));
#99931=CARTESIAN_POINT('Ctrl Pts',(2.91498064352448,-0.408491069207567,
10.6556980950279));
#99932=CARTESIAN_POINT('Ctrl Pts',(2.9264482602729,-0.316122766635949,10.6607501556776));
#99933=CARTESIAN_POINT('Ctrl Pts',(2.93351468075643,-0.223283715900937,
10.6658022163273));
#99934=CARTESIAN_POINT('Ctrl Pts',(2.94057134873308,-0.130572794178757,
10.6708473045281));
#99935=CARTESIAN_POINT('Ctrl Pts',(2.94323885714092,-0.0373928544717329,
10.6758923927288));
#99936=CARTESIAN_POINT('Ctrl Pts',(2.94147066358924,0.0558062294362782,
10.6809374809296));
#99937=CARTESIAN_POINT('Ctrl Pts',(2.93970436387373,0.148905491807847,10.685977165553));
#99938=CARTESIAN_POINT('Ctrl Pts',(2.93351181366009,0.242023415793992,10.6910168501765));
#99939=CARTESIAN_POINT('Ctrl Pts',(2.92289842623039,0.334707021049594,10.6960565347999));
#99940=CARTESIAN_POINT('Ctrl Pts',(2.91229269849198,0.427323736463604,10.7010925822784));
#99941=CARTESIAN_POINT('Ctrl Pts',(2.89727252553217,0.519506316022336,10.7061286297569));
#99942=CARTESIAN_POINT('Ctrl Pts',(2.87789531241531,0.610804854907006,10.7111646772354));
#99943=CARTESIAN_POINT('Ctrl Pts',(2.85852515699718,0.702070140424593,10.7161988904509));
#99944=CARTESIAN_POINT('Ctrl Pts',(2.83480120620408,0.792451590753148,10.7212331036663));
#99945=CARTESIAN_POINT('Ctrl Pts',(2.80683215556769,0.881508508450836,10.7262673168818));
#99946=CARTESIAN_POINT('Ctrl Pts',(2.7788654658233,0.970557908776306,10.7313011051549));
#99947=CARTESIAN_POINT('Ctrl Pts',(2.74665452197561,1.05828257492776,10.736334893428));
#99948=CARTESIAN_POINT('Ctrl Pts',(2.71035784359889,1.14425712129835,10.7413686817011));
#99949=CARTESIAN_POINT('Ctrl Pts',(2.67405407279247,1.23024846723444,10.7464034535846));
#99950=CARTESIAN_POINT('Ctrl Pts',(2.63366315505343,1.31448860507283,10.7514382254681));
#99951=CARTESIAN_POINT('Ctrl Pts',(2.58939122436995,1.39657333755012,10.7564729973516));
#99952=CARTESIAN_POINT('Ctrl Pts',(2.54507062228231,1.47874831183814,10.7615133043318));
#99953=CARTESIAN_POINT('Ctrl Pts',(2.49686070164771,1.55876275909157,10.766553611312));
#99954=CARTESIAN_POINT('Ctrl Pts',(2.44501277546394,1.63623853023272,10.7715939182922));
#99955=CARTESIAN_POINT('Ctrl Pts',(2.39313301140087,1.7137618763577,10.7766373203371));
#99956=CARTESIAN_POINT('Ctrl Pts',(2.33761105861865,1.78874308609211,10.781680722382));
#99957=CARTESIAN_POINT('Ctrl Pts',(2.27873931833247,1.86083613439918,10.7867241244268));
#99958=CARTESIAN_POINT('Ctrl Pts',(2.21977211220626,1.93304608809045,10.7917757048033));
#99959=CARTESIAN_POINT('Ctrl Pts',(2.15744457093765,2.00235820046636,10.7968272851797));
#99960=CARTESIAN_POINT('Ctrl Pts',(2.09208667763803,2.06846255302084,10.8018788655562));
#99961=CARTESIAN_POINT('Ctrl Pts',(2.05874070922855,2.1021893691822,10.8044562105584));
#99962=CARTESIAN_POINT('Ctrl Pts',(2.02460646014681,2.13508180906774,10.8070335555606));
#99963=CARTESIAN_POINT('Ctrl Pts',(1.98973093565381,2.16710285951134,10.8096109005629));
#99964=CARTESIAN_POINT('Ctrl Pts',(1.92136862297226,2.22986988867118,10.8146629612126));
#99965=CARTESIAN_POINT('Ctrl Pts',(1.8499105348167,2.28951174638045,10.8197150218623));
#99966=CARTESIAN_POINT('Ctrl Pts',(1.77567423197015,2.34570778698397,10.8247670825121));
#99967=CARTESIAN_POINT('Ctrl Pts',(1.70154038411552,2.4018262703188,10.8298121707128));
#99968=CARTESIAN_POINT('Ctrl Pts',(1.62463629189386,2.45450812074662,10.8348572589136));
#99969=CARTESIAN_POINT('Ctrl Pts',(1.54531502676182,2.50347068448267,10.8399023471144));
#99970=CARTESIAN_POINT('Ctrl Pts',(1.46607871923073,2.55238080651919,10.8449420317378));
#99971=CARTESIAN_POINT('Ctrl Pts',(1.38443076070111,2.59757932766267,10.8499817163612));
#99972=CARTESIAN_POINT('Ctrl Pts',(1.30075495866742,2.63882559815955,10.8550214009847));
#99973=CARTESIAN_POINT('Ctrl Pts',(1.21713954553546,2.68004210118585,10.8600574484632));
#99974=CARTESIAN_POINT('Ctrl Pts',(1.13149959516399,2.71731182710678,10.8650934959417));
#99975=CARTESIAN_POINT('Ctrl Pts',(1.04424447257713,2.75043950696832,10.8701295434202));
#99976=CARTESIAN_POINT('Ctrl Pts',(0.95702113063717,2.78355512084375,10.8751637566356));
#99977=CARTESIAN_POINT('Ctrl Pts',(0.868184200127716,2.81253152818451,10.8801979698511));
#99978=CARTESIAN_POINT('Ctrl Pts',(0.778163068161974,2.83722157036576,10.8852321830665));
#99979=CARTESIAN_POINT('Ctrl Pts',(0.688149534958645,2.86190952843897,10.8902659713397));
#99980=CARTESIAN_POINT('Ctrl Pts',(0.596952427566446,2.88231172337541,10.8952997596128));
#99981=CARTESIAN_POINT('Ctrl Pts',(0.505015228620273,2.89833117825786,10.9003335478859));
#99982=CARTESIAN_POINT('Ctrl Pts',(0.41306006499664,2.91435376336773,10.9053683197694));
#99983=CARTESIAN_POINT('Ctrl Pts',(0.320364960359397,2.92599183172582,10.9104030916529));
#99984=CARTESIAN_POINT('Ctrl Pts',(0.227381355662065,2.93319991120573,10.9154378635364));
#99985=CARTESIAN_POINT('Ctrl Pts',(0.134295527218521,2.94041591505993,10.9204781705166));
#99986=CARTESIAN_POINT('Ctrl Pts',(0.0409210092667924,2.94319217407971,
10.9255184774968));
#99987=CARTESIAN_POINT('Ctrl Pts',(-0.0522882034994405,2.94153530384641,
10.930558784477));
#99988=CARTESIAN_POINT('Ctrl Pts',(-0.145554652569598,2.93987741619085,
10.9356021865218));
#99989=CARTESIAN_POINT('Ctrl Pts',(-0.238655151344086,2.93378100889542,
10.9406455885667));
#99990=CARTESIAN_POINT('Ctrl Pts',(-0.33114047449463,2.92330463451065,10.9456889906116));
#99991=CARTESIAN_POINT('Ctrl Pts',(-0.423775770943575,2.91281127173932,
10.950740570988));
#99992=CARTESIAN_POINT('Ctrl Pts',(-0.515793462184951,2.89792383336941,
10.9557921513645));
#99993=CARTESIAN_POINT('Ctrl Pts',(-0.606754338829127,2.87875201646686,
10.960843731741));
#99994=CARTESIAN_POINT('Ctrl Pts',(-0.653163094772113,2.86897044658276,
10.9634210767432));
#99995=CARTESIAN_POINT('Ctrl Pts',(-0.699296987943584,2.85807441689912,
10.9659984217454));
#99996=CARTESIAN_POINT('Ctrl Pts',(-0.745099452472975,2.84608341513816,
10.9685757667476));
#99997=CARTESIAN_POINT('Ctrl Pts',(-0.83488053669317,2.8225788908719,10.9736278273974));
#99998=CARTESIAN_POINT('Ctrl Pts',(-0.923709662851784,2.79477968405277,
10.9786798880471));
#99999=CARTESIAN_POINT('Ctrl Pts',(-1.01114532619468,2.76277924006147,10.9837319486969));
#100000=CARTESIAN_POINT('Ctrl Pts',(-1.09846031784684,2.73082296051673,
10.9887770368976));
#100001=CARTESIAN_POINT('Ctrl Pts',(-1.18438525459698,2.69467711691828,
10.9938221250984));
#100002=CARTESIAN_POINT('Ctrl Pts',(-1.26849135403759,2.65448557817365,
10.9988672132992));
#100003=CARTESIAN_POINT('Ctrl Pts',(-1.35250737104688,2.6143370868602,11.0039068979226));
#100004=CARTESIAN_POINT('Ctrl Pts',(-1.4347080241103,2.57015170373841,11.0089465825461));
#100005=CARTESIAN_POINT('Ctrl Pts',(-1.51468321123573,2.52212187841917,
11.0139862671695));
#100006=CARTESIAN_POINT('Ctrl Pts',(-1.59460068019626,2.4741267162683,11.019022314648));
#100007=CARTESIAN_POINT('Ctrl Pts',(-1.67229549580595,2.42229285477578,
11.0240583621265));
#100008=CARTESIAN_POINT('Ctrl Pts',(-1.74738187892169,2.36685879790411,
11.029094409605));
#100009=CARTESIAN_POINT('Ctrl Pts',(-1.8224409135706,2.31144493159701,11.0341286228205));
#100010=CARTESIAN_POINT('Ctrl Pts',(-1.89489304603083,2.25243373853424,
11.0391628360359));
#100011=CARTESIAN_POINT('Ctrl Pts',(-1.96438211143745,2.19010660020569,
11.0441970492514));
#100012=CARTESIAN_POINT('Ctrl Pts',(-2.03386531121143,2.12778472296528,
11.0492308375245));
#100013=CARTESIAN_POINT('Ctrl Pts',(-2.10038561058346,2.06214775376033,
11.0542646257976));
#100014=CARTESIAN_POINT('Ctrl Pts',(-2.1636214087255,1.99351608965282,11.0592984140708));
#100015=CARTESIAN_POINT('Ctrl Pts',(-2.22686956324487,1.92487101480704,
11.0643331859543));
#100016=CARTESIAN_POINT('Ctrl Pts',(-2.28683164115361,1.85323040989809,
11.0693679578378));
#100017=CARTESIAN_POINT('Ctrl Pts',(-2.34322504025233,1.77894924343963,
11.0744027297213));
#100018=CARTESIAN_POINT('Ctrl Pts',(-2.39968043678087,1.70458641420722,
11.0794430367014));
#100019=CARTESIAN_POINT('Ctrl Pts',(-2.45255905399601,1.62757758316637,
11.0844833436816));
#100020=CARTESIAN_POINT('Ctrl Pts',(-2.50162070399376,1.54830806151417,
11.0895236506618));
#100021=CARTESIAN_POINT('Ctrl Pts',(-2.55071248092226,1.46898986340307,
11.0945670527067));
#100022=CARTESIAN_POINT('Ctrl Pts',(-2.59598240905828,1.38740859925202,
11.0996104547515));
#100023=CARTESIAN_POINT('Ctrl Pts',(-2.63723655209584,1.30397368389459,
11.1046538567964));
#100024=CARTESIAN_POINT('Ctrl Pts',(-2.67855759244963,1.2204034712917,11.1097054371728));
#100025=CARTESIAN_POINT('Ctrl Pts',(-2.71584966976585,1.13497401330425,
11.1147570175493));
#100026=CARTESIAN_POINT('Ctrl Pts',(-2.74896727302769,1.04811398799116,
11.1198085979258));
#100027=CARTESIAN_POINT('Ctrl Pts',(-2.76586406232745,1.00379750969158,
11.122385942928));
#100028=CARTESIAN_POINT('Ctrl Pts',(-2.78167500073675,0.959108878155302,
11.1249632879302));
#100029=CARTESIAN_POINT('Ctrl Pts',(-2.79638585452687,0.914106204224653,
11.1275406329324));
#100030=CARTESIAN_POINT('Ctrl Pts',(-2.83087452683876,0.808600263067428,
11.1335830563351));
#100031=CARTESIAN_POINT('Ctrl Pts',(-2.85941468770278,0.701059871883707,
11.1396254797378));
#100032=CARTESIAN_POINT('Ctrl Pts',(-2.88180167265537,0.592100599122085,
11.1456679031406));
#100033=CARTESIAN_POINT('Ctrl Pts',(-2.90393651237435,0.484368537677298,
11.1516422705606));
#100034=CARTESIAN_POINT('Ctrl Pts',(-2.9200559557708,0.375249434849865,
11.1576166379806));
#100035=CARTESIAN_POINT('Ctrl Pts',(-2.93000827999668,0.265359151247653,
11.1635910054007));
#100036=CARTESIAN_POINT('Ctrl Pts',(-2.93791148095195,0.178094611364554,
11.1683352867594));
#100037=CARTESIAN_POINT('Ctrl Pts',(-2.94192651932955,0.0903441705776652,
11.1730795681182));
#100038=CARTESIAN_POINT('Ctrl Pts',(-2.94199900023815,0.00242540671930449,
11.1778238494769));
#100039=CARTESIAN_POINT('',(-2.9380472957324,-0.00162286220386191,12.1778238829104));
#100040=CARTESIAN_POINT('Ctrl Pts',(-2.93966322424947,0.00242286200588204,
11.1778238829104));
#100041=CARTESIAN_POINT('Ctrl Pts',(-2.93447022488878,-0.668394196839997,
11.2140510883126));
#100042=CARTESIAN_POINT('Ctrl Pts',(-2.37356269205824,-2.3282443459899,
11.3032665824432));
#100043=CARTESIAN_POINT('Ctrl Pts',(0.384920002627215,-3.45738444354686,
11.4454703653018));
#100044=CARTESIAN_POINT('Ctrl Pts',(3.11541549378935,-1.54785558110535,
11.6044352314866));
#100045=CARTESIAN_POINT('Ctrl Pts',(2.98787167512539,1.78165469490725,11.7634000976714));
#100046=CARTESIAN_POINT('Ctrl Pts',(0.119295491036091,3.47669946712688,
11.922364963856));
#100047=CARTESIAN_POINT('Ctrl Pts',(-2.4686154660414,2.17803105228073,12.0605062256025));
#100048=CARTESIAN_POINT('Ctrl Pts',(-2.93506592488484,0.594792322390365,
12.1456591986206));
#100049=CARTESIAN_POINT('Ctrl Pts',(-2.9380472957324,-0.00162286220386191,
12.1778238829104));
#100050=CARTESIAN_POINT('',(-2.94199950407814,-0.00170821660887623,13.1778238829104));
#100051=CARTESIAN_POINT('Ctrl Pts',(-2.9380472957324,-0.00162286220386191,
12.1778238829104));
#100052=CARTESIAN_POINT('Ctrl Pts',(-2.93997745262914,-0.38774553554093,
12.1986474873488));
#100053=CARTESIAN_POINT('Ctrl Pts',(-2.68948523871683,-1.75400101947579,
12.2724593805155));
#100054=CARTESIAN_POINT('Ctrl Pts',(-0.62100113389732,-3.42286841561285,
12.3992595624103));
#100055=CARTESIAN_POINT('Ctrl Pts',(2.54188151956999,-2.37497556605756,
12.558224428595));
#100056=CARTESIAN_POINT('Ctrl Pts',(3.37287704005805,0.851687191139494,
12.7171892947799));
#100057=CARTESIAN_POINT('Ctrl Pts',(1.10964157051829,3.29702383732351,12.8761541609645));
#100058=CARTESIAN_POINT('Ctrl Pts',(-2.05967935882506,2.73746974758015,
13.0296985506708));
#100059=CARTESIAN_POINT('Ctrl Pts',(-2.93954203332316,0.874568473683911,
13.1302546516486));
#100060=CARTESIAN_POINT('Ctrl Pts',(-2.94560408402907,-0.00168416984504231,
13.1778224638982));
#100061=CARTESIAN_POINT('',(-2.94199888698872,0.00255909303077856,14.1778238829104));
#100062=CARTESIAN_POINT('Ctrl Pts',(-2.94199950407814,-0.00170821660887623,
13.1778238829104));
#100063=CARTESIAN_POINT('Ctrl Pts',(-2.9419416035759,-0.101428151412843,
13.183243886385));
#100064=CARTESIAN_POINT('Ctrl Pts',(-2.93681405116898,-0.200999029500833,
13.1886638898595));
#100065=CARTESIAN_POINT('Ctrl Pts',(-2.92665961476548,-0.300045828667542,
13.194083893334));
#100066=CARTESIAN_POINT('Ctrl Pts',(-2.91719452331025,-0.392368728256213,
13.1991359539837));
#100067=CARTESIAN_POINT('Ctrl Pts',(-2.90333958420986,-0.484409209656405,
13.2041880146334));
#100068=CARTESIAN_POINT('Ctrl Pts',(-2.88511946458446,-0.575716662148895,
13.2092400752831));
#100069=CARTESIAN_POINT('Ctrl Pts',(-2.86692449090703,-0.666898099417747,
13.2142851634838));
#100070=CARTESIAN_POINT('Ctrl Pts',(-2.84437639424497,-0.75734808616101,
13.2193302516846));
#100071=CARTESIAN_POINT('Ctrl Pts',(-2.81755161946311,-0.846620854728244,
13.2243753398853));
#100072=CARTESIAN_POINT('Ctrl Pts',(-2.79075557554563,-0.935798007066586,
13.2294150245088));
#100073=CARTESIAN_POINT('Ctrl Pts',(-2.75969208521324,-1.02380002416844,
13.2344547091322));
#100074=CARTESIAN_POINT('Ctrl Pts',(-2.72448846328387,-1.11019215158148,
13.2394943937556));
#100075=CARTESIAN_POINT('Ctrl Pts',(-2.68931024784018,-1.19652192971826,
13.2445304412341));
#100076=CARTESIAN_POINT('Ctrl Pts',(-2.64999800690478,-1.2812437172495,
13.2495664887126));
#100077=CARTESIAN_POINT('Ctrl Pts',(-2.60672829362551,-1.36393973591659,
13.2546025361911));
#100078=CARTESIAN_POINT('Ctrl Pts',(-2.56347434033188,-1.44660563448424,
13.2596367494066));
#100079=CARTESIAN_POINT('Ctrl Pts',(-2.51626598398431,-1.52724683670544,
13.2646709626221));
#100080=CARTESIAN_POINT('Ctrl Pts',(-2.46532668784965,-1.60546825635896,
13.2697051758376));
#100081=CARTESIAN_POINT('Ctrl Pts',(-2.41439169154547,-1.68368307327412,
13.2747389641107));
#100082=CARTESIAN_POINT('Ctrl Pts',(-2.35972662421619,-1.7594781415096,
13.2797727523838));
#100083=CARTESIAN_POINT('Ctrl Pts',(-2.30159880163073,-1.83248655010943,
13.284806540657));
#100084=CARTESIAN_POINT('Ctrl Pts',(-2.24345962077456,-1.9055092246706,
13.2898413125405));
#100085=CARTESIAN_POINT('Ctrl Pts',(-2.18185661789604,-1.97574381084583,
13.294876084424));
#100086=CARTESIAN_POINT('Ctrl Pts',(-2.11709724939872,-2.04285663632776,
13.2999108563076));
#100087=CARTESIAN_POINT('Ctrl Pts',(-2.0522666861434,-2.11004324389683,
13.3049511632878));
#100088=CARTESIAN_POINT('Ctrl Pts',(-1.98427313965147,-2.17410091987957,
13.309991470268));
#100089=CARTESIAN_POINT('Ctrl Pts',(-1.91346055171977,-2.23473325410714,
13.3150317772482));
#100090=CARTESIAN_POINT('Ctrl Pts',(-1.84260448041671,-2.29540282039165,
13.3200751792931));
#100091=CARTESIAN_POINT('Ctrl Pts',(-1.76892627206687,-2.35264258513913,
13.325118581338));
#100092=CARTESIAN_POINT('Ctrl Pts',(-1.69280077672489,-2.40619814859866,
13.3301619833829));
#100093=CARTESIAN_POINT('Ctrl Pts',(-1.61655183702189,-2.45984055723772,
13.3352135637594));
#100094=CARTESIAN_POINT('Ctrl Pts',(-1.53784806233757,-2.50978659985422,
13.3402651441359));
#100095=CARTESIAN_POINT('Ctrl Pts',(-1.45709076095764,-2.55582677705902,
13.3453167245123));
#100096=CARTESIAN_POINT('Ctrl Pts',(-1.41588792707355,-2.57931673698771,
13.3478940695146));
#100097=CARTESIAN_POINT('Ctrl Pts',(-1.3741508982027,-2.60179072157022,
13.3504714145168));
#100098=CARTESIAN_POINT('Ctrl Pts',(-1.3319349167263,-2.62322575803252,
13.353048759519));
#100099=CARTESIAN_POINT('Ctrl Pts',(-1.24918398558434,-2.66524229215738,
13.3581008201687));
#100100=CARTESIAN_POINT('Ctrl Pts',(-1.16429426401653,-2.70341485725333,
13.3631528808185));
#100101=CARTESIAN_POINT('Ctrl Pts',(-1.07765798931138,-2.7375202753721,
13.3682049414682));
#100102=CARTESIAN_POINT('Ctrl Pts',(-0.991141283044934,-2.77157862392781,
13.373250029669));
#100103=CARTESIAN_POINT('Ctrl Pts',(-0.902883223327401,-2.80158081817814,
13.3782951178697));
#100104=CARTESIAN_POINT('Ctrl Pts',(-0.813300002922856,-2.82734983778903,
13.3833402060705));
#100105=CARTESIAN_POINT('Ctrl Pts',(-0.723812731258834,-2.85309125730959,
13.3883798906939));
#100106=CARTESIAN_POINT('Ctrl Pts',(-0.633003544705303,-2.87460839194949,
13.3934195753174));
#100107=CARTESIAN_POINT('Ctrl Pts',(-0.541306912108402,-2.89177295562838,
13.3984592599408));
#100108=CARTESIAN_POINT('Ctrl Pts',(-0.449676457053898,-2.90892513162618,
13.4034953074193));
#100109=CARTESIAN_POINT('Ctrl Pts',(-0.35716026443591,-2.92173089881644,
13.4085313548978));
#100110=CARTESIAN_POINT('Ctrl Pts',(-0.26420518213739,-2.93011256127333,
13.4135674023763));
#100111=CARTESIAN_POINT('Ctrl Pts',(-0.171283956563379,-2.93849117090481,
13.4186016155917));
#100112=CARTESIAN_POINT('Ctrl Pts',(-0.0779246009367638,-2.94244883710017,
13.4236358288072));
#100113=CARTESIAN_POINT('Ctrl Pts',(0.0154197241241465,-2.94195959049541,
13.4286700420226));
#100114=CARTESIAN_POINT('Ctrl Pts',(0.108756169909025,-2.94147038518838,
13.4337038302957));
#100115=CARTESIAN_POINT('Ctrl Pts',(0.202077143355244,-2.93653501590194,
13.4387376185689));
#100116=CARTESIAN_POINT('Ctrl Pts',(0.294929436653915,-2.92717963702179,
13.443771406842));
#100117=CARTESIAN_POINT('Ctrl Pts',(0.387799873441089,-2.91782243008545,
13.4488061787255));
#100118=CARTESIAN_POINT('Ctrl Pts',(0.480201006199476,-2.90404354319927,
13.4538409506089));
#100119=CARTESIAN_POINT('Ctrl Pts',(0.571685846608818,-2.88592087431155,
13.4588757224924));
#100120=CARTESIAN_POINT('Ctrl Pts',(0.663271263061884,-2.86777828183508,
13.4639160294726));
#100121=CARTESIAN_POINT('Ctrl Pts',(0.753937939861054,-2.84528246144413,
13.4689563364528));
#100122=CARTESIAN_POINT('Ctrl Pts',(0.843250469833347,-2.81856215917369,
13.473996643433));
#100123=CARTESIAN_POINT('Ctrl Pts',(0.932617843301892,-2.79182544896141,
13.4790400454778));
#100124=CARTESIAN_POINT('Ctrl Pts',(1.02062899572037,-2.76085923989495,
13.4840834475227));
#100125=CARTESIAN_POINT('Ctrl Pts',(1.10686711247742,-2.72584100697673,
13.4891268495676));
#100126=CARTESIAN_POINT('Ctrl Pts',(1.19324507212386,-2.69076598883339,
13.494178429944));
#100127=CARTESIAN_POINT('Ctrl Pts',(1.27784385347303,-2.65162601544494,
13.4992300103205));
#100128=CARTESIAN_POINT('Ctrl Pts',(1.36027007324264,-2.6086451134335,13.5042815906969));
#100129=CARTESIAN_POINT('Ctrl Pts',(1.4023243987688,-2.58671601308594,13.5068589356991));
#100130=CARTESIAN_POINT('Ctrl Pts',(1.443813630136,-2.56378779373677,13.5094362807013));
#100131=CARTESIAN_POINT('Ctrl Pts',(1.48468854817802,-2.53989446924652,
13.5120136257035));
#100132=CARTESIAN_POINT('Ctrl Pts',(1.56481075332511,-2.49305924759577,
13.5170656863532));
#100133=CARTESIAN_POINT('Ctrl Pts',(1.64285859476912,-2.44234491037467,
13.5221177470029));
#100134=CARTESIAN_POINT('Ctrl Pts',(1.71843209814497,-2.38796045278499,
13.5271698076527));
#100135=CARTESIAN_POINT('Ctrl Pts',(1.79390130103201,-2.33365105226236,
13.5322148958534));
#100136=CARTESIAN_POINT('Ctrl Pts',(1.86690259413939,-2.27568185380676,
13.5372599840542));
#100137=CARTESIAN_POINT('Ctrl Pts',(1.93706184631927,-2.21430698041942,
13.5423050722549));
#100138=CARTESIAN_POINT('Ctrl Pts',(2.00714595393684,-2.15299784302348,
13.5473447568784));
#100139=CARTESIAN_POINT('Ctrl Pts',(2.07439373838678,-2.0882905719314,13.5523844415018));
#100140=CARTESIAN_POINT('Ctrl Pts',(2.13846215253643,-2.02048103731989,
13.5574241261253));
#100141=CARTESIAN_POINT('Ctrl Pts',(2.20248432845386,-1.9527204409106,13.5624601736038));
#100142=CARTESIAN_POINT('Ctrl Pts',(2.26333139055242,-1.88186235313072,
13.5674962210823));
#100143=CARTESIAN_POINT('Ctrl Pts',(2.32069612831383,-1.80824043756056,
13.5725322685608));
#100144=CARTESIAN_POINT('Ctrl Pts',(2.3780399723051,-1.73464533705904,13.5775664817762));
#100145=CARTESIAN_POINT('Ctrl Pts',(2.4319037388655,-1.65828875871343,13.5826006949917));
#100146=CARTESIAN_POINT('Ctrl Pts',(2.48202029334157,-1.5795376739542,13.5876349082072));
#100147=CARTESIAN_POINT('Ctrl Pts',(2.5321326174355,-1.50079323664281,13.5926686964803));
#100148=CARTESIAN_POINT('Ctrl Pts',(2.57849811993762,-1.4196550697134,13.5977024847534));
#100149=CARTESIAN_POINT('Ctrl Pts',(2.62089346760739,-1.33651839921975,
13.6027362730265));
#100150=CARTESIAN_POINT('Ctrl Pts',(2.66329709939676,-1.25336548368603,
13.6077710449101));
#100151=CARTESIAN_POINT('Ctrl Pts',(2.70172883416518,-1.16821368498781,
13.6128058167936));
#100152=CARTESIAN_POINT('Ctrl Pts',(2.73601221261071,-1.0814810088231,13.6178405886771));
#100153=CARTESIAN_POINT('Ctrl Pts',(2.77033328130693,-0.994652981019935,
13.6228808956573));
#100154=CARTESIAN_POINT('Ctrl Pts',(2.80049672657653,-0.906241020367979,
13.6279212026375));
#100155=CARTESIAN_POINT('Ctrl Pts',(2.82637511242025,-0.816680919264938,
13.6329615096177));
#100156=CARTESIAN_POINT('Ctrl Pts',(2.85226938921632,-0.727065822641398,
13.6380049116626));
#100157=CARTESIAN_POINT('Ctrl Pts',(2.87387326539693,-0.636301613902794,
13.6430483137074));
#100158=CARTESIAN_POINT('Ctrl Pts',(2.89111034178361,-0.544834829679486,
13.6480917157523));
#100159=CARTESIAN_POINT('Ctrl Pts',(2.9083753696453,-0.453219723810628,
13.6531432961288));
#100160=CARTESIAN_POINT('Ctrl Pts',(2.92125939962182,-0.360900207487329,
13.6581948765052));
#100161=CARTESIAN_POINT('Ctrl Pts',(2.92973785784498,-0.268328314402158,
13.6632464568817));
#100162=CARTESIAN_POINT('Ctrl Pts',(2.93406361539006,-0.221097608720155,
13.6658238018839));
#100163=CARTESIAN_POINT('Ctrl Pts',(2.93724339923687,-0.173801218406553,
13.6684011468862));
#100164=CARTESIAN_POINT('Ctrl Pts',(2.93927916642012,-0.126498940108793,
13.6709784918884));
#100165=CARTESIAN_POINT('Ctrl Pts',(2.94326963695069,-0.0337779506314332,
13.6760305525381));
#100166=CARTESIAN_POINT('Ctrl Pts',(2.94287558236983,0.0592986537052232,
13.6810826131878));
#100167=CARTESIAN_POINT('Ctrl Pts',(2.93805622221528,0.152281433871947,
13.6861346738376));
#100168=CARTESIAN_POINT('Ctrl Pts',(2.93324351335512,0.245135886662127,
13.6911797620383));
#100169=CARTESIAN_POINT('Ctrl Pts',(2.92401765796111,0.337896332743346,
13.6962248502391));
#100170=CARTESIAN_POINT('Ctrl Pts',(2.91038980926908,0.430110634724023,
13.7012699384399));
#100171=CARTESIAN_POINT('Ctrl Pts',(2.89677655678059,0.522226169925629,
13.7063096230633));
#100172=CARTESIAN_POINT('Ctrl Pts',(2.87877074691709,0.61379628654003,13.7113493076867));
#100173=CARTESIAN_POINT('Ctrl Pts',(2.856435460979,0.704372385362796,13.7163889923102));
#100174=CARTESIAN_POINT('Ctrl Pts',(2.83411629443691,0.794883115333414,
13.7214250397887));
#100175=CARTESIAN_POINT('Ctrl Pts',(2.80747396842548,0.88440082327186,13.7264610872672));
#100176=CARTESIAN_POINT('Ctrl Pts',(2.77662274049373,0.972486584469465,
13.7314971347457));
#100177=CARTESIAN_POINT('Ctrl Pts',(2.74578274940346,1.06054026247942,13.7365313479611));
#100178=CARTESIAN_POINT('Ctrl Pts',(2.71073704855245,1.14716261096171,13.7415655611766));
#100179=CARTESIAN_POINT('Ctrl Pts',(2.67164959490775,1.23193037223264,13.746599774392));
#100180=CARTESIAN_POINT('Ctrl Pts',(2.63256544066916,1.3166909781828,13.7516335626651));
#100181=CARTESIAN_POINT('Ctrl Pts',(2.5894403981624,1.39959690477271,13.7566673509383));
#100182=CARTESIAN_POINT('Ctrl Pts',(2.54248589155738,1.48024642922444,13.7617011392114));
#100183=CARTESIAN_POINT('Ctrl Pts',(2.49552220996571,1.56091171272386,13.7667359110949));
#100184=CARTESIAN_POINT('Ctrl Pts',(2.44472780203968,1.63931933468942,13.7717706829784));
#100185=CARTESIAN_POINT('Ctrl Pts',(2.3903586188314,1.71509465434956,13.7768054548619));
#100186=CARTESIAN_POINT('Ctrl Pts',(2.33592966356338,1.79095327941667,13.7818457618421));
#100187=CARTESIAN_POINT('Ctrl Pts',(2.27791834762396,1.86417346406433,13.7868860688222));
#100188=CARTESIAN_POINT('Ctrl Pts',(2.21662211421995,1.93441215948181,13.7919263758024));
#100189=CARTESIAN_POINT('Ctrl Pts',(2.15528824108331,2.00469398586459,13.7969697778473));
#100190=CARTESIAN_POINT('Ctrl Pts',(2.09066574225995,2.0719903579793,13.8020131798922));
#100191=CARTESIAN_POINT('Ctrl Pts',(2.02308872155946,2.13599532412852,13.807056581937));
#100192=CARTESIAN_POINT('Ctrl Pts',(1.95540211862103,2.20010408010686,13.8121081623135));
#100193=CARTESIAN_POINT('Ctrl Pts',(1.88475176539237,2.26091048528984,13.8171597426899));
#100194=CARTESIAN_POINT('Ctrl Pts',(1.81150444114801,2.31814918840463,13.8222113230664));
#100195=CARTESIAN_POINT('Ctrl Pts',(1.77413324025682,2.34735269986285,13.8247886680686));
#100196=CARTESIAN_POINT('Ctrl Pts',(1.73608648663172,2.37562820340534,13.8273660130708));
#100197=CARTESIAN_POINT('Ctrl Pts',(1.69741551815161,2.40294497621941,13.829943358073));
#100198=CARTESIAN_POINT('Ctrl Pts',(1.62161345130467,2.45649077350038,13.8349954187228));
#100199=CARTESIAN_POINT('Ctrl Pts',(1.54313900094964,2.50654244875047,13.8400474793725));
#100200=CARTESIAN_POINT('Ctrl Pts',(1.4623479919621,2.5528224282947,13.8450995400222));
#100201=CARTESIAN_POINT('Ctrl Pts',(1.38166848424622,2.59903853592253,13.850144628223));
#100202=CARTESIAN_POINT('Ctrl Pts',(1.29867915315312,2.64149307266085,13.8551897164238));
#100203=CARTESIAN_POINT('Ctrl Pts',(1.21376620447723,2.67995067134993,13.8602348046245));
#100204=CARTESIAN_POINT('Ctrl Pts',(1.12894420241449,2.71836707975643,13.865274489248));
#100205=CARTESIAN_POINT('Ctrl Pts',(1.04220308046915,2.75279487680003,13.8703141738714));
#100206=CARTESIAN_POINT('Ctrl Pts',(0.953954178457664,2.78304427298654,
13.8753538584948));
#100207=CARTESIAN_POINT('Ctrl Pts',(0.865768965758247,2.81327183815657,
13.8803899059733));
#100208=CARTESIAN_POINT('Ctrl Pts',(0.776078554954986,2.83932685264125,
13.8854259534518));
#100209=CARTESIAN_POINT('Ctrl Pts',(0.68531385336078,2.86106779409223,13.8904620009303));
#100210=CARTESIAN_POINT('Ctrl Pts',(0.594582210695881,2.88280081691149,
13.8954962141458));
#100211=CARTESIAN_POINT('Ctrl Pts',(0.502777486209641,2.90022278484671,
13.9005304273613));
#100212=CARTESIAN_POINT('Ctrl Pts',(0.410344316623877,2.91324244473653,
13.9055646405767));
#100213=CARTESIAN_POINT('Ctrl Pts',(0.317918949402688,2.92626100562549,
13.9105984288499));
#100214=CARTESIAN_POINT('Ctrl Pts',(0.224865682536686,2.93487793550296,
13.915632217123));
#100215=CARTESIAN_POINT('Ctrl Pts',(0.131636739981672,2.93905354981616,
13.9206660053961));
#100216=CARTESIAN_POINT('Ctrl Pts',(0.0383895803403089,2.94322998005117,
13.9257007772796));
#100217=CARTESIAN_POINT('Ctrl Pts',(-0.0550328793156447,2.94296335168255,
13.9307355491631));
#100218=CARTESIAN_POINT('Ctrl Pts',(-0.148177083553659,2.93826607915443,
13.9357703210467));
#100219=CARTESIAN_POINT('Ctrl Pts',(-0.241423688096629,2.9335636425676,
13.9408106280268));
#100220=CARTESIAN_POINT('Ctrl Pts',(-0.334390982164589,2.92442086123227,
13.945850935007));
#100221=CARTESIAN_POINT('Ctrl Pts',(-0.426629513650132,2.91090213818374,
13.9508912419872));
#100222=CARTESIAN_POINT('Ctrl Pts',(-0.518924685380454,2.89737511379118,
13.9559346440321));
#100223=CARTESIAN_POINT('Ctrl Pts',(-0.610489767911087,2.87946688341686,
13.960978046077));
#100224=CARTESIAN_POINT('Ctrl Pts',(-0.700886656682442,2.85729275617402,
13.9660214481219));
#100225=CARTESIAN_POINT('Ctrl Pts',(-0.791430132167314,2.83508267158262,
13.9710730284983));
#100226=CARTESIAN_POINT('Ctrl Pts',(-0.880801206608649,2.80859300612958,
13.9761246088748));
#100227=CARTESIAN_POINT('Ctrl Pts',(-0.968578225849275,2.77798852056856,
13.9811761892513));
#100228=CARTESIAN_POINT('Ctrl Pts',(-1.01336255965936,2.76237393819486,
13.9837535342535));
#100229=CARTESIAN_POINT('Ctrl Pts',(-1.05773228245566,2.74568899705179,
13.9863308792557));
#100230=CARTESIAN_POINT('Ctrl Pts',(-1.10163377217885,2.72796023284706,
13.9889082242579));
#100231=CARTESIAN_POINT('Ctrl Pts',(-1.18768860321842,2.6932086602285,13.9939602849076));
#100232=CARTESIAN_POINT('Ctrl Pts',(-1.27225206830103,2.65431868816531,
13.9990123455573));
#100233=CARTESIAN_POINT('Ctrl Pts',(-1.35489816605842,2.61143925060713,
14.004064406207));
#100234=CARTESIAN_POINT('Ctrl Pts',(-1.43743020229941,2.56861899181,14.0091094944078));
#100235=CARTESIAN_POINT('Ctrl Pts',(-1.51804973857495,2.5218204113224,14.0141545826086));
#100236=CARTESIAN_POINT('Ctrl Pts',(-1.59634981641415,2.47124083481042,
14.0191996708093));
#100237=CARTESIAN_POINT('Ctrl Pts',(-1.67456603040223,2.42071543191092,
14.0242393554328));
#100238=CARTESIAN_POINT('Ctrl Pts',(-1.75046735260485,2.36641732205891,
14.0292790400562));
#100239=CARTESIAN_POINT('Ctrl Pts',(-1.82367154217766,2.30858963574113,
14.0343187246796));
#100240=CARTESIAN_POINT('Ctrl Pts',(-1.89682290022091,2.25080368371666,
14.0393547721581));
#100241=CARTESIAN_POINT('Ctrl Pts',(-1.96728064697167,2.18949349294338,
14.0443908196366));
#100242=CARTESIAN_POINT('Ctrl Pts',(-2.03469253379327,2.12494477408848,
14.0494268671151));
#100243=CARTESIAN_POINT('Ctrl Pts',(-2.10207986740462,2.06041956560156,
14.0544610803306));
#100244=CARTESIAN_POINT('Ctrl Pts',(-2.16642322439926,1.99265847931019,
14.059495293546));
#100245=CARTESIAN_POINT('Ctrl Pts',(-2.22740519191158,1.92198598097003,
14.0645295067615));
#100246=CARTESIAN_POINT('Ctrl Pts',(-2.28838201188272,1.85131944815723,
14.0695632950346));
#100247=CARTESIAN_POINT('Ctrl Pts',(-2.34599771638028,1.77774232841077,
14.0745970833077));
#100248=CARTESIAN_POINT('Ctrl Pts',(-2.39997414569756,1.70161338146573,
14.0796308715808));
#100249=CARTESIAN_POINT('Ctrl Pts',(-2.45396112209656,1.62546955880117,
14.0846656434643));
#100250=CARTESIAN_POINT('Ctrl Pts',(-2.50430715436889,1.54677328129533,
14.0897004153478));
#100251=CARTESIAN_POINT('Ctrl Pts',(-2.55077716821508,1.46591262976777,
14.0947351872313));
#100252=CARTESIAN_POINT('Ctrl Pts',(-2.59729826998059,1.38496308215219,
14.0997754942115));
#100253=CARTESIAN_POINT('Ctrl Pts',(-2.6399346257115,1.30184479663781,14.1048158011917));
#100254=CARTESIAN_POINT('Ctrl Pts',(-2.67849709557925,1.21697054564747,
14.1098561081719));
#100255=CARTESIAN_POINT('Ctrl Pts',(-2.71708324522266,1.13204417654257,
14.1148995102168));
#100256=CARTESIAN_POINT('Ctrl Pts',(-2.75159036456666,1.04536010783004,
14.1199429122616));
#100257=CARTESIAN_POINT('Ctrl Pts',(-2.78187825939687,0.957349126439784,
14.1249863143065));
#100258=CARTESIAN_POINT('Ctrl Pts',(-2.81221526878206,0.869195427300135,
14.130037894683));
#100259=CARTESIAN_POINT('Ctrl Pts',(-2.83831927037654,0.779710945833389,
14.1350894750594));
#100260=CARTESIAN_POINT('Ctrl Pts',(-2.86010055486284,0.689339405571228,
14.1401410554359));
#100261=CARTESIAN_POINT('Ctrl Pts',(-2.87121348993049,0.643231332398185,
14.1427184004381));
#100262=CARTESIAN_POINT('Ctrl Pts',(-2.88120200867619,0.596892482010356,
14.1452957454403));
#100263=CARTESIAN_POINT('Ctrl Pts',(-2.89005939699962,0.550382305142697,
14.1478730904426));
#100264=CARTESIAN_POINT('Ctrl Pts',(-2.91574538419712,0.415505097104356,
14.155347263225));
#100265=CARTESIAN_POINT('Ctrl Pts',(-2.93199546254514,0.278777808809255,
14.1628214360074));
#100266=CARTESIAN_POINT('Ctrl Pts',(-2.93860597986145,0.141275953801512,
14.1702956087899));
#100267=CARTESIAN_POINT('Ctrl Pts',(-2.940825435574,0.0951102359037864,
14.1728050334967));
#100268=CARTESIAN_POINT('Ctrl Pts',(-2.94195861445419,0.0488574301164584,
14.1753144582036));
#100269=CARTESIAN_POINT('Ctrl Pts',(-2.94199888698872,0.00255909303077856,
14.1778238829104));
#100270=CARTESIAN_POINT('',(-2.94153552810316,0.000339057197988907,15.1778238581128));
#100271=CARTESIAN_POINT('Ctrl Pts',(-2.94332536232247,0.00254738520742678,
14.1778245797126));
#100272=CARTESIAN_POINT('Ctrl Pts',(-2.93605737211391,-0.791240222849468,
14.2208290386842));
#100273=CARTESIAN_POINT('Ctrl Pts',(-2.19483961771011,-2.57505010203599,
14.3168217863839));
#100274=CARTESIAN_POINT('Ctrl Pts',(0.822272561487176,-3.38016840313126,
14.4658028228121));
#100275=CARTESIAN_POINT('Ctrl Pts',(3.28723225708272,-1.1383209946658,14.6247676889968));
#100276=CARTESIAN_POINT('Ctrl Pts',(2.73653030818804,2.14780643244915,14.7837325551815));
#100277=CARTESIAN_POINT('Ctrl Pts',(-0.32462689424278,3.46356578953478,
14.9426974213664));
#100278=CARTESIAN_POINT('Ctrl Pts',(-2.60817372378361,1.92514024732049,
15.0740611115662));
#100279=CARTESIAN_POINT('Ctrl Pts',(-2.93766532742435,0.471430358787691,
15.152436513038));
#100280=CARTESIAN_POINT('Ctrl Pts',(-2.93718401591717,0.000342867480166743,
15.1778236257814));
#100281=CARTESIAN_POINT('',(-2.94199875963773,-0.00270153476367689,16.1778238829104));
#100282=CARTESIAN_POINT('Ctrl Pts',(-2.94199998050915,0.000338650512990829,
15.1778238829104));
#100283=CARTESIAN_POINT('Ctrl Pts',(-2.94201116901371,-0.0968606122596855,
15.1830534200964));
#100284=CARTESIAN_POINT('Ctrl Pts',(-2.93720105751752,-0.193984951321332,
15.1882829572824));
#100285=CARTESIAN_POINT('Ctrl Pts',(-2.92761780337622,-0.290547754000271,
15.1935124944683));
#100286=CARTESIAN_POINT('Ctrl Pts',(-2.91802323889267,-0.387224521970202,
15.1987482036554));
#100287=CARTESIAN_POINT('Ctrl Pts',(-2.903644344505,-0.48333804304514,15.2039839128426));
#100288=CARTESIAN_POINT('Ctrl Pts',(-2.88458066522055,-0.578410222796756,
15.2092196220297));
#100289=CARTESIAN_POINT('Ctrl Pts',(-2.8654748648745,-0.673692463842373,
15.2144668994784));
#100290=CARTESIAN_POINT('Ctrl Pts',(-2.84166367815638,-0.767928381784394,
15.2197141769271));
#100291=CARTESIAN_POINT('Ctrl Pts',(-2.81329716202206,-0.860652704729742,
15.2249614543758));
#100292=CARTESIAN_POINT('Ctrl Pts',(-2.78489523094661,-0.953492791853635,
15.2302152829294));
#100293=CARTESIAN_POINT('Ctrl Pts',(-2.75192676404131,-1.04481715309615,
15.235469111483));
#100294=CARTESIAN_POINT('Ctrl Pts',(-2.71459004383728,-1.13418027398625,
15.2407229400366));
#100295=CARTESIAN_POINT('Ctrl Pts',(-2.67717267079504,-1.2237364324354,
15.245988117637));
#100296=CARTESIAN_POINT('Ctrl Pts',(-2.63536836176582,-1.31132253321761,
15.2512532952374));
#100297=CARTESIAN_POINT('Ctrl Pts',(-2.58942164066141,-1.39651694113404,
15.2565184728377));
#100298=CARTESIAN_POINT('Ctrl Pts',(-2.57747013401016,-1.41867742415413,
15.2578880331371));
#100299=CARTESIAN_POINT('Ctrl Pts',(-2.56523857520824,-1.44067623877505,
15.2592575934365));
#100300=CARTESIAN_POINT('Ctrl Pts',(-2.55273173589492,-1.46250630239836,
15.2606271537359));
#100301=CARTESIAN_POINT('Ctrl Pts',(-2.50659626396544,-1.54303346535945,
15.2656792143856));
#100302=CARTESIAN_POINT('Ctrl Pts',(-2.45656375314834,-1.62152013566208,
15.2707312750353));
#100303=CARTESIAN_POINT('Ctrl Pts',(-2.40283970639844,-1.69756453348762,
15.2757833356851));
#100304=CARTESIAN_POINT('Ctrl Pts',(-2.34918980526959,-1.77350398093349,
15.2808284238858));
#100305=CARTESIAN_POINT('Ctrl Pts',(-2.29185874625095,-1.84700749402453,
15.2858735120866));
#100306=CARTESIAN_POINT('Ctrl Pts',(-2.23109738351376,-1.91769874205467,
15.2909186002873));
#100307=CARTESIAN_POINT('Ctrl Pts',(-2.17040109966286,-1.98831427572481,
15.2959582849108));
#100308=CARTESIAN_POINT('Ctrl Pts',(-2.10628210285226,-2.05612319618261,
15.3009979695342));
#100309=CARTESIAN_POINT('Ctrl Pts',(-2.03903326362832,-2.12077989188347,
15.3060376541577));
#100310=CARTESIAN_POINT('Ctrl Pts',(-1.97183295795236,-2.18538992478866,
15.3110737016362));
#100311=CARTESIAN_POINT('Ctrl Pts',(-1.90150761891054,-2.24685194768499,
15.3161097491147));
#100312=CARTESIAN_POINT('Ctrl Pts',(-1.82838822120408,-2.30485585505085,
15.3211457965932));
#100313=CARTESIAN_POINT('Ctrl Pts',(-1.75529545553588,-2.36283863584389,
15.3261800098086));
#100314=CARTESIAN_POINT('Ctrl Pts',(-1.67941100063365,-2.41736552745628,
15.3312142230241));
#100315=CARTESIAN_POINT('Ctrl Pts',(-1.60109948689982,-2.46816620855427,
15.3362484362395));
#100316=CARTESIAN_POINT('Ctrl Pts',(-1.52279458350912,-2.51896260152248,
15.3412822245127));
#100317=CARTESIAN_POINT('Ctrl Pts',(-1.44206340145464,-2.56603316768702,
15.3463160127858));
#100318=CARTESIAN_POINT('Ctrl Pts',(-1.35929920625946,-2.60915113932911,
15.3513498010589));
#100319=CARTESIAN_POINT('Ctrl Pts',(-1.27651883880636,-2.65227753629276,
15.3563845729424));
#100320=CARTESIAN_POINT('Ctrl Pts',(-1.19170506344987,-2.69144959991829,
15.3614193448259));
#100321=CARTESIAN_POINT('Ctrl Pts',(-1.10527433282822,-2.72648723620543,
15.3664541167094));
#100322=CARTESIAN_POINT('Ctrl Pts',(-1.01874858251935,-2.76156339195454,
15.3714944236896));
#100323=CARTESIAN_POINT('Ctrl Pts',(-0.930602740949971,-2.79249588022971,
15.3765347306698));
#100324=CARTESIAN_POINT('Ctrl Pts',(-0.841271473842247,-2.81915347352699,
15.38157503765));
#100325=CARTESIAN_POINT('Ctrl Pts',(-0.751885351732374,-2.84582743625891,
15.3866184396949));
#100326=CARTESIAN_POINT('Ctrl Pts',(-0.661312785928075,-2.86822117149054,
15.3916618417397));
#100327=CARTESIAN_POINT('Ctrl Pts',(-0.56999963057609,-2.88625439300543,
15.3967052437846));
#100328=CARTESIAN_POINT('Ctrl Pts',(-0.478538402701799,-2.90431685701647,
15.4017568241611));
#100329=CARTESIAN_POINT('Ctrl Pts',(-0.38633462669517,-2.91800462574334,
15.4068084045375));
#100330=CARTESIAN_POINT('Ctrl Pts',(-0.293840105025006,-2.92728918842654,
15.411859984914));
#100331=CARTESIAN_POINT('Ctrl Pts',(-0.24664887467922,-2.93202622504591,
15.4144373299162));
#100332=CARTESIAN_POINT('Ctrl Pts',(-0.199381979216108,-2.93561790365231,
15.4170146749183));
#100333=CARTESIAN_POINT('Ctrl Pts',(-0.152099230062562,-2.93806566029665,
15.4195920199205));
#100334=CARTESIAN_POINT('Ctrl Pts',(-0.0594165212255564,-2.94286370441279,
15.4246440805702));
#100335=CARTESIAN_POINT('Ctrl Pts',(0.0336599841104272,-2.94328048767179,
15.42969614122));
#100336=CARTESIAN_POINT('Ctrl Pts',(0.126681219222801,-2.93927131593806,
15.4347482018697));
#100337=CARTESIAN_POINT('Ctrl Pts',(0.219574073886284,-2.93526767734163,
15.4397932900704));
#100338=CARTESIAN_POINT('Ctrl Pts',(0.312411369872398,-2.92685024074075,
15.4448383782712));
#100339=CARTESIAN_POINT('Ctrl Pts',(0.404740889785965,-2.91402622022096,
15.449883466472));
#100340=CARTESIAN_POINT('Ctrl Pts',(0.496971519515494,-2.90121593495887,
15.4549231510954));
#100341=CARTESIAN_POINT('Ctrl Pts',(0.588695016458655,-2.88400850766301,
15.4599628357188));
#100342=CARTESIAN_POINT('Ctrl Pts',(0.679462248909604,-2.86246310933551,
15.4650025203423));
#100343=CARTESIAN_POINT('Ctrl Pts',(0.770163974567093,-2.84093326034139,
15.4700385678208));
#100344=CARTESIAN_POINT('Ctrl Pts',(0.859910376427894,-2.8150717653556,
15.4750746152993));
#100345=CARTESIAN_POINT('Ctrl Pts',(0.948261551100615,-2.78498905396489,
15.4801106627778));
#100346=CARTESIAN_POINT('Ctrl Pts',(1.03658054591503,-2.75491729950139,
15.4851448759933));
#100347=CARTESIAN_POINT('Ctrl Pts',(1.1235049029231,-2.72062752604819,15.4901790892087));
#100348=CARTESIAN_POINT('Ctrl Pts',(1.20860995221491,-2.68227999720519,
15.4952133024242));
#100349=CARTESIAN_POINT('Ctrl Pts',(1.29370781771518,-2.64393570531059,
15.5002470906973));
#100350=CARTESIAN_POINT('Ctrl Pts',(1.3769862758226,-2.60153452171618,15.5052808789704));
#100351=CARTESIAN_POINT('Ctrl Pts',(1.45804177721246,-2.55528436302169,
15.5103146672436));
#100352=CARTESIAN_POINT('Ctrl Pts',(1.53911311697834,-2.5090251669714,15.5153494391271));
#100353=CARTESIAN_POINT('Ctrl Pts',(1.61796025167456,-2.45891572266182,
15.5203842110106));
#100354=CARTESIAN_POINT('Ctrl Pts',(1.6942063250659,-2.40520870780618,15.5254189828941));
#100355=CARTESIAN_POINT('Ctrl Pts',(1.77053622139873,-2.35144264886128,
15.5304592898742));
#100356=CARTESIAN_POINT('Ctrl Pts',(1.84425898462451,-2.29407138079774,
15.5354995968544));
#100357=CARTESIAN_POINT('Ctrl Pts',(1.91502898781745,-2.23338934711771,
15.5405399038346));
#100358=CARTESIAN_POINT('Ctrl Pts',(1.98584244823186,-2.17267005086233,
15.5455833058795));
#100359=CARTESIAN_POINT('Ctrl Pts',(2.0536992160296,-2.10863624636823,15.5506267079244));
#100360=CARTESIAN_POINT('Ctrl Pts',(2.11829044062721,-2.04161935951523,
15.5556701099692));
#100361=CARTESIAN_POINT('Ctrl Pts',(2.18298640572505,-1.97449379873173,
15.5607216903457));
#100362=CARTESIAN_POINT('Ctrl Pts',(2.24440596360011,-1.90437583218216,
15.5657732707222));
#100363=CARTESIAN_POINT('Ctrl Pts',(2.3022805779055,-1.8316299136559,15.5708248510986));
#100364=CARTESIAN_POINT('Ctrl Pts',(2.33180853486532,-1.79451453281014,
15.5734021961008));
#100365=CARTESIAN_POINT('Ctrl Pts',(2.36041440409863,-1.75671554066214,
15.5759795411031));
#100366=CARTESIAN_POINT('Ctrl Pts',(2.38806701673623,-1.71828400550564,
15.5785568861053));
#100367=CARTESIAN_POINT('Ctrl Pts',(2.44227112059056,-1.64295127111975,
15.583608946755));
#100368=CARTESIAN_POINT('Ctrl Pts',(2.49300451506521,-1.56491581610779,
15.5886610074047));
#100369=CARTESIAN_POINT('Ctrl Pts',(2.53998653730253,-1.48453103380222,
15.5937130680545));
#100370=CARTESIAN_POINT('Ctrl Pts',(2.58690371872048,-1.40425719212675,
15.5987581562552));
#100371=CARTESIAN_POINT('Ctrl Pts',(2.6300795936601,-1.32164084635823,15.603803244456));
#100372=CARTESIAN_POINT('Ctrl Pts',(2.66927543951866,-1.23706613727096,
15.6088483326568));
#100373=CARTESIAN_POINT('Ctrl Pts',(2.70842930438981,-1.15258201252289,
15.6138880172802));
#100374=CARTESIAN_POINT('Ctrl Pts',(2.74361142736925,-1.06614409452229,
15.6189277019036));
#100375=CARTESIAN_POINT('Ctrl Pts',(2.7746284428391,-0.97816205415477,15.6239673865271));
#100376=CARTESIAN_POINT('Ctrl Pts',(2.80562307330092,-0.890243510505094,
15.6290034340056));
#100377=CARTESIAN_POINT('Ctrl Pts',(2.83245842371054,-0.800783477315732,
15.6340394814841));
#100378=CARTESIAN_POINT('Ctrl Pts',(2.85498922330515,-0.710211612698273,
15.6390755289626));
#100379=CARTESIAN_POINT('Ctrl Pts',(2.87751181658058,-0.61967273677373,
15.644109742178));
#100380=CARTESIAN_POINT('Ctrl Pts',(2.8957328665444,-0.528023264636981,
15.6491439553935));
#100381=CARTESIAN_POINT('Ctrl Pts',(2.9095572501116,-0.435707021200076,
15.654178168609));
#100382=CARTESIAN_POINT('Ctrl Pts',(2.9233804667505,-0.343398570257963,
15.6592119568821));
#100383=CARTESIAN_POINT('Ctrl Pts',(2.93280768924939,-0.250423899347588,
15.6642457451552));
#100384=CARTESIAN_POINT('Ctrl Pts',(2.93779529508008,-0.157234869559293,
15.6692795334283));
#100385=CARTESIAN_POINT('Ctrl Pts',(2.94278387549704,-0.0640276304835271,
15.6743143053118));
#100386=CARTESIAN_POINT('Ctrl Pts',(2.94333109299994,0.0293936069942164,
15.6793490771953));
#100387=CARTESIAN_POINT('Ctrl Pts',(2.93944541048168,0.122575196504791,
15.6843838490788));
#100388=CARTESIAN_POINT('Ctrl Pts',(2.93555545614557,0.215859227420616,
15.689424156059));
#100389=CARTESIAN_POINT('Ctrl Pts',(2.92722289237642,0.308902639857464,
15.6944644630392));
#100390=CARTESIAN_POINT('Ctrl Pts',(2.91450820443112,0.401255437724781,
15.6995047700194));
#100391=CARTESIAN_POINT('Ctrl Pts',(2.90178570886979,0.493664946003564,
15.7045481720643));
#100392=CARTESIAN_POINT('Ctrl Pts',(2.88467581350687,0.585382559004776,
15.7095915741092));
#100393=CARTESIAN_POINT('Ctrl Pts',(2.86329000659806,0.675969184294437,
15.714634976154));
#100394=CARTESIAN_POINT('Ctrl Pts',(2.84186952067322,0.766702703972665,
15.7196865565305));
#100395=CARTESIAN_POINT('Ctrl Pts',(2.81615940307745,0.856301148020783,
15.724738136907));
#100396=CARTESIAN_POINT('Ctrl Pts',(2.78632073513565,0.944341442992474,
15.7297897172834));
#100397=CARTESIAN_POINT('Ctrl Pts',(2.77109687726129,0.989260101576055,
15.7323670622856));
#100398=CARTESIAN_POINT('Ctrl Pts',(2.75479908941012,1.03377348914806,15.7349444072878));
#100399=CARTESIAN_POINT('Ctrl Pts',(2.73745343916241,1.07782775452198,15.73752175229));
#100400=CARTESIAN_POINT('Ctrl Pts',(2.70345283893801,1.16418205336739,15.7425738129398));
#100401=CARTESIAN_POINT('Ctrl Pts',(2.66530100448761,1.24908109389148,15.7476258735895));
#100402=CARTESIAN_POINT('Ctrl Pts',(2.62314315306257,1.33209759347465,15.7526779342392));
#100403=CARTESIAN_POINT('Ctrl Pts',(2.58104348452323,1.41499952034257,15.75772302244));
#100404=CARTESIAN_POINT('Ctrl Pts',(2.53494898479218,1.49602367636708,15.7627681106407));
#100405=CARTESIAN_POINT('Ctrl Pts',(2.48505342689035,1.57476139954614,15.7678131988415));
#100406=CARTESIAN_POINT('Ctrl Pts',(2.43521130997793,1.65341479013114,15.772852883465));
#100407=CARTESIAN_POINT('Ctrl Pts',(2.38157646343374,1.72978624213928,15.7778925680884));
#100408=CARTESIAN_POINT('Ctrl Pts',(2.32438867868526,1.80349141123538,15.7829322527118));
#100409=CARTESIAN_POINT('Ctrl Pts',(2.26724216641271,1.87714338724433,15.7879683001903));
#100410=CARTESIAN_POINT('Ctrl Pts',(2.2065480841259,1.94813255504624,15.7930043476688));
#100411=CARTESIAN_POINT('Ctrl Pts',(2.14258906308966,2.01610419044467,15.7980403951473));
#100412=CARTESIAN_POINT('Ctrl Pts',(2.07865333763776,2.08405106875741,15.8030746083628));
#100413=CARTESIAN_POINT('Ctrl Pts',(2.01145534001924,2.14898227482019,15.8081088215782));
#100414=CARTESIAN_POINT('Ctrl Pts',(1.94131675858346,2.21057758127667,15.8131430347937));
#100415=CARTESIAN_POINT('Ctrl Pts',(1.87118409760659,2.27216768841954,15.8181768230668));
#100416=CARTESIAN_POINT('Ctrl Pts',(1.79811168028328,2.33042216276658,15.8232106113399));
#100417=CARTESIAN_POINT('Ctrl Pts',(1.72245582958902,2.3850597298841,15.828244399613));
#100418=CARTESIAN_POINT('Ctrl Pts',(1.64678519561889,2.43970797327081,15.8332791714965));
#100419=CARTESIAN_POINT('Ctrl Pts',(1.56853048612015,2.49073764601253,15.83831394338));
#100420=CARTESIAN_POINT('Ctrl Pts',(1.4880777193723,2.53791030202167,15.8433487152635));
#100421=CARTESIAN_POINT('Ctrl Pts',(1.40753650495438,2.58513481841653,15.8483890222437));
#100422=CARTESIAN_POINT('Ctrl Pts',(1.32479279354661,2.62849362881679,15.8534293292239));
#100423=CARTESIAN_POINT('Ctrl Pts',(1.2402576942461,2.66779400476561,15.8584696362041));
#100424=CARTESIAN_POINT('Ctrl Pts',(1.15567068509158,2.70711851361066,15.863513038249));
#100425=CARTESIAN_POINT('Ctrl Pts',(1.06929050916347,2.74237945886987,15.8685564402938));
#100426=CARTESIAN_POINT('Ctrl Pts',(0.981546715764777,2.77343289891271,
15.8735998423387));
#100427=CARTESIAN_POINT('Ctrl Pts',(0.893660637886069,2.80453669491121,
15.8786514227152));
#100428=CARTESIAN_POINT('Ctrl Pts',(0.804406952963284,2.83141923664927,
15.8837030030916));
#100429=CARTESIAN_POINT('Ctrl Pts',(0.714228586201955,2.85398695278236,
15.8887545834681));
#100430=CARTESIAN_POINT('Ctrl Pts',(0.668219071246137,2.86550112974337,
15.8913319284703));
#100431=CARTESIAN_POINT('Ctrl Pts',(0.621968992648011,2.87589294342898,
15.8939092734725));
#100432=CARTESIAN_POINT('Ctrl Pts',(0.57553774039783,2.88515516209748,15.8964866184747));
#100433=CARTESIAN_POINT('Ctrl Pts',(0.484524118935146,2.90331077976762,
15.9015386791245));
#100434=CARTESIAN_POINT('Ctrl Pts',(0.392487023563346,2.91718819413048,
15.9065907397742));
#100435=CARTESIAN_POINT('Ctrl Pts',(0.299864331334389,2.9266782164757,15.911642800424));
#100436=CARTESIAN_POINT('Ctrl Pts',(0.207369469517258,2.93615514145314,
15.9166878886247));
#100437=CARTESIAN_POINT('Ctrl Pts',(0.114291054966479,2.94125666178667,
15.9217329768255));
#100438=CARTESIAN_POINT('Ctrl Pts',(0.0210775916233303,2.94192449514452,
15.9267780650263));
#100439=CARTESIAN_POINT('Ctrl Pts',(-0.0720360347817216,2.94259161321474,
15.9318177496498));
#100440=CARTESIAN_POINT('Ctrl Pts',(-0.165283980577547,2.93883447993254,
15.9368574342732));
#100441=CARTESIAN_POINT('Ctrl Pts',(-0.25821327864767,2.93064666971814,
15.9418971188966));
#100442=CARTESIAN_POINT('Ctrl Pts',(-0.351075509559587,2.92246476865375,
15.9469331663751));
#100443=CARTESIAN_POINT('Ctrl Pts',(-0.443619108526811,2.90985858524784,
15.9519692138537));
#100444=CARTESIAN_POINT('Ctrl Pts',(-0.535392824290577,2.8928737483164,
15.9570052613322));
#100445=CARTESIAN_POINT('Ctrl Pts',(-0.627133113615048,2.87589509771637,
15.9620394745476));
#100446=CARTESIAN_POINT('Ctrl Pts',(-0.718103640360218,2.85454104263448,
15.9670736877631));
#100447=CARTESIAN_POINT('Ctrl Pts',(-0.807861017208068,2.82890872544088,
15.9721079009785));
#100448=CARTESIAN_POINT('Ctrl Pts',(-0.89761081755764,2.80327857189348,
15.9771416892517));
#100449=CARTESIAN_POINT('Ctrl Pts',(-0.986147244435183,2.77337099641894,
15.9821754775248));
#100450=CARTESIAN_POINT('Ctrl Pts',(-1.07304091515667,2.73933334853568,
15.987209265798));
#100451=CARTESIAN_POINT('Ctrl Pts',(-1.1599515650417,2.70528904964109,15.9922440376815));
#100452=CARTESIAN_POINT('Ctrl Pts',(-1.24521840773356,2.66711323797731,
15.997278809565));
#100453=CARTESIAN_POINT('Ctrl Pts',(-1.32843199742465,2.62500141489836,
16.0023135814485));
#100454=CARTESIAN_POINT('Ctrl Pts',(-1.41173706996259,2.58284329518112,
16.0073538884287));
#100455=CARTESIAN_POINT('Ctrl Pts',(-1.49298398661229,2.5367407274459,16.0123941954089));
#100456=CARTESIAN_POINT('Ctrl Pts',(-1.57178816026574,2.48693505730416,
16.017434502389));
#100457=CARTESIAN_POINT('Ctrl Pts',(-1.65064072462551,2.43709880335645,
16.0224779044339));
#100458=CARTESIAN_POINT('Ctrl Pts',(-1.72704719620449,2.38355517483878,
16.0275213064788));
#100459=CARTESIAN_POINT('Ctrl Pts',(-1.80065402727287,2.32658743099545,
16.0325647085237));
#100460=CARTESIAN_POINT('Ctrl Pts',(-1.87438021846099,2.26952730881402,
16.0376162889001));
#100461=CARTESIAN_POINT('Ctrl Pts',(-1.94529736818064,2.20903227432121,
16.0426678692766));
#100462=CARTESIAN_POINT('Ctrl Pts',(-2.01308704083513,2.14542409933833,
16.0477194496531));
#100463=CARTESIAN_POINT('Ctrl Pts',(-2.04767371688367,2.11297084715366,
16.0502967946552));
#100464=CARTESIAN_POINT('Ctrl Pts',(-2.08144690046443,2.07970778005639,
16.0528741396574));
#100465=CARTESIAN_POINT('Ctrl Pts',(-2.11436836273714,2.04568092004992,
16.0554514846596));
#100466=CARTESIAN_POINT('Ctrl Pts',(-2.17949801956193,1.97836441701341,
16.0605503345867));
#100467=CARTESIAN_POINT('Ctrl Pts',(-2.24154457972021,1.9077946655625,16.0656491845138));
#100468=CARTESIAN_POINT('Ctrl Pts',(-2.30016070585547,1.83429134197337,
16.0707480344409));
#100469=CARTESIAN_POINT('Ctrl Pts',(-2.35739165283549,1.76252500235759,
16.075726391577));
#100470=CARTESIAN_POINT('Ctrl Pts',(-2.41135216583501,1.68796256164301,
16.0807047487132));
#100471=CARTESIAN_POINT('Ctrl Pts',(-2.46175467667096,1.61094007085573,
16.0856831058493));
#100472=CARTESIAN_POINT('Ctrl Pts',(-2.51210957595231,1.53399033756533,
16.0906567602966));
#100473=CARTESIAN_POINT('Ctrl Pts',(-2.55891289594708,1.45458554692395,
16.095630414744));
#100474=CARTESIAN_POINT('Ctrl Pts',(-2.601917966428,1.37309391375069,16.1006040691913));
#100475=CARTESIAN_POINT('Ctrl Pts',(-2.6448951938005,1.2916550413415,16.1055745035068));
#100476=CARTESIAN_POINT('Ctrl Pts',(-2.68407884249686,1.20813241238184,
16.1105449378222));
#100477=CARTESIAN_POINT('Ctrl Pts',(-2.71926683982214,1.12292112538846,
16.1155153721376));
#100478=CARTESIAN_POINT('Ctrl Pts',(-2.75602606398772,1.03390495401982,
16.1207077480353));
#100479=CARTESIAN_POINT('Ctrl Pts',(-2.78842422023279,0.943046257073344,
16.1259001239331));
#100480=CARTESIAN_POINT('Ctrl Pts',(-2.81628627618475,0.850820551334667,
16.1310924998308));
#100481=CARTESIAN_POINT('Ctrl Pts',(-2.84295512294477,0.762544466543243,
16.1360625091286));
#100482=CARTESIAN_POINT('Ctrl Pts',(-2.86546831287009,0.673016534318072,
16.1410325184264));
#100483=CARTESIAN_POINT('Ctrl Pts',(-2.88372341249344,0.582669100122154,
16.1460025277242));
#100484=CARTESIAN_POINT('Ctrl Pts',(-2.90198198245374,0.492304490668651,
16.1509734818323));
#100485=CARTESIAN_POINT('Ctrl Pts',(-2.91598077466729,0.401120519722664,
16.1559444359405));
#100486=CARTESIAN_POINT('Ctrl Pts',(-2.92566878415543,0.309558016240055,
16.1609153900486));
#100487=CARTESIAN_POINT('Ctrl Pts',(-2.93536485446695,0.217919328978934,
16.1658904801955));
#100488=CARTESIAN_POINT('Ctrl Pts',(-2.94074295664986,0.125901936329462,
16.1708655703425));
#100489=CARTESIAN_POINT('Ctrl Pts',(-2.9418041153148,0.0339491843337573,
16.1758406604894));
#100490=CARTESIAN_POINT('Ctrl Pts',(-2.94194511869995,0.0217307953837703,
16.1765017346297));
#100491=CARTESIAN_POINT('Ctrl Pts',(-2.94200997631809,0.00951354392413586,
16.1771628087701));
#100492=CARTESIAN_POINT('Ctrl Pts',(-2.94199875963773,-0.00270153476367689,
16.1778238829104));
#100493=CARTESIAN_POINT('',(-2.9422462097844,0.00107083704094043,17.1778238829104));
#100494=CARTESIAN_POINT('Ctrl Pts',(-2.94208124408393,-0.00270161050626413,
16.1778238829104));
#100495=CARTESIAN_POINT('Ctrl Pts',(-2.94416292838268,-0.228090639137221,
16.1900213722217));
#100496=CARTESIAN_POINT('Ctrl Pts',(-2.81747124271292,-1.43029794424299,
16.2552071502614));
#100497=CARTESIAN_POINT('Ctrl Pts',(-1.16691403270231,-3.27719121187224,
16.3733812170289));
#100498=CARTESIAN_POINT('Ctrl Pts',(2.12388606133514,-2.75513676563843,
16.5323460832138));
#100499=CARTESIAN_POINT('Ctrl Pts',(3.46626230468908,0.294442242197471,
16.6913109493985));
#100500=CARTESIAN_POINT('Ctrl Pts',(1.62873720110606,3.07390398819469,16.8502758155833));
#100501=CARTESIAN_POINT('Ctrl Pts',(-1.7029690014089,3.03340850845079,17.0092406817681));
#100502=CARTESIAN_POINT('Ctrl Pts',(-2.91827323464354,1.0942644108035,17.118423370877));
#100503=CARTESIAN_POINT('Ctrl Pts',(-2.94665605505738,0.0600914372647645,
17.1746177712579));
#100504=CARTESIAN_POINT('Ctrl Pts',(-2.9463796754372,0.00107234142494241,
17.1778238829104));
#100505=CARTESIAN_POINT('',(-2.94199923877503,0.00211637595187146,18.1778238442168));
#100506=CARTESIAN_POINT('Ctrl Pts',(-2.94199980514957,0.00107074736142649,
17.1778238829104));
#100507=CARTESIAN_POINT('Ctrl Pts',(-2.94203329402139,-0.0909437258276088,
17.1828298628248));
#100508=CARTESIAN_POINT('Ctrl Pts',(-2.9377457510742,-0.183133975815443,
17.1878358427392));
#100509=CARTESIAN_POINT('Ctrl Pts',(-2.92911390110944,-0.275055911275205,
17.1928418226536));
#100510=CARTESIAN_POINT('Ctrl Pts',(-2.92049354800805,-0.366855414818711,
17.1978411350439));
#100511=CARTESIAN_POINT('Ctrl Pts',(-2.90754042312244,-0.458386866549597,
17.2028404474343));
#100512=CARTESIAN_POINT('Ctrl Pts',(-2.89028326165503,-0.549205487405925,
17.2078397598246));
#100513=CARTESIAN_POINT('Ctrl Pts',(-2.87304432078033,-0.639928219427667,
17.2128337938014));
#100514=CARTESIAN_POINT('Ctrl Pts',(-2.85151045925375,-0.729939173642679,
17.2178278277782));
#100515=CARTESIAN_POINT('Ctrl Pts',(-2.82576214795534,-0.818799293589582,
17.222821861755));
#100516=CARTESIAN_POINT('Ctrl Pts',(-2.80002863466342,-0.907608344065715,
17.2278130255728));
#100517=CARTESIAN_POINT('Ctrl Pts',(-2.77008560583347,-0.995267439275946,
17.2328041893907));
#100518=CARTESIAN_POINT('Ctrl Pts',(-2.73606426772405,-1.0813493065997,
17.2377953532085));
#100519=CARTESIAN_POINT('Ctrl Pts',(-2.70205254225591,-1.16740685171399,
17.2427851067858));
#100520=CARTESIAN_POINT('Ctrl Pts',(-2.66396496251153,-1.25188763292986,
17.2477748603632));
#100521=CARTESIAN_POINT('Ctrl Pts',(-2.62198166987877,-1.33438230009985,
17.2527646139405));
#100522=CARTESIAN_POINT('Ctrl Pts',(-2.57999797332518,-1.41687776095018,
17.2577544155243));
#100523=CARTESIAN_POINT('Ctrl Pts',(-2.53411869616048,-1.49738666660656,
17.262744217108));
#100524=CARTESIAN_POINT('Ctrl Pts',(-2.48457035483657,-1.57552345329014,
17.2677340186917));
#100525=CARTESIAN_POINT('Ctrl Pts',(-2.43497377683174,-1.65373630829703,
17.2727286779853));
#100526=CARTESIAN_POINT('Ctrl Pts',(-2.38170124307166,-1.72957204808033,
17.2777233372789));
#100527=CARTESIAN_POINT('Ctrl Pts',(-2.3250229238281,-1.80267368197183,
17.2827179965725));
#100528=CARTESIAN_POINT('Ctrl Pts',(-2.26831796501701,-1.87580967460821,
17.2877150034227));
#100529=CARTESIAN_POINT('Ctrl Pts',(-2.20820432795751,-1.94620865790778,
17.292712010273));
#100530=CARTESIAN_POINT('Ctrl Pts',(-2.14499132103499,-2.01354816994393,
17.2977090171232));
#100531=CARTESIAN_POINT('Ctrl Pts',(-2.08166776344506,-2.08100544932516,
17.3027147630363));
#100532=CARTESIAN_POINT('Ctrl Pts',(-2.01523433286974,-2.14539225199398,
17.3077205089494));
#100533=CARTESIAN_POINT('Ctrl Pts',(-1.94603592045869,-2.20642430105465,
17.3127262548625));
#100534=CARTESIAN_POINT('Ctrl Pts',(-1.87947821472108,-2.26512728310883,
17.3175409746208));
#100535=CARTESIAN_POINT('Ctrl Pts',(-1.8103630377244,-2.32072672154925,
17.3223556943792));
#100536=CARTESIAN_POINT('Ctrl Pts',(-1.73902209390058,-2.37300782909068,
17.3271704141375));
#100537=CARTESIAN_POINT('Ctrl Pts',(-1.66416440890601,-2.42786612601998,
17.3322224747872));
#100538=CARTESIAN_POINT('Ctrl Pts',(-1.58657387127427,-2.47927738960965,
17.337274535437));
#100539=CARTESIAN_POINT('Ctrl Pts',(-1.50660141597608,-2.52695788911863,
17.3423265960867));
#100540=CARTESIAN_POINT('Ctrl Pts',(-1.42673933224742,-2.57457258382585,
17.3473716842875));
#100541=CARTESIAN_POINT('Ctrl Pts',(-1.34450224148032,-2.61846652039016,
17.3524167724883));
#100542=CARTESIAN_POINT('Ctrl Pts',(-1.26027219027686,-2.65839763888226,
17.357461860689));
#100543=CARTESIAN_POINT('Ctrl Pts',(-1.17613235426424,-2.69828598886806,
17.3625015453125));
#100544=CARTESIAN_POINT('Ctrl Pts',(-1.09000419990067,-2.73421976784508,
17.3675412299359));
#100545=CARTESIAN_POINT('Ctrl Pts',(-1.00229569805139,-2.76600204874611,
17.3725809145594));
#100546=CARTESIAN_POINT('Ctrl Pts',(-0.914650495507,-2.79776139234635,17.3776169620379));
#100547=CARTESIAN_POINT('Ctrl Pts',(-0.825427628969259,-2.82537504217137,
17.3826530095164));
#100548=CARTESIAN_POINT('Ctrl Pts',(-0.735055474742115,-2.84869399006837,
17.3876890569949));
#100549=CARTESIAN_POINT('Ctrl Pts',(-0.644716236468095,-2.87200444458151,
17.3927232702103));
#100550=CARTESIAN_POINT('Ctrl Pts',(-0.553228971873109,-2.8910231937955,
17.3977574834258));
#100551=CARTESIAN_POINT('Ctrl Pts',(-0.461036660377981,-2.90565125192056,
17.4027916966413));
#100552=CARTESIAN_POINT('Ctrl Pts',(-0.368852130916373,-2.92027807527846,
17.4078254849144));
#100553=CARTESIAN_POINT('Ctrl Pts',(-0.275963111721861,-2.93051487497566,
17.4128592731875));
#100554=CARTESIAN_POINT('Ctrl Pts',(-0.182821066728011,-2.93631409381906,
17.4178930614606));
#100555=CARTESIAN_POINT('Ctrl Pts',(-0.089660821627973,-2.94211444583919,
17.4229278333441));
#100556=CARTESIAN_POINT('Ctrl Pts',(0.00375210402130081,-2.94347546768573,
17.4279626052276));
#100557=CARTESIAN_POINT('Ctrl Pts',(0.0969640073408292,-2.94040167005809,
17.4329973771111));
#100558=CARTESIAN_POINT('Ctrl Pts',(0.19027838539218,-2.93732449317763,
17.4380376840913));
#100559=CARTESIAN_POINT('Ctrl Pts',(0.283390855220886,-2.92980277932503,
17.4430779910715));
#100560=CARTESIAN_POINT('Ctrl Pts',(0.375850910903049,-2.9178930913886,
17.4481182980517));
#100561=CARTESIAN_POINT('Ctrl Pts',(0.468367742859676,-2.90597609015666,
17.4531617000966));
#100562=CARTESIAN_POINT('Ctrl Pts',(0.560230925968129,-2.88966582825894,
17.4582051021415));
#100563=CARTESIAN_POINT('Ctrl Pts',(0.651000413242353,-2.86906996463284,
17.4632485041864));
#100564=CARTESIAN_POINT('Ctrl Pts',(0.741917091432303,-2.84844070295506,
17.4683000845628));
#100565=CARTESIAN_POINT('Ctrl Pts',(0.831736105545388,-2.82351208433317,
17.4733516649393));
#100566=CARTESIAN_POINT('Ctrl Pts',(0.920032994952805,-2.79444149843903,
17.4784032453158));
#100567=CARTESIAN_POINT('Ctrl Pts',(0.965082569474462,-2.77960952038844,
17.4809805903179));
#100568=CARTESIAN_POINT('Ctrl Pts',(1.0097362437424,-2.76370012265316,17.4835579353201));
#100569=CARTESIAN_POINT('Ctrl Pts',(1.05393994152964,-2.74673890270781,
17.4861352803223));
#100570=CARTESIAN_POINT('Ctrl Pts',(1.14058715483423,-2.71349185515119,
17.491187340972));
#100571=CARTESIAN_POINT('Ctrl Pts',(1.22581532789134,-2.67608105362047,
17.4962394016217));
#100572=CARTESIAN_POINT('Ctrl Pts',(1.30919592925609,-2.63464798764831,
17.5012914622715));
#100573=CARTESIAN_POINT('Ctrl Pts',(1.39246145540148,-2.59327210427111,
17.5063365504722));
#100574=CARTESIAN_POINT('Ctrl Pts',(1.47388408232774,-2.54788518336495,
17.511381638673));
#100575=CARTESIAN_POINT('Ctrl Pts',(1.55305347551471,-2.49867743060037,
17.5164267268737));
#100576=CARTESIAN_POINT('Ctrl Pts',(1.63213807376387,-2.44952238214699,
17.5214664114971));
#100577=CARTESIAN_POINT('Ctrl Pts',(1.70897385981901,-2.39655486920936,
17.5265060961205));
#100578=CARTESIAN_POINT('Ctrl Pts',(1.78317441502162,-2.34001132595812,
17.531545780744));
#100579=CARTESIAN_POINT('Ctrl Pts',(1.85732141961698,-2.28350859023278,
17.5365818282224));
#100580=CARTESIAN_POINT('Ctrl Pts',(1.92883662116874,-2.22343522244948,
17.5416178757009));
#100581=CARTESIAN_POINT('Ctrl Pts',(1.99736284684045,-2.16007075302209,
17.5466539231794));
#100582=CARTESIAN_POINT('Ctrl Pts',(2.06586411342986,-2.09672936262746,
17.5516881363949));
#100583=CARTESIAN_POINT('Ctrl Pts',(2.13137824099259,-2.03009955327481,
17.5567223496103));
#100584=CARTESIAN_POINT('Ctrl Pts',(2.19358221198335,-1.96050021149457,
17.5617565628258));
#100585=CARTESIAN_POINT('Ctrl Pts',(2.2557809322827,-1.89090674465542,17.5667903510989));
#100586=CARTESIAN_POINT('Ctrl Pts',(2.31466975560202,-1.81834457515237,
17.571824139372));
#100587=CARTESIAN_POINT('Ctrl Pts',(2.36996431412626,-1.74316756216034,
17.5768579276451));
#100588=CARTESIAN_POINT('Ctrl Pts',(2.42526967729674,-1.66797585945829,
17.5818926995286));
#100589=CARTESIAN_POINT('Ctrl Pts',(2.47697911791386,-1.59016865664336,
17.5869274714121));
#100590=CARTESIAN_POINT('Ctrl Pts',(2.52485083619738,-1.51012988016045,
17.5919622432956));
#100591=CARTESIAN_POINT('Ctrl Pts',(2.57277518339745,-1.43000311113747,
17.5970025502758));
#100592=CARTESIAN_POINT('Ctrl Pts',(2.61685315800773,-1.34764025317901,
17.602042857256));
#100593=CARTESIAN_POINT('Ctrl Pts',(2.65688845756911,-1.26345072085777,
17.6070831642362));
#100594=CARTESIAN_POINT('Ctrl Pts',(2.69694834131592,-1.17920949088231,
17.612126566281));
#100595=CARTESIAN_POINT('Ctrl Pts',(2.7329604365705,-1.09313976304902,17.6171699683259));
#100596=CARTESIAN_POINT('Ctrl Pts',(2.76477706520972,-1.00566981643594,
17.6222133703707));
#100597=CARTESIAN_POINT('Ctrl Pts',(2.7966452873838,-0.918058029410124,
17.6272649507472));
#100598=CARTESIAN_POINT('Ctrl Pts',(2.82430432917473,-0.829041914409659,
17.6323165311236));
#100599=CARTESIAN_POINT('Ctrl Pts',(2.84765676431199,-0.739063564700747,
17.6373681115001));
#100600=CARTESIAN_POINT('Ctrl Pts',(2.85957130936675,-0.693156099579488,
17.6399454565024));
#100601=CARTESIAN_POINT('Ctrl Pts',(2.8703656293677,-0.646998302644535,
17.6425228015047));
#100602=CARTESIAN_POINT('Ctrl Pts',(2.88003197548053,-0.60064949863438,
17.645100146507));
#100603=CARTESIAN_POINT('Ctrl Pts',(2.89897975576582,-0.509797490582921,
17.6501522071567));
#100604=CARTESIAN_POINT('Ctrl Pts',(2.91365841091782,-0.417884778530722,
17.6552042678065));
#100605=CARTESIAN_POINT('Ctrl Pts',(2.92395494186897,-0.325348271733616,
17.6602563284562));
#100606=CARTESIAN_POINT('Ctrl Pts',(2.9342372623738,-0.232939476402446,
17.665301416657));
#100607=CARTESIAN_POINT('Ctrl Pts',(2.9401494277896,-0.139909034798525,
17.6703465048577));
#100608=CARTESIAN_POINT('Ctrl Pts',(2.94162925092124,-0.0467049261270682,
17.6753915930585));
#100609=CARTESIAN_POINT('Ctrl Pts',(2.94310748907788,0.0463993556257909,
17.6804312776819));
#100610=CARTESIAN_POINT('Ctrl Pts',(2.94016281386149,0.139676492875248,
17.6854709623053));
#100611=CARTESIAN_POINT('Ctrl Pts',(2.932784853981,0.232673591667947,17.6905106469288));
#100612=CARTESIAN_POINT('Ctrl Pts',(2.92541221878078,0.325603574370818,
17.6955466944073));
#100613=CARTESIAN_POINT('Ctrl Pts',(2.91361269340193,0.41825347869182,17.7005827418858));
#100614=CARTESIAN_POINT('Ctrl Pts',(2.89742797392138,0.5101716730061,17.7056187893643));
#100615=CARTESIAN_POINT('Ctrl Pts',(2.88124914934808,0.602056388258219,
17.7106530025797));
#100616=CARTESIAN_POINT('Ctrl Pts',(2.86068838064425,0.693209485819634,
17.7156872157952));
#100617=CARTESIAN_POINT('Ctrl Pts',(2.83583894399186,0.783186748955274,
17.7207214290106));
#100618=CARTESIAN_POINT('Ctrl Pts',(2.81099160490214,0.87315641703148,17.7257552172838));
#100619=CARTESIAN_POINT('Ctrl Pts',(2.78185643606895,0.961950019796551,
17.7307890055569));
#100620=CARTESIAN_POINT('Ctrl Pts',(2.74857704091671,1.04913690724593,17.73582279383));
#100621=CARTESIAN_POINT('Ctrl Pts',(2.71529114291672,1.13634083115442,17.7408575657135));
#100622=CARTESIAN_POINT('Ctrl Pts',(2.67785956913586,1.22193700129747,17.745892337597));
#100623=CARTESIAN_POINT('Ctrl Pts',(2.63647424668415,1.30551428432293,17.7509271094805));
#100624=CARTESIAN_POINT('Ctrl Pts',(2.59504342629008,1.38918345003001,17.7559674164607));
#100625=CARTESIAN_POINT('Ctrl Pts',(2.54965037823171,1.47082889941229,17.7610077234409));
#100626=CARTESIAN_POINT('Ctrl Pts',(2.50053308868983,1.55006395750862,17.7660480304211));
#100627=CARTESIAN_POINT('Ctrl Pts',(2.45138563805086,1.62934767090134,17.771091432466));
#100628=CARTESIAN_POINT('Ctrl Pts',(2.39850964474591,1.70621768056698,17.7761348345108));
#100629=CARTESIAN_POINT('Ctrl Pts',(2.34218527739306,1.7803179846205,17.7811782365557));
#100630=CARTESIAN_POINT('Ctrl Pts',(2.28576957499525,1.85453844900462,17.7862298169322));
#100631=CARTESIAN_POINT('Ctrl Pts',(2.2258946200785,1.92597990123178,17.7912813973086));
#100632=CARTESIAN_POINT('Ctrl Pts',(2.16287939825066,1.99432111472121,17.7963329776851));
#100633=CARTESIAN_POINT('Ctrl Pts',(2.13072867413291,2.02918919003758,17.7989103226873));
#100634=CARTESIAN_POINT('Ctrl Pts',(2.09776107921285,2.06325085833496,17.8014876676895));
#100635=CARTESIAN_POINT('Ctrl Pts',(2.0640223007228,2.09646749130984,17.8040650126918));
#100636=CARTESIAN_POINT('Ctrl Pts',(1.99788821505217,2.16157807767854,17.8091170733415));
#100637=CARTESIAN_POINT('Ctrl Pts',(1.92855135602194,2.22367324281825,17.8141691339912));
#100638=CARTESIAN_POINT('Ctrl Pts',(1.85631792073174,2.28242147228995,17.819221194641));
#100639=CARTESIAN_POINT('Ctrl Pts',(1.78418417623612,2.34108862216667,17.8242662828418));
#100640=CARTESIAN_POINT('Ctrl Pts',(1.70916214093243,2.39641773732234,17.8293113710426));
#100641=CARTESIAN_POINT('Ctrl Pts',(1.63159482462775,2.4481140349763,17.8343564592434));
#100642=CARTESIAN_POINT('Ctrl Pts',(1.55411058734505,2.49975496294553,17.8393961438668));
#100643=CARTESIAN_POINT('Ctrl Pts',(1.47408685538507,2.54777056216937,17.8444358284902));
#100644=CARTESIAN_POINT('Ctrl Pts',(1.39189881930388,2.59190695759328,17.8494755131137));
#100645=CARTESIAN_POINT('Ctrl Pts',(1.3097700984023,2.63601149974089,17.8545115605922));
#100646=CARTESIAN_POINT('Ctrl Pts',(1.22548056832853,2.67624219312077,17.8595476080707));
#100647=CARTESIAN_POINT('Ctrl Pts',(1.13943254266561,2.71238962553586,17.8645836555492));
#100648=CARTESIAN_POINT('Ctrl Pts',(1.05341585799265,2.74852389209029,17.8696178687647));
#100649=CARTESIAN_POINT('Ctrl Pts',(0.965642359340677,2.78057768030859,
17.8746520819802));
#100650=CARTESIAN_POINT('Ctrl Pts',(0.876536046332958,2.80838896157192,
17.8796862951956));
#100651=CARTESIAN_POINT('Ctrl Pts',(0.787437254866824,2.83619789526074,
17.8847200834688));
#100652=CARTESIAN_POINT('Ctrl Pts',(0.697006296905316,2.85976490179861,
17.8897538717419));
#100653=CARTESIAN_POINT('Ctrl Pts',(0.605683007306596,2.87897761274033,
17.894787660015));
#100654=CARTESIAN_POINT('Ctrl Pts',(0.514341872989364,2.89819407787686,
17.8998224318986));
#100655=CARTESIAN_POINT('Ctrl Pts',(0.422108495585902,2.91305446655337,
17.9048572037821));
#100656=CARTESIAN_POINT('Ctrl Pts',(0.329432457806434,2.92349760659105,
17.9098919756656));
#100657=CARTESIAN_POINT('Ctrl Pts',(0.236654534412013,2.93395222754408,
17.9149322826458));
#100658=CARTESIAN_POINT('Ctrl Pts',(0.143433421422785,2.9399798564246,17.919972589626));
#100659=CARTESIAN_POINT('Ctrl Pts',(0.0502230684115907,2.94157128817225,
17.9250128966062));
#100660=CARTESIAN_POINT('Ctrl Pts',(-0.043044521604017,2.94316369715882,
17.9300562986511));
#100661=CARTESIAN_POINT('Ctrl Pts',(-0.136300894717583,2.94031449942311,
17.935099700696));
#100662=CARTESIAN_POINT('Ctrl Pts',(-0.229095058405284,2.93306656150424,
17.9401431027408));
#100663=CARTESIAN_POINT('Ctrl Pts',(-0.32203969620398,2.92580687039991,
17.9451946831173));
#100664=CARTESIAN_POINT('Ctrl Pts',(-0.414520187991462,2.91413425452411,
17.9502462634938));
#100665=CARTESIAN_POINT('Ctrl Pts',(-0.506093769289275,2.89814304282701,
17.9552978438702));
#100666=CARTESIAN_POINT('Ctrl Pts',(-0.552815130624427,2.88998423578573,
17.9578751888723));
#100667=CARTESIAN_POINT('Ctrl Pts',(-0.599300622475556,2.88070206959699,
17.9604525338744));
#100668=CARTESIAN_POINT('Ctrl Pts',(-0.645493034382045,2.87031404946641,
17.9630298788766));
#100669=CARTESIAN_POINT('Ctrl Pts',(-0.736038485735576,2.84995165805682,
17.9680819395263));
#100670=CARTESIAN_POINT('Ctrl Pts',(-0.825782178460994,2.82526402613562,
17.973134000176));
#100671=CARTESIAN_POINT('Ctrl Pts',(-0.914279620297822,2.79632916086574,
17.9781860608258));
#100672=CARTESIAN_POINT('Ctrl Pts',(-1.00265492506214,2.76743422917658,
17.9832311490265));
#100673=CARTESIAN_POINT('Ctrl Pts',(-1.08978697810545,2.73430384889857,
17.9882762372273));
#100674=CARTESIAN_POINT('Ctrl Pts',(-1.1752422450961,2.69706686334275,17.993321325428));
#100675=CARTESIAN_POINT('Ctrl Pts',(-1.26060598461976,2.65986976072318,
17.9983610100514));
#100676=CARTESIAN_POINT('Ctrl Pts',(-1.34429610264826,2.61857497182734,
18.0034006946749));
#100677=CARTESIAN_POINT('Ctrl Pts',(-1.42589604143235,2.57336054198154,
18.0084403792983));
#100678=CARTESIAN_POINT('Ctrl Pts',(-1.50743708946725,2.52817874343043,
18.0134764267768));
#100679=CARTESIAN_POINT('Ctrl Pts',(-1.58689056906333,2.47908314128601,
18.0185124742553));
#100680=CARTESIAN_POINT('Ctrl Pts',(-1.66386262607719,2.42629865464734,
18.0235485217338));
#100681=CARTESIAN_POINT('Ctrl Pts',(-1.74080664781156,2.37353339352887,
18.0285827349492));
#100682=CARTESIAN_POINT('Ctrl Pts',(-1.81527067640061,2.31708216811217,
18.0336169481647));
#100683=CARTESIAN_POINT('Ctrl Pts',(-1.88688896020049,2.25721378072028,
18.0386511613802));
#100684=CARTESIAN_POINT('Ctrl Pts',(-1.95850119863849,2.19735044687123,
18.0436849496533));
#100685=CARTESIAN_POINT('Ctrl Pts',(-2.02726782910982,2.13407080963618,
18.0487187379264));
#100686=CARTESIAN_POINT('Ctrl Pts',(-2.0928562837699,2.06768386739483,18.0537525261996));
#100687=CARTESIAN_POINT('Ctrl Pts',(-2.15845755451999,2.00128395303772,
18.0587872980831));
#100688=CARTESIAN_POINT('Ctrl Pts',(-2.22087910413052,1.93177584413635,
18.0638220699666));
#100689=CARTESIAN_POINT('Ctrl Pts',(-2.27982613528375,1.85950444820043,
18.06885684185));
#100690=CARTESIAN_POINT('Ctrl Pts',(-2.33883797126325,1.78715359897963,
18.0738971488302));
#100691=CARTESIAN_POINT('Ctrl Pts',(-2.39436738273153,1.71203374355614,
18.0789374558104));
#100692=CARTESIAN_POINT('Ctrl Pts',(-2.44616090381604,1.63452159136607,
18.0839777627906));
#100693=CARTESIAN_POINT('Ctrl Pts',(-2.4979862293717,1.55696184185195,18.0890211648355));
#100694=CARTESIAN_POINT('Ctrl Pts',(-2.5460708686889,1.47700725151648,18.0940645668803));
#100695=CARTESIAN_POINT('Ctrl Pts',(-2.59020673967435,1.39506023014978,
18.0991079689252));
#100696=CARTESIAN_POINT('Ctrl Pts',(-2.6344141809579,1.31298032429216,18.1041595493017));
#100697=CARTESIAN_POINT('Ctrl Pts',(-2.67465987886471,1.22890193751765,
18.1092111296781));
#100698=CARTESIAN_POINT('Ctrl Pts',(-2.71078347608639,1.14324841822633,
18.1142627100546));
#100699=CARTESIAN_POINT('Ctrl Pts',(-2.72921394057933,1.09954750615196,
18.1168400550568));
#100700=CARTESIAN_POINT('Ctrl Pts',(-2.74657217872128,1.0554368370274,18.119417400059));
#100701=CARTESIAN_POINT('Ctrl Pts',(-2.76284194091274,1.01097399053265,
18.1219947450613));
#100702=CARTESIAN_POINT('Ctrl Pts',(-2.79968270885509,0.910293636972882,
18.1278308087982));
#100703=CARTESIAN_POINT('Ctrl Pts',(-2.83104886874699,0.807508598495934,
18.1336668725351));
#100704=CARTESIAN_POINT('Ctrl Pts',(-2.85672911385411,0.703180467631383,
18.1395029362721));
#100705=CARTESIAN_POINT('Ctrl Pts',(-2.88229461777721,0.599318482366823,
18.1453129240561));
#100706=CARTESIAN_POINT('Ctrl Pts',(-2.90222479222233,0.493927308134397,
18.1511229118401));
#100707=CARTESIAN_POINT('Ctrl Pts',(-2.91635794815504,0.387582659871288,
18.1569328996241));
#100708=CARTESIAN_POINT('Ctrl Pts',(-2.93038160278863,0.282061951936535,
18.1626978726065));
#100709=CARTESIAN_POINT('Ctrl Pts',(-2.93869761945983,0.175602649068792,
18.1684628455889));
#100710=CARTESIAN_POINT('Ctrl Pts',(-2.941195752608,0.068786225660934,18.1742278185713));
#100711=CARTESIAN_POINT('Ctrl Pts',(-2.94171517399957,0.0465765466729996,
18.1754264937864));
#100712=CARTESIAN_POINT('Ctrl Pts',(-2.9419832435771,0.0243514897462521,
18.1766251690016));
#100713=CARTESIAN_POINT('Ctrl Pts',(-2.94199923877503,0.00211637595187146,
18.1778238442168));
#100714=CARTESIAN_POINT('',(-2.94199929009827,-0.00204378601551511,19.1778239218877));
#100715=CARTESIAN_POINT('Ctrl Pts',(-2.9388439218794,0.0021133891354786,
18.1778238829104));
#100716=CARTESIAN_POINT('Ctrl Pts',(-2.93462424779457,-0.634919682450241,
18.2122024590223));
#100717=CARTESIAN_POINT('Ctrl Pts',(-2.41790829107791,-2.26005798993625,
18.2995693238623));
#100718=CARTESIAN_POINT('Ctrl Pts',(0.264235245208259,-3.46869576845375,
18.4399244774308));
#100719=CARTESIAN_POINT('Ctrl Pts',(3.05959885035108,-1.65545325329123,
18.5988893436155));
#100720=CARTESIAN_POINT('Ctrl Pts',(3.04812856639187,1.67647929949768,18.7578542098002));
#100721=CARTESIAN_POINT('Ctrl Pts',(0.240347074017613,3.4704328091634,18.916819075985));
#100722=CARTESIAN_POINT('Ctrl Pts',(-2.4264532086293,2.24655052879084,19.0568089670217));
#100723=CARTESIAN_POINT('Ctrl Pts',(-2.93467894617267,0.628302831224356,
19.1438105693302));
#100724=CARTESIAN_POINT('Ctrl Pts',(-2.93869762167607,-0.00204077003662013,
19.1778238829104));
#100725=CARTESIAN_POINT('',(-2.94219292041373,-0.00118371768616264,20.1778238829104));
#100726=CARTESIAN_POINT('Ctrl Pts',(-2.94199929009827,-0.00204378601551511,
19.1778239218877));
#100727=CARTESIAN_POINT('Ctrl Pts',(-2.94192528935904,-0.108566739313825,
19.183565473421));
#100728=CARTESIAN_POINT('Ctrl Pts',(-2.93606185133819,-0.214861265836627,
19.1893070249543));
#100729=CARTESIAN_POINT('Ctrl Pts',(-2.92450720316344,-0.320346091977305,
19.1950485764876));
#100730=CARTESIAN_POINT('Ctrl Pts',(-2.91289326540157,-0.426372185294256,
19.2008195892572));
#100731=CARTESIAN_POINT('Ctrl Pts',(-2.89552968666625,-0.531580070789771,
19.2065906020268));
#100732=CARTESIAN_POINT('Ctrl Pts',(-2.87256561562812,-0.63539813023885,
19.2123616147964));
#100733=CARTESIAN_POINT('Ctrl Pts',(-2.84946366066775,-0.73983954785524,
19.2181672786465));
#100734=CARTESIAN_POINT('Ctrl Pts',(-2.82069386446977,-0.842874227815561,
19.2239729424967));
#100735=CARTESIAN_POINT('Ctrl Pts',(-2.7864562018921,-0.943941648057266,
19.2297786063469));
#100736=CARTESIAN_POINT('Ctrl Pts',(-2.77668596695865,-0.972782765281283,
19.2314353403494));
#100737=CARTESIAN_POINT('Ctrl Pts',(-2.76647075879212,-1.00146382400338,
19.233092074352));
#100738=CARTESIAN_POINT('Ctrl Pts',(-2.75581591881844,-1.02997214602478,
19.2347488083546));
#100739=CARTESIAN_POINT('Ctrl Pts',(-2.72332494701671,-1.11690569821321,
19.2398008690043));
#100740=CARTESIAN_POINT('Ctrl Pts',(-2.68665801747615,-1.20245653591761,
19.2448529296541));
#100741=CARTESIAN_POINT('Ctrl Pts',(-2.64595288127318,-1.28619491138869,
19.2499049903038));
#100742=CARTESIAN_POINT('Ctrl Pts',(-2.60530392303494,-1.36981771786916,
19.2549500785046));
#100743=CARTESIAN_POINT('Ctrl Pts',(-2.56062802532435,-1.45163263661067,
19.2599951667053));
#100744=CARTESIAN_POINT('Ctrl Pts',(-2.51211181202702,-1.53122769171483,
19.2650402549061));
#100745=CARTESIAN_POINT('Ctrl Pts',(-2.46364756236242,-1.61073749597335,
19.2700799395295));
#100746=CARTESIAN_POINT('Ctrl Pts',(-2.41135140268535,-1.68803178508086,
19.275119624153));
#100747=CARTESIAN_POINT('Ctrl Pts',(-2.35545639196684,-1.76272209538048,
19.2801593087764));
#100748=CARTESIAN_POINT('Ctrl Pts',(-2.29960172072789,-1.83735850161591,
19.2851953562549));
#100749=CARTESIAN_POINT('Ctrl Pts',(-2.24015362635919,-1.90939430969625,
19.2902314037334));
#100750=CARTESIAN_POINT('Ctrl Pts',(-2.17738851721032,-1.97846992525048,
19.2952674512119));
#100751=CARTESIAN_POINT('Ctrl Pts',(-2.11464626879112,-2.04752038162,19.3003016644273));
#100752=CARTESIAN_POINT('Ctrl Pts',(-2.0485897041775,-2.11361245887728,
19.3053358776428));
#100753=CARTESIAN_POINT('Ctrl Pts',(-1.97953488388095,-2.17642037380154,
19.3103700908583));
#100754=CARTESIAN_POINT('Ctrl Pts',(-1.91048589256215,-2.23922298705479,
19.3154038791314));
#100755=CARTESIAN_POINT('Ctrl Pts',(-1.83843947755403,-2.29874169032879,
19.3204376674045));
#100756=CARTESIAN_POINT('Ctrl Pts',(-1.76374700737692,-2.3546890440075,
19.3254714556776));
#100757=CARTESIAN_POINT('Ctrl Pts',(-1.68903994217004,-2.41064732988982,
19.3305062275611));
#100758=CARTESIAN_POINT('Ctrl Pts',(-1.61168615075386,-2.46303261420156,
19.3355409994446));
#100759=CARTESIAN_POINT('Ctrl Pts',(-1.53206743860281,-2.51159976181975,
19.3405757713281));
#100760=CARTESIAN_POINT('Ctrl Pts',(-1.45236119571956,-2.56022030289127,
19.3456160783083));
#100761=CARTESIAN_POINT('Ctrl Pts',(-1.37038544164988,-2.6050140966754,
19.3506563852885));
#100762=CARTESIAN_POINT('Ctrl Pts',(-1.28654786537196,-2.64578128160792,
19.3556966922687));
#100763=CARTESIAN_POINT('Ctrl Pts',(-1.2026588075628,-2.68657350014945,
19.3607400943136));
#100764=CARTESIAN_POINT('Ctrl Pts',(-1.11690605957456,-2.72333401247518,
19.3657834963584));
#100765=CARTESIAN_POINT('Ctrl Pts',(-1.02971659775859,-2.75591141517656,
19.3708268984033));
#100766=CARTESIAN_POINT('Ctrl Pts',(-0.942385750361367,-2.78854164507656,
19.3758784787797));
#100767=CARTESIAN_POINT('Ctrl Pts',(-0.853613960632055,-2.81697508790143,
19.3809300591562));
#100768=CARTESIAN_POINT('Ctrl Pts',(-0.763842456347477,-2.8411104698482,
19.3859816395327));
#100769=CARTESIAN_POINT('Ctrl Pts',(-0.718040524939103,-2.85342447881185,
19.3885589845348));
#100770=CARTESIAN_POINT('Ctrl Pts',(-0.671978512543133,-2.86462048595629,
19.391136329537));
#100771=CARTESIAN_POINT('Ctrl Pts',(-0.625715674144197,-2.87469022594266,
19.3937136745392));
#100772=CARTESIAN_POINT('Ctrl Pts',(-0.53503217417749,-2.89442873091386,
19.3987657351889));
#100773=CARTESIAN_POINT('Ctrl Pts',(-0.44325082061425,-2.90990751290563,
19.4038177958386));
#100774=CARTESIAN_POINT('Ctrl Pts',(-0.350807521757551,-2.92100977106862,
19.4088698564884));
#100775=CARTESIAN_POINT('Ctrl Pts',(-0.258491805728526,-2.93209670678522,
19.4139149446891));
#100776=CARTESIAN_POINT('Ctrl Pts',(-0.165516397063802,-2.9388190686146,
19.4189600328899));
#100777=CARTESIAN_POINT('Ctrl Pts',(-0.0723287162357964,-2.94111076921759,
19.4240051210907));
#100778=CARTESIAN_POINT('Ctrl Pts',(0.0207591552688803,-2.94340001527847,
19.4290448057141));
#100779=CARTESIAN_POINT('Ctrl Pts',(0.11405840525815,-2.94126802159644,
19.4340844903375));
#100780=CARTESIAN_POINT('Ctrl Pts',(0.207116247311439,-2.93470047195615,
19.439124174961));
#100781=CARTESIAN_POINT('Ctrl Pts',(0.300106929436197,-2.92813766212235,
19.4441602224394));
#100782=CARTESIAN_POINT('Ctrl Pts',(0.392856107996778,-2.91714569022534,
19.4491962699179));
#100783=CARTESIAN_POINT('Ctrl Pts',(0.484911805276166,-2.90176231643872,
19.4542323173964));
#100784=CARTESIAN_POINT('Ctrl Pts',(0.576933973411127,-2.88638454568784,
19.4592665306119));
#100785=CARTESIAN_POINT('Ctrl Pts',(0.668262724265773,-2.86661862369939,
19.4643007438274));
#100786=CARTESIAN_POINT('Ctrl Pts',(0.758453045399138,-2.84255395338853,
19.4693349570428));
#100787=CARTESIAN_POINT('Ctrl Pts',(0.848635753488712,-2.81849131439751,
19.4743687453159));
#100788=CARTESIAN_POINT('Ctrl Pts',(0.937679793678511,-2.79013076324602,
19.4794025335891));
#100789=CARTESIAN_POINT('Ctrl Pts',(1.02515328132509,-2.75761214636656,
19.4844363218622));
#100790=CARTESIAN_POINT('Ctrl Pts',(1.11264386143281,-2.72508717529671,
19.4894710937457));
#100791=CARTESIAN_POINT('Ctrl Pts',(1.19856286321372,-2.68840268004576,
19.4945058656292));
#100792=CARTESIAN_POINT('Ctrl Pts',(1.28249749697171,-2.6477469989146,19.4995406375127));
#100793=CARTESIAN_POINT('Ctrl Pts',(1.36652440627345,-2.60704662198965,
19.5045809444929));
#100794=CARTESIAN_POINT('Ctrl Pts',(1.44856219239176,-2.56236653844383,
19.5096212514731));
#100795=CARTESIAN_POINT('Ctrl Pts',(1.52822212185677,-2.51394135696671,
19.5146615584533));
#100796=CARTESIAN_POINT('Ctrl Pts',(1.60793096751581,-2.46548643939027,
19.5197049604981));
#100797=CARTESIAN_POINT('Ctrl Pts',(1.68525868167522,-2.41328209400741,
19.524748362543));
#100798=CARTESIAN_POINT('Ctrl Pts',(1.75984683531133,-2.35760537754831,
19.5297917645879));
#100799=CARTESIAN_POINT('Ctrl Pts',(1.8345559403702,-2.30183837626859,19.5348433449644));
#100800=CARTESIAN_POINT('Ctrl Pts',(1.90651627348025,-2.24258804478179,
19.5398949253408));
#100801=CARTESIAN_POINT('Ctrl Pts',(1.97540384145417,-2.18017055827476,
19.5449465057173));
#100802=CARTESIAN_POINT('Ctrl Pts',(2.01055066993215,-2.14832480211279,
19.5475238507195));
#100803=CARTESIAN_POINT('Ctrl Pts',(2.04489823803742,-2.1156551812504,19.5501011957218));
#100804=CARTESIAN_POINT('Ctrl Pts',(2.07840752093473,-2.08220704468167,
19.552678540724));
#100805=CARTESIAN_POINT('Ctrl Pts',(2.14409175388668,-2.01664266955247,
19.5577306013737));
#100806=CARTESIAN_POINT('Ctrl Pts',(2.20678858050854,-1.94784937420141,
19.5627826620234));
#100807=CARTESIAN_POINT('Ctrl Pts',(2.2661638315503,-1.87613045617123,19.5678347226731));
#100808=CARTESIAN_POINT('Ctrl Pts',(2.32545713763209,-1.80451051884032,
19.5728798108738));
#100809=CARTESIAN_POINT('Ctrl Pts',(2.38143769656555,-1.72997332150707,
19.5779248990745));
#100810=CARTESIAN_POINT('Ctrl Pts',(2.43380774867689,-1.65285929300723,
19.5829699872752));
#100811=CARTESIAN_POINT('Ctrl Pts',(2.48612170947426,-1.57582785803192,
19.5880096718986));
#100812=CARTESIAN_POINT('Ctrl Pts',(2.53483260151494,-1.49622544323132,
19.593049356522));
#100813=CARTESIAN_POINT('Ctrl Pts',(2.57968329096128,-1.41442501333057,
19.5980890411454));
#100814=CARTESIAN_POINT('Ctrl Pts',(2.62450161162462,-1.33268361887382,
19.6031250886239));
#100815=CARTESIAN_POINT('Ctrl Pts',(2.66546505407691,-1.24874775078289,
19.6081611361024));
#100816=CARTESIAN_POINT('Ctrl Pts',(2.70236070937266,-1.16301788311225,
19.6131971835808));
#100817=CARTESIAN_POINT('Ctrl Pts',(2.73924292628499,-1.0773192405499,19.6182313967962));
#100818=CARTESIAN_POINT('Ctrl Pts',(2.77206012391477,-0.989828304194625,
19.6232656100117));
#100819=CARTESIAN_POINT('Ctrl Pts',(2.80064658618208,-0.900967646093179,
19.6282998232271));
#100820=CARTESIAN_POINT('Ctrl Pts',(2.82923063544113,-0.812114488797507,
19.6333336115002));
#100821=CARTESIAN_POINT('Ctrl Pts',(2.85358452347601,-0.721892262642336,
19.6383673997732));
#100822=CARTESIAN_POINT('Ctrl Pts',(2.87359205454985,-0.630739806915627,
19.6434011880463));
#100823=CARTESIAN_POINT('Ctrl Pts',(2.89360349512767,-0.539569539851416,
19.6484359599298));
#100824=CARTESIAN_POINT('Ctrl Pts',(2.90926679717675,-0.447469116249552,
19.6534707318133));
#100825=CARTESIAN_POINT('Ctrl Pts',(2.920516874367,-0.354887568868786,19.6585055036967));
#100826=CARTESIAN_POINT('Ctrl Pts',(2.93177931959824,-0.262204239753328,
19.6635458106769));
#100827=CARTESIAN_POINT('Ctrl Pts',(2.93861880151689,-0.169039172781787,
19.668586117657));
#100828=CARTESIAN_POINT('Ctrl Pts',(2.94102216089823,-0.0758462201135838,
19.6736264246372));
#100829=CARTESIAN_POINT('Ctrl Pts',(2.94342699609299,0.0174039588738806,
19.678669826682));
#100830=CARTESIAN_POINT('Ctrl Pts',(2.94139029538589,0.110681613776166,
19.6837132287268));
#100831=CARTESIAN_POINT('Ctrl Pts',(2.93495099493572,0.203535395756719,
19.6887566307717));
#100832=CARTESIAN_POINT('Ctrl Pts',(2.92850125257871,0.296539748524878,
19.6938082111481));
#100833=CARTESIAN_POINT('Ctrl Pts',(2.91763470955827,0.389118415426352,
19.6988597915245));
#100834=CARTESIAN_POINT('Ctrl Pts',(2.9024418341689,0.480827827050681,19.7039113719009));
#100835=CARTESIAN_POINT('Ctrl Pts',(2.89469034284498,0.527618489799412,
19.7064887169035));
#100836=CARTESIAN_POINT('Ctrl Pts',(2.88581348025684,0.574183077988833,
19.7090660619061));
#100837=CARTESIAN_POINT('Ctrl Pts',(2.87582825256554,0.620464230835137,
19.7116434069087));
#100838=CARTESIAN_POINT('Ctrl Pts',(2.85625540692478,0.71118363040637,19.7166954675585));
#100839=CARTESIAN_POINT('Ctrl Pts',(2.83235050049138,0.801138980456197,
19.7217475282084));
#100840=CARTESIAN_POINT('Ctrl Pts',(2.8041876653406,0.889885126042465,19.7267995888582));
#100841=CARTESIAN_POINT('Ctrl Pts',(2.77606369827642,0.978508791315476,
19.7318446770591));
#100842=CARTESIAN_POINT('Ctrl Pts',(2.74369361293433,1.06592614851754,19.7368897652599));
#100843=CARTESIAN_POINT('Ctrl Pts',(2.70720247106711,1.15170255736805,19.7419348534608));
#100844=CARTESIAN_POINT('Ctrl Pts',(2.67075041329496,1.23738709479044,19.7469745380843));
#100845=CARTESIAN_POINT('Ctrl Pts',(2.63018624522835,1.32143377060214,19.7520142227079));
#100846=CARTESIAN_POINT('Ctrl Pts',(2.58568437665739,1.40342449184482,19.7570539073314));
#100847=CARTESIAN_POINT('Ctrl Pts',(2.54121462512511,1.48535604031002,19.76208995481));
#100848=CARTESIAN_POINT('Ctrl Pts',(2.4928130329673,1.56523419406149,19.7671260022886));
#100849=CARTESIAN_POINT('Ctrl Pts',(2.44070107974723,1.64266315455139,19.7721620497672));
#100850=CARTESIAN_POINT('Ctrl Pts',(2.38860810709281,1.72006391334518,19.7771962629827));
#100851=CARTESIAN_POINT('Ctrl Pts',(2.3328077059137,1.79501688282123,19.7822304761983));
#100852=CARTESIAN_POINT('Ctrl Pts',(2.27356548214273,1.86715398358279,19.7872646894138));
#100853=CARTESIAN_POINT('Ctrl Pts',(2.21432825905962,1.93928499518866,19.7922984776871));
#100854=CARTESIAN_POINT('Ctrl Pts',(2.15165007313315,2.00860026741789,19.7973322659603));
#100855=CARTESIAN_POINT('Ctrl Pts',(2.08583701390335,2.07476455325195,19.8023660542335));
#100856=CARTESIAN_POINT('Ctrl Pts',(2.02001109469515,2.14094176769465,19.8074008261171));
#100857=CARTESIAN_POINT('Ctrl Pts',(1.95104939921749,2.20396645822157,19.8124355980007));
#100858=CARTESIAN_POINT('Ctrl Pts',(1.87929425381006,2.2635408340908,19.8174703698843));
#100859=CARTESIAN_POINT('Ctrl Pts',(1.80746022267026,2.32318070447258,19.8225106768646));
#100860=CARTESIAN_POINT('Ctrl Pts',(1.73282695377717,2.37936240426445,19.8275509838449));
#100861=CARTESIAN_POINT('Ctrl Pts',(1.65576893424291,2.43182919556372,19.8325912908251));
#100862=CARTESIAN_POINT('Ctrl Pts',(1.57866359625056,2.48432820476426,19.8376346928701));
#100863=CARTESIAN_POINT('Ctrl Pts',(1.49913092188043,2.53310753196164,19.8426780949151));
#100864=CARTESIAN_POINT('Ctrl Pts',(1.41757149297742,2.57795559742556,19.84772149696));
#100865=CARTESIAN_POINT('Ctrl Pts',(1.33587980809967,2.62287638807519,19.8527730773366));
#100866=CARTESIAN_POINT('Ctrl Pts',(1.25215520600279,2.66385299514138,19.8578246577131));
#100867=CARTESIAN_POINT('Ctrl Pts',(1.16681962209446,2.70072137946426,19.8628762380897));
#100868=CARTESIAN_POINT('Ctrl Pts',(1.12328092247561,2.71953183855939,19.865453583091));
#100869=CARTESIAN_POINT('Ctrl Pts',(1.07932314081581,2.73727368152657,19.8680309280922));
#100870=CARTESIAN_POINT('Ctrl Pts',(1.03500371305417,2.75393015778616,19.8706082730935));
#100871=CARTESIAN_POINT('Ctrl Pts',(0.948129648114924,2.78657985281419,
19.8756603337431));
#100872=CARTESIAN_POINT('Ctrl Pts',(0.859553040888233,2.81517345709628,
19.8807123943928));
#100873=CARTESIAN_POINT('Ctrl Pts',(0.769688317028746,2.83953233731005,
19.8857644550424));
#100874=CARTESIAN_POINT('Ctrl Pts',(0.67994761725451,2.86385759935078,19.8908095432431));
#100875=CARTESIAN_POINT('Ctrl Pts',(0.588922758559964,2.88395963567448,
19.8958546314438));
#100876=CARTESIAN_POINT('Ctrl Pts',(0.497046894193138,2.89970832756899,
19.9008997196445));
#100877=CARTESIAN_POINT('Ctrl Pts',(0.405269434119334,2.91544015171589,
19.9059394042678));
#100878=CARTESIAN_POINT('Ctrl Pts',(0.312643215620222,2.92682782452305,
19.9109790888912));
#100879=CARTESIAN_POINT('Ctrl Pts',(0.219614190971859,2.9337916775265,19.9160187735146));
#100880=CARTESIAN_POINT('Ctrl Pts',(0.126652305454438,2.94075050471097,
19.921054820993));
#100881=CARTESIAN_POINT('Ctrl Pts',(0.033288633389895,2.94329182489224,
19.9260908684714));
#100882=CARTESIAN_POINT('Ctrl Pts',(-0.0600241394538181,2.94138761517125,
19.9311269159499));
#100883=CARTESIAN_POINT('Ctrl Pts',(-0.153302925292624,2.93948409901432,
19.9361611291652));
#100884=CARTESIAN_POINT('Ctrl Pts',(-0.246530404979054,2.93313827867081,
19.9411953423806));
#100885=CARTESIAN_POINT('Ctrl Pts',(-0.339253313795942,2.92237423836826,
19.946229555596));
#100886=CARTESIAN_POINT('Ctrl Pts',(-0.431968395791085,2.91161110666776,
19.9512633438691));
#100887=CARTESIAN_POINT('Ctrl Pts',(-0.524178550279414,2.89643054791783,
19.9562971321421));
#100888=CARTESIAN_POINT('Ctrl Pts',(-0.615436204776654,2.87690845837161,
19.9613309204152));
#100889=CARTESIAN_POINT('Ctrl Pts',(-0.706711691167461,2.85738255417746,
19.9663656922986));
#100890=CARTESIAN_POINT('Ctrl Pts',(-0.797033873563027,2.83351352767994,
19.9714004641821));
#100891=CARTESIAN_POINT('Ctrl Pts',(-0.885967058427973,2.80542801928342,
19.9764352360655));
#100892=CARTESIAN_POINT('Ctrl Pts',(-0.974998014113154,2.77731163441264,
19.9814755430456));
#100893=CARTESIAN_POINT('Ctrl Pts',(-1.06263649979134,2.74496964862536,
19.9865158500257));
#100894=CARTESIAN_POINT('Ctrl Pts',(-1.14846393133775,2.70857796609517,
19.9915561570059));
#100895=CARTESIAN_POINT('Ctrl Pts',(-1.23434406631143,2.67216393678891,
19.9965995590507));
#100896=CARTESIAN_POINT('Ctrl Pts',(-1.31841053314281,2.63169545265336,
20.0016429610955));
#100897=CARTESIAN_POINT('Ctrl Pts',(-1.40026859257394,2.587394803398,20.0066863631403));
#100898=CARTESIAN_POINT('Ctrl Pts',(-1.4822593922362,2.54302231664171,20.0117379435167));
#100899=CARTESIAN_POINT('Ctrl Pts',(-1.56203425538677,2.49480548833797,
20.0167895238931));
#100900=CARTESIAN_POINT('Ctrl Pts',(-1.63922685724251,2.44301029684585,
20.0218411042695));
#100901=CARTESIAN_POINT('Ctrl Pts',(-1.67861096119261,2.4165840959302,20.0244184492724));
#100902=CARTESIAN_POINT('Ctrl Pts',(-1.71732339786238,2.38922707104951,
20.0269957942753));
#100903=CARTESIAN_POINT('Ctrl Pts',(-1.75531899247482,2.36097844857957,
20.0295731392782));
#100904=CARTESIAN_POINT('Ctrl Pts',(-1.82907976954247,2.30613945038183,
20.034576534333));
#100905=CARTESIAN_POINT('Ctrl Pts',(-1.90041320610856,2.24773250319076,
20.0395799293878));
#100906=CARTESIAN_POINT('Ctrl Pts',(-1.96894869439112,2.18600206744081,
20.0445833244426));
#100907=CARTESIAN_POINT('Ctrl Pts',(-2.03738930140254,2.12435709197368,
20.0495797927432));
#100908=CARTESIAN_POINT('Ctrl Pts',(-2.10303931960925,2.05939806735333,
20.0545762610437));
#100909=CARTESIAN_POINT('Ctrl Pts',(-2.16555842516025,1.99141173724006,
20.0595727293443));
#100910=CARTESIAN_POINT('Ctrl Pts',(-2.22800653052416,1.92350261619936,
20.0645635233765));
#100911=CARTESIAN_POINT('Ctrl Pts',(-2.28733048517625,1.8525733552444,20.0695543174087));
#100912=CARTESIAN_POINT('Ctrl Pts',(-2.34322528180016,1.77894892527374,
20.0745451114409));
#100913=CARTESIAN_POINT('Ctrl Pts',(-2.39908531028227,1.70537029177743,
20.0795328010582));
#100914=CARTESIAN_POINT('Ctrl Pts',(-2.45152014164691,1.62910017771565,
20.0845204906756));
#100915=CARTESIAN_POINT('Ctrl Pts',(-2.50026434729797,1.55049740200707,
20.089508180293));
#100916=CARTESIAN_POINT('Ctrl Pts',(-2.54899251987054,1.47192048054014,
20.0944942293457));
#100917=CARTESIAN_POINT('Ctrl Pts',(-2.59403223871125,1.39101280656167,
20.0994802783985));
#100918=CARTESIAN_POINT('Ctrl Pts',(-2.63516153465743,1.30816194955437,
20.1044663274512));
#100919=CARTESIAN_POINT('Ctrl Pts',(-2.67628935711786,1.22531406073689,
20.1094521978753));
#100920=CARTESIAN_POINT('Ctrl Pts',(-2.71350683455284,1.14052353429524,
20.1144380682993));
#100921=CARTESIAN_POINT('Ctrl Pts',(-2.7466386640879,1.05420114254228,20.1194239387234));
#100922=CARTESIAN_POINT('Ctrl Pts',(-2.77979990513923,0.967802121382922,
20.1244142351635));
#100923=CARTESIAN_POINT('Ctrl Pts',(-2.80886809048247,0.879868943068014,
20.1294045316036));
#100924=CARTESIAN_POINT('Ctrl Pts',(-2.83371684144385,0.7908304891173,20.1343948280437));
#100925=CARTESIAN_POINT('Ctrl Pts',(-2.8585763585795,0.701753457633498,
20.1393872866207));
#100926=CARTESIAN_POINT('Ctrl Pts',(-2.87921269939872,0.61157063956846,
20.1443797451977));
#100927=CARTESIAN_POINT('Ctrl Pts',(-2.89555049922398,0.520721908933904,
20.1493722037747));
#100928=CARTESIAN_POINT('Ctrl Pts',(-2.91191514662537,0.429723888417112,
20.154372866358));
#100929=CARTESIAN_POINT('Ctrl Pts',(-2.92396708264555,0.338058219848184,
20.1593735289412));
#100930=CARTESIAN_POINT('Ctrl Pts',(-2.93168279631951,0.246170635462961,
20.1643741915245));
#100931=CARTESIAN_POINT('Ctrl Pts',(-2.93860014417155,0.163790908669531,
20.1688574219864));
#100932=CARTESIAN_POINT('Ctrl Pts',(-2.94203292020321,0.0812330863468883,
20.1733406524484));
#100933=CARTESIAN_POINT('Ctrl Pts',(-2.94199976189605,-0.00118363997366727,
20.1778238829104));
#100934=CARTESIAN_POINT('',(-2.94199876947892,0.00269079626312435,21.1778238829104));
#100935=CARTESIAN_POINT('Ctrl Pts',(-2.94627313971723,-0.00118535926028303,
20.1778238829104));
#100936=CARTESIAN_POINT('Ctrl Pts',(-2.94660879883213,-0.0669346369190534,
20.1813952570946));
#100937=CARTESIAN_POINT('Ctrl Pts',(-2.91478035335495,-1.10787161819102,
20.2379549200069));
#100938=CARTESIAN_POINT('Ctrl Pts',(-1.68204367473694,-3.04506152239431,
20.3475028716478));
#100939=CARTESIAN_POINT('Ctrl Pts',(1.64986237125127,-3.06261730478403,
20.5064677378324));
#100940=CARTESIAN_POINT('Ctrl Pts',(3.46820737751736,-0.270570109276814,
20.6654326040173));
#100941=CARTESIAN_POINT('Ctrl Pts',(2.1048666544717,2.76969438133523,20.8243974702019));
#100942=CARTESIAN_POINT('Ctrl Pts',(-1.18944977837209,3.26907935485098,
20.9833623363867));
#100943=CARTESIAN_POINT('Ctrl Pts',(-2.82218977905123,1.41660932964794,
21.1011711406229));
#100944=CARTESIAN_POINT('Ctrl Pts',(-2.94431188226859,0.221291506348862,
21.1659916561308));
#100945=CARTESIAN_POINT('Ctrl Pts',(-2.94228710142995,0.00269105997585707,
21.1778238829104));
#100946=CARTESIAN_POINT('',(-2.94152579413549,-0.000227484859817469,22.177823899892));
#100947=CARTESIAN_POINT('Ctrl Pts',(-2.94199876947892,0.00269079626312435,
21.1778238829104));
#100948=CARTESIAN_POINT('Ctrl Pts',(-2.94208568955751,-0.092343810318554,
21.182968390654));
#100949=CARTESIAN_POINT('Ctrl Pts',(-2.93756295517028,-0.187514566962741,
21.1881128983975));
#100950=CARTESIAN_POINT('Ctrl Pts',(-2.92842156909576,-0.282331566876175,
21.1932574061411));
#100951=CARTESIAN_POINT('Ctrl Pts',(-2.91959119562788,-0.373922657495653,
21.1982268849831));
#100952=CARTESIAN_POINT('Ctrl Pts',(-2.90645140284425,-0.465183175120309,
21.2031963638252));
#100953=CARTESIAN_POINT('Ctrl Pts',(-2.8890470071336,-0.555672017085965,
21.2081658426672));
#100954=CARTESIAN_POINT('Ctrl Pts',(-2.8716495703139,-0.646124678422679,
21.2131333345364));
#100955=CARTESIAN_POINT('Ctrl Pts',(-2.8499910018557,-0.735805828061689,
21.2181008264056));
#100956=CARTESIAN_POINT('Ctrl Pts',(-2.82416761979265,-0.824282266771967,
21.2230683182748));
#100957=CARTESIAN_POINT('Ctrl Pts',(-2.79834688003636,-0.912749652373244,
21.228035301859));
#100958=CARTESIAN_POINT('Ctrl Pts',(-2.76836230204739,-1.0000121330932,
21.2330022854432));
#100959=CARTESIAN_POINT('Ctrl Pts',(-2.7343603456571,-1.08565072656817,
21.2379692690275));
#100960=CARTESIAN_POINT('Ctrl Pts',(-2.70035175188033,-1.17130603721188,
21.2429372221968));
#100961=CARTESIAN_POINT('Ctrl Pts',(-2.66232439333023,-1.2553364070001,
21.2479051753661));
#100962=CARTESIAN_POINT('Ctrl Pts',(-2.62047271950662,-1.33734315952248,
21.2528731285354));
#100963=CARTESIAN_POINT('Ctrl Pts',(-2.57857604001892,-1.41943809892057,
21.2578464240485));
#100964=CARTESIAN_POINT('Ctrl Pts',(-2.53284704979247,-1.49950467242914,
21.2628197195616));
#100965=CARTESIAN_POINT('Ctrl Pts',(-2.48352571060707,-1.57716963093818,
21.2677930150748));
#100966=CARTESIAN_POINT('Ctrl Pts',(-2.43417250807282,-1.6548847637877,
21.2727695235146));
#100967=CARTESIAN_POINT('Ctrl Pts',(-2.38122260415856,-1.7301948231818,
21.2777460319545));
#100968=CARTESIAN_POINT('Ctrl Pts',(-2.32495739514281,-1.80275819531371,
21.2827225403944));
#100969=CARTESIAN_POINT('Ctrl Pts',(-2.26860603184925,-1.87543267775751,
21.2877066689515));
#100970=CARTESIAN_POINT('Ctrl Pts',(-2.20892953587721,-1.94535173976802,
21.2926907975087));
#100971=CARTESIAN_POINT('Ctrl Pts',(-2.1462469970462,-2.01220968779851,
21.2976749260658));
#100972=CARTESIAN_POINT('Ctrl Pts',(-2.13108341765969,-2.02838334351645,
21.2988806402959));
#100973=CARTESIAN_POINT('Ctrl Pts',(-2.11574407572406,-2.04437804425921,
21.3000863545261));
#100974=CARTESIAN_POINT('Ctrl Pts',(-2.10023377245074,-2.06018982160803,
21.3012920687562));
#100975=CARTESIAN_POINT('Ctrl Pts',(-2.03524408410839,-2.12644271582489,
21.3063441293552));
#100976=CARTESIAN_POINT('Ctrl Pts',(-1.96699957376989,-2.18973644539041,
21.3113961899542));
#100977=CARTESIAN_POINT('Ctrl Pts',(-1.89580061639637,-2.24973421160615,
21.3164482505532));
#100978=CARTESIAN_POINT('Ctrl Pts',(-1.82469992211389,-2.30964917371659,
21.3214933387033));
#100979=CARTESIAN_POINT('Ctrl Pts',(-1.75065322006327,-2.36627692772359,
21.3265384268534));
#100980=CARTESIAN_POINT('Ctrl Pts',(-1.67399833226664,-2.41931675965933,
21.3315835150036));
#100981=CARTESIAN_POINT('Ctrl Pts',(-1.59742554622715,-2.47229978290973,
21.3366231995765));
#100982=CARTESIAN_POINT('Ctrl Pts',(-1.51825049035633,-2.52170227089869,
21.3416628841494));
#100983=CARTESIAN_POINT('Ctrl Pts',(-1.43684387523728,-2.56726385052123,
21.3467025687224));
#100984=CARTESIAN_POINT('Ctrl Pts',(-1.35549601133922,-2.61279254831435,
21.3517386161508));
#100985=CARTESIAN_POINT('Ctrl Pts',(-1.27192017590671,-2.65448563107063,
21.3567746635793));
#100986=CARTESIAN_POINT('Ctrl Pts',(-1.18651497306713,-2.69212670925562,
21.3618107110077));
#100987=CARTESIAN_POINT('Ctrl Pts',(-1.10114087707972,-2.72975407755626,
21.3668449241734));
#100988=CARTESIAN_POINT('Ctrl Pts',(-1.01393914351902,-2.76333219419435,
21.3718791373391));
#100989=CARTESIAN_POINT('Ctrl Pts',(-0.925330884779896,-2.79269166820694,
21.3769133505048));
#100990=CARTESIAN_POINT('Ctrl Pts',(-0.836730105535406,-2.82204866396263,
21.3819471387285));
#100991=CARTESIAN_POINT('Ctrl Pts',(-0.746723458975725,-2.84718758552121,
21.3869809269522));
#100992=CARTESIAN_POINT('Ctrl Pts',(-0.655748755508701,-2.8679884186741,
21.3920147151759));
#100993=CARTESIAN_POINT('Ctrl Pts',(-0.564756275429846,-2.88879331634519,
21.3970494870103));
#100994=CARTESIAN_POINT('Ctrl Pts',(-0.472795795954753,-2.90525834347357,
21.4020842588448));
#100995=CARTESIAN_POINT('Ctrl Pts',(-0.380315765807076,-2.91731450451928,
21.4071190306793));
#100996=CARTESIAN_POINT('Ctrl Pts',(-0.287734065512315,-2.92938391979582,
21.4121593376114));
#100997=CARTESIAN_POINT('Ctrl Pts',(-0.194632115655815,-2.93703473625338,
21.4171996445435));
#100998=CARTESIAN_POINT('Ctrl Pts',(-0.101463636534064,-2.94024984150349,
21.4222399514755));
#100999=CARTESIAN_POINT('Ctrl Pts',(-0.00823794611273068,-2.94346692103021,
21.4272833534727));
#101000=CARTESIAN_POINT('Ctrl Pts',(0.0850539109652886,-2.94224287261987,
21.4323267554699));
#101001=CARTESIAN_POINT('Ctrl Pts',(0.177960263810673,-2.93661269909814,
21.4373701574671));
#101002=CARTESIAN_POINT('Ctrl Pts',(0.271017272714683,-2.93097339574054,
21.4424217377971));
#101003=CARTESIAN_POINT('Ctrl Pts',(0.363687088218949,-2.92091375109494,
21.447473318127));
#101004=CARTESIAN_POINT('Ctrl Pts',(0.455525369650964,-2.90652036593662,
21.4525248984569));
#101005=CARTESIAN_POINT('Ctrl Pts',(0.502381791884863,-2.89917677760028,
21.4551022439516));
#101006=CARTESIAN_POINT('Ctrl Pts',(0.549021951560869,-2.89070589085695,
21.4576795894463));
#101007=CARTESIAN_POINT('Ctrl Pts',(0.595388341891801,-2.88112421154301,
21.460256934941));
#101008=CARTESIAN_POINT('Ctrl Pts',(0.686274804721182,-2.86234239707365,
21.4653089955786));
#101009=CARTESIAN_POINT('Ctrl Pts',(0.776434985139052,-2.8392220303162,
21.4703610562162));
#101010=CARTESIAN_POINT('Ctrl Pts',(0.865423099306033,-2.81183336262794,
21.4754131168539));
#101011=CARTESIAN_POINT('Ctrl Pts',(0.95428839920448,-2.78448249458539,
21.480458205042));
#101012=CARTESIAN_POINT('Ctrl Pts',(1.04198442625007,-2.75287516083567,
21.4855032932302));
#101013=CARTESIAN_POINT('Ctrl Pts',(1.12807546719918,-2.71713263207804,
21.4905483814183));
#101014=CARTESIAN_POINT('Ctrl Pts',(1.21407429972261,-2.6814283856117,21.4955880660287));
#101015=CARTESIAN_POINT('Ctrl Pts',(1.29847115483984,-2.64159791691911,
21.500627750639));
#101016=CARTESIAN_POINT('Ctrl Pts',(1.38084643611309,-2.59781198701403,
21.5056674352493));
#101017=CARTESIAN_POINT('Ctrl Pts',(1.46316226706027,-2.55405765746004,
21.510703482714));
#101018=CARTESIAN_POINT('Ctrl Pts',(1.54345903287469,-2.50635374865088,
21.5157395301788));
#101019=CARTESIAN_POINT('Ctrl Pts',(1.62133902064147,-2.454918283802,21.5207755776435));
#101020=CARTESIAN_POINT('Ctrl Pts',(1.69919064242934,-2.40350155312802,
21.5258097908447));
#101021=CARTESIAN_POINT('Ctrl Pts',(1.77462686451415,-2.34835621107149,
21.530844004046));
#101022=CARTESIAN_POINT('Ctrl Pts',(1.84727730767968,-2.28974464701454,
21.5358782172472));
#101023=CARTESIAN_POINT('Ctrl Pts',(1.9199216183521,-2.23113803041553,21.5409120055057));
#101024=CARTESIAN_POINT('Ctrl Pts',(1.98978027194905,-2.16906605265924,
21.5459457937642));
#101025=CARTESIAN_POINT('Ctrl Pts',(2.05651536771951,-2.10383187121345,
21.5509795820228));
#101026=CARTESIAN_POINT('Ctrl Pts',(2.12326350363077,-2.03858494290784,
21.5560143538913));
#101027=CARTESIAN_POINT('Ctrl Pts',(2.18688655211979,-1.97017489458745,
21.5610491257598));
#101028=CARTESIAN_POINT('Ctrl Pts',(2.24708375161924,-1.89894144543975,
21.5660838976283));
#101029=CARTESIAN_POINT('Ctrl Pts',(2.30734713034196,-1.82762968410519,
21.5711242045931));
#101030=CARTESIAN_POINT('Ctrl Pts',(2.36417685486138,-1.75348866590415,
21.5761645115578));
#101031=CARTESIAN_POINT('Ctrl Pts',(2.41731293472768,-1.67689062720209,
21.5812048185226));
#101032=CARTESIAN_POINT('Ctrl Pts',(2.47048164347745,-1.60024555250332,
21.5862482205517));
#101033=CARTESIAN_POINT('Ctrl Pts',(2.51995195677038,-1.52114083008159,
21.5912916225808));
#101034=CARTESIAN_POINT('Ctrl Pts',(2.56550881329504,-1.43997518343389,
21.5963350246099));
#101035=CARTESIAN_POINT('Ctrl Pts',(2.61113954437165,-1.35867791936926,
21.6013866049704));
#101036=CARTESIAN_POINT('Ctrl Pts',(2.65284395100615,-1.27531345605971,
21.6064381853308));
#101037=CARTESIAN_POINT('Ctrl Pts',(2.69045432463521,-1.19030228389755,
21.6114897656912));
#101038=CARTESIAN_POINT('Ctrl Pts',(2.70964335201929,-1.14692909843915,
21.6140671108361));
#101039=CARTESIAN_POINT('Ctrl Pts',(2.72776745447538,-1.10312753770133,
21.6166444559809));
#101040=CARTESIAN_POINT('Ctrl Pts',(2.74480938171181,-1.05895488953347,
21.6192218011258));
#101041=CARTESIAN_POINT('Ctrl Pts',(2.77821462964113,-0.972368540274324,
21.6242738619854));
#101042=CARTESIAN_POINT('Ctrl Pts',(2.80757877179907,-0.884044379248353,
21.629325922845));
#101043=CARTESIAN_POINT('Ctrl Pts',(2.83271957144272,-0.79439526028633,
21.6343779837046));
#101044=CARTESIAN_POINT('Ctrl Pts',(2.85782567377613,-0.704869867830115,
21.639423072116));
#101045=CARTESIAN_POINT('Ctrl Pts',(2.87871989703247,-0.614023575165785,
21.6444681605274));
#101046=CARTESIAN_POINT('Ctrl Pts',(2.89526835409674,-0.522288385631872,
21.6495132489388));
#101047=CARTESIAN_POINT('Ctrl Pts',(2.91179908682151,-0.430651449707756,
21.6545529337733));
#101048=CARTESIAN_POINT('Ctrl Pts',(2.92399322651787,-0.338127944159667,
21.6595926186079));
#101049=CARTESIAN_POINT('Ctrl Pts',(2.9317672229085,-0.245163110355933,
21.6646323034424));
#101050=CARTESIAN_POINT('Ctrl Pts',(2.9395356087989,-0.152265369356827,
21.6696683511319));
#101051=CARTESIAN_POINT('Ctrl Pts',(2.94289015506298,-0.0589273746584211,
21.6747043988213));
#101052=CARTESIAN_POINT('Ctrl Pts',(2.94179889637111,0.0343984492339381,
21.6797404465107));
#101053=CARTESIAN_POINT('Ctrl Pts',(2.94070803514484,0.127690281365921,
21.684774659937));
#101054=CARTESIAN_POINT('Ctrl Pts',(2.93517459101143,0.220969507675514,
21.6898088733632));
#101055=CARTESIAN_POINT('Ctrl Pts',(2.92521869874725,0.31378267080806,21.6948430867894));
#101056=CARTESIAN_POINT('Ctrl Pts',(2.91526364686947,0.406587999492738,
21.6998768752729));
#101057=CARTESIAN_POINT('Ctrl Pts',(2.90088693663444,0.498926901469453,
21.7049106637563));
#101058=CARTESIAN_POINT('Ctrl Pts',(2.88216056246513,0.590351160048563,
21.7099444522398));
#101059=CARTESIAN_POINT('Ctrl Pts',(2.86343052913474,0.681793283062371,
21.7149792243329));
#101060=CARTESIAN_POINT('Ctrl Pts',(2.84034923342057,0.772319972569361,
21.720013996426));
#101061=CARTESIAN_POINT('Ctrl Pts',(2.81303951545293,0.861494448328216,
21.7250487685191));
#101062=CARTESIAN_POINT('Ctrl Pts',(2.7856997739086,0.950766960131055,21.7300890757066));
#101063=CARTESIAN_POINT('Ctrl Pts',(2.75412246119298,1.03868386528113,21.7351293828941));
#101064=CARTESIAN_POINT('Ctrl Pts',(2.71847982838235,1.12482506314461,21.7401696900816));
#101065=CARTESIAN_POINT('Ctrl Pts',(2.68281530876714,1.21101915708829,21.7452130923328));
#101066=CARTESIAN_POINT('Ctrl Pts',(2.64308068838097,1.29543497128397,21.750256494584));
#101067=CARTESIAN_POINT('Ctrl Pts',(2.59949480979731,1.37767584497837,21.7552998968352));
#101068=CARTESIAN_POINT('Ctrl Pts',(2.55583825281186,1.46005007960762,21.7603514774143));
#101069=CARTESIAN_POINT('Ctrl Pts',(2.50831819607966,1.54024195098564,21.7654030579935));
#101070=CARTESIAN_POINT('Ctrl Pts',(2.4571974166949,1.61788283116792,21.7704546385727));
#101071=CARTESIAN_POINT('Ctrl Pts',(2.43111532686805,1.65749561554877,21.7730319814852));
#101072=CARTESIAN_POINT('Ctrl Pts',(2.40409659879385,1.69644486793155,21.7756093243978));
#101073=CARTESIAN_POINT('Ctrl Pts',(2.37618006372778,1.73468507364958,21.7781866673104));
#101074=CARTESIAN_POINT('Ctrl Pts',(2.32145858420865,1.80964282284925,21.7832387275705));
#101075=CARTESIAN_POINT('Ctrl Pts',(2.26308843126375,1.88214339907823,21.7882907878305));
#101076=CARTESIAN_POINT('Ctrl Pts',(2.20131809666195,1.9518100925317,21.7933428480905));
#101077=CARTESIAN_POINT('Ctrl Pts',(2.13963301252477,2.021380637599,21.7983879359019));
#101078=CARTESIAN_POINT('Ctrl Pts',(2.07455736380772,2.08812474215966,21.8034330237133));
#101079=CARTESIAN_POINT('Ctrl Pts',(2.00638191565684,2.15169598422388,21.8084781115247));
#101080=CARTESIAN_POINT('Ctrl Pts',(1.93827948729521,2.21519913786591,21.8135177957597));
#101081=CARTESIAN_POINT('Ctrl Pts',(1.86708418180217,2.27553588228219,21.8185574799946));
#101082=CARTESIAN_POINT('Ctrl Pts',(1.79312514287188,2.3323949541192,21.8235971642295));
#101083=CARTESIAN_POINT('Ctrl Pts',(1.71921948020912,2.38921299074167,21.8286332113223));
#101084=CARTESIAN_POINT('Ctrl Pts',(1.64255439984473,2.44255807340714,21.8336692584152));
#101085=CARTESIAN_POINT('Ctrl Pts',(1.56349300852536,2.49215842439687,21.838705305508));
#101086=CARTESIAN_POINT('Ctrl Pts',(1.48446041344956,2.54174070963082,21.8437395183396));
#101087=CARTESIAN_POINT('Ctrl Pts',(1.40303361730671,2.58758073688774,21.8487737311713));
#101088=CARTESIAN_POINT('Ctrl Pts',(1.31960479743701,2.62944997643637,21.853807944003));
#101089=CARTESIAN_POINT('Ctrl Pts',(1.23618301982847,2.67131568178519,21.8588417318947));
#101090=CARTESIAN_POINT('Ctrl Pts',(1.15075995166674,2.70921106670083,21.8638755197864));
#101091=CARTESIAN_POINT('Ctrl Pts',(1.06375143579366,2.74295404315255,21.868909307678));
#101092=CARTESIAN_POINT('Ctrl Pts',(0.976725918265993,2.77670361305579,
21.8739440791829));
#101093=CARTESIAN_POINT('Ctrl Pts',(0.888114752116835,2.80629900278147,
21.8789788506878));
#101094=CARTESIAN_POINT('Ctrl Pts',(0.798351687265794,2.83160706727467,
21.8840136221926));
#101095=CARTESIAN_POINT('Ctrl Pts',(0.708489939122239,2.85694295482778,
21.8890539288007));
#101096=CARTESIAN_POINT('Ctrl Pts',(0.617474192739987,2.87798198789189,
21.8940942354088));
#101097=CARTESIAN_POINT('Ctrl Pts',(0.525750919889955,2.89464159616262,
21.8991345420169));
#101098=CARTESIAN_POINT('Ctrl Pts',(0.43397132313475,2.91131143448911,21.9041779436928));
#101099=CARTESIAN_POINT('Ctrl Pts',(0.341483775087955,2.92359643581221,
21.9092213453687));
#101100=CARTESIAN_POINT('Ctrl Pts',(0.248740258974479,2.9314658932973,21.9142647470446));
#101101=CARTESIAN_POINT('Ctrl Pts',(0.155846350712511,2.93934811183208,
21.9193163270606));
#101102=CARTESIAN_POINT('Ctrl Pts',(0.0626960891820613,2.94280047552177,
21.9243679070766));
#101103=CARTESIAN_POINT('Ctrl Pts',(-0.0302583310267743,2.94184439313222,
21.9294194870926));
#101104=CARTESIAN_POINT('Ctrl Pts',(-0.0776842775038254,2.94135659371254,
21.9319968358935));
#101105=CARTESIAN_POINT('Ctrl Pts',(-0.125059318147335,2.93972206567021,
21.9345741846944));
#101106=CARTESIAN_POINT('Ctrl Pts',(-0.17232416304451,2.9369488219632,21.9371515334952));
#101107=CARTESIAN_POINT('Ctrl Pts',(-0.264971640504095,2.93151277251895,
21.9422035941855));
#101108=CARTESIAN_POINT('Ctrl Pts',(-0.357528117153358,2.92167874159305,
21.9472556548757));
#101109=CARTESIAN_POINT('Ctrl Pts',(-0.449542335570193,2.90745175171147,
21.952307715566));
#101110=CARTESIAN_POINT('Ctrl Pts',(-0.54142956327939,2.89324439679005,
21.9573528038038));
#101111=CARTESIAN_POINT('Ctrl Pts',(-0.63277558461395,2.87465619775139,
21.9623978920416));
#101112=CARTESIAN_POINT('Ctrl Pts',(-0.723131726038894,2.8517441166409,
21.9674429802794));
#101113=CARTESIAN_POINT('Ctrl Pts',(-0.813391090819521,2.82885657569215,
21.9724826649364));
#101114=CARTESIAN_POINT('Ctrl Pts',(-0.902662254674683,2.80165446632487,
21.9775223495934));
#101115=CARTESIAN_POINT('Ctrl Pts',(-0.990505331762105,2.77024605184284,
21.9825620342505));
#101116=CARTESIAN_POINT('Ctrl Pts',(-1.07828501233058,2.7388603048744,21.9875980817573));
#101117=CARTESIAN_POINT('Ctrl Pts',(-1.16463823753488,2.70327443580654,
21.9926341292641));
#101118=CARTESIAN_POINT('Ctrl Pts',(-1.24913993761244,2.6636466387758,21.997670176771));
#101119=CARTESIAN_POINT('Ctrl Pts',(-1.33361085985892,2.62403327527292,
22.0027043900115));
#101120=CARTESIAN_POINT('Ctrl Pts',(-1.41623119483375,2.58038109689235,
22.0077386032521));
#101121=CARTESIAN_POINT('Ctrl Pts',(-1.49659650065452,2.53289615148917,
22.0127728164926));
#101122=CARTESIAN_POINT('Ctrl Pts',(-1.57695502271736,2.48541521436259,
22.0178066047875));
#101123=CARTESIAN_POINT('Ctrl Pts',(-1.65505851165594,2.43410237963196,
22.0228403930825));
#101124=CARTESIAN_POINT('Ctrl Pts',(-1.73052876463478,2.37920873291345,
22.0278741813774));
#101125=CARTESIAN_POINT('Ctrl Pts',(-1.80601376457456,2.3243043599229,22.0329089532795));
#101126=CARTESIAN_POINT('Ctrl Pts',(-1.8788641476136,2.26581804698184,22.0379437251816));
#101127=CARTESIAN_POINT('Ctrl Pts',(-1.94873317017218,2.20404242959856,
22.0429784970836));
#101128=CARTESIAN_POINT('Ctrl Pts',(-2.01867900483887,2.14219889777726,
22.0480188040774));
#101129=CARTESIAN_POINT('Ctrl Pts',(-2.0856366030939,2.07705913793298,22.0530591110711));
#101130=CARTESIAN_POINT('Ctrl Pts',(-2.14929485944968,2.00895385888854,
22.0580994180648));
#101131=CARTESIAN_POINT('Ctrl Pts',(-2.21299220593247,1.9408067589687,22.0631428201204));
#101132=CARTESIAN_POINT('Ctrl Pts',(-2.27338588976149,1.86969085298636,
22.068186222176));
#101133=CARTESIAN_POINT('Ctrl Pts',(-2.33020543016506,1.79596955799069,
22.0732296242315));
#101134=CARTESIAN_POINT('Ctrl Pts',(-2.38711710853098,1.72212871732719,
22.0782812046142));
#101135=CARTESIAN_POINT('Ctrl Pts',(-2.44044281894712,1.64567441712911,
22.083332784997));
#101136=CARTESIAN_POINT('Ctrl Pts',(-2.48995578633093,1.56699846270414,
22.0883843653797));
#101137=CARTESIAN_POINT('Ctrl Pts',(-2.51521758119624,1.52685754757558,
22.0909617101464));
#101138=CARTESIAN_POINT('Ctrl Pts',(-2.53948762525191,1.48613870506356,
22.0935390549132));
#101139=CARTESIAN_POINT('Ctrl Pts',(-2.56274056206897,1.44489612482227,
22.0961163996799));
#101140=CARTESIAN_POINT('Ctrl Pts',(-2.6103764335966,1.36040674314553,22.1013963376576));
#101141=CARTESIAN_POINT('Ctrl Pts',(-2.65389921416439,1.27343736533958,
22.1066762756352));
#101142=CARTESIAN_POINT('Ctrl Pts',(-2.69305519158291,1.18440606849522,
22.1119562136129));
#101143=CARTESIAN_POINT('Ctrl Pts',(-2.73376136689767,1.09184999361783,
22.1174451860543));
#101144=CARTESIAN_POINT('Ctrl Pts',(-2.76974753991899,0.997065665326674,
22.1229341584958));
#101145=CARTESIAN_POINT('Ctrl Pts',(-2.8007794475078,0.900554543832798,
22.1284231309372));
#101146=CARTESIAN_POINT('Ctrl Pts',(-2.83050512030054,0.808105892064405,
22.1336810545211));
#101147=CARTESIAN_POINT('Ctrl Pts',(-2.85568497940642,0.714073287878334,
22.1389389781049));
#101148=CARTESIAN_POINT('Ctrl Pts',(-2.87616093144695,0.618920266608081,
22.1441969016888));
#101149=CARTESIAN_POINT('Ctrl Pts',(-2.8966088623409,0.52389746134687,22.149447629854));
#101150=CARTESIAN_POINT('Ctrl Pts',(-2.91236561448378,0.427757666820328,
22.1546983580192));
#101151=CARTESIAN_POINT('Ctrl Pts',(-2.92332287558182,0.330979402833541,
22.1599490861844));
#101152=CARTESIAN_POINT('Ctrl Pts',(-2.93426307423731,0.234351840153816,
22.1651916380136));
#101153=CARTESIAN_POINT('Ctrl Pts',(-2.94041862569877,0.137088172150242,
22.1704341898429));
#101154=CARTESIAN_POINT('Ctrl Pts',(-2.94173245156721,0.0396759800933485,
22.1756767416722));
#101155=CARTESIAN_POINT('Ctrl Pts',(-2.9419118152177,0.0263772570361183,
22.1763924554182));
#101156=CARTESIAN_POINT('Ctrl Pts',(-2.94200101859664,0.0130757779320145,
22.1771081691643));
#101157=CARTESIAN_POINT('Ctrl Pts',(-2.94199999122659,-0.000227206362431655,
22.1778238829104));
#101158=CARTESIAN_POINT('',(-2.94312392831984,-0.00259505423936747,23.1778238829104));
#101159=CARTESIAN_POINT('Ctrl Pts',(-2.9371647108909,-0.000230046137197137,
22.1778240560681));
#101160=CARTESIAN_POINT('Ctrl Pts',(-2.93749219107628,-0.478103761682066,
22.2035764593337));
#101161=CARTESIAN_POINT('Ctrl Pts',(-2.6012367037522,-1.93881763980532,
22.2823171513272));
#101162=CARTESIAN_POINT('Ctrl Pts',(-0.300772375801865,-3.46571890274164,
22.4140461320495));
#101163=CARTESIAN_POINT('Ctrl Pts',(2.75125260656092,-2.12891426657218,
22.5730109982341));
#101164=CARTESIAN_POINT('Ctrl Pts',(3.279317883015,1.16092598313884,22.731975864419));
#101165=CARTESIAN_POINT('Ctrl Pts',(0.798979033620407,3.38575070070742,
22.8909407306036));
#101166=CARTESIAN_POINT('Ctrl Pts',(-2.20513524174184,2.56189931173273,
23.0395567367676));
#101167=CARTESIAN_POINT('Ctrl Pts',(-2.93587608380215,0.784594837198067,
23.1351844542031));
#101168=CARTESIAN_POINT('Ctrl Pts',(-2.94312392831984,-0.00259505423936747,
23.1778238829104));
#101169=CARTESIAN_POINT('',(-2.14321747322427,2.01117680924495,24.058));
#101170=CARTESIAN_POINT('Ctrl Pts',(-2.94312392831984,-0.00259505423936747,
23.1778238829104));
#101171=CARTESIAN_POINT('Ctrl Pts',(-2.94488302619335,-0.193651037946246,
23.1881727429313));
#101172=CARTESIAN_POINT('Ctrl Pts',(-2.84079414435847,-1.36104498058977,
23.2515098916811));
#101173=CARTESIAN_POINT('Ctrl Pts',(-1.28036762178996,-3.23455542907612,
23.3678353291575));
#101174=CARTESIAN_POINT('Ctrl Pts',(2.02658934189923,-2.82744350159193,
23.5268001953429));
#101175=CARTESIAN_POINT('Ctrl Pts',(3.47445766960654,0.173475693601123,
23.6857650615274));
#101176=CARTESIAN_POINT('Ctrl Pts',(1.73476021572655,3.01534707573969,23.8447299277121));
#101177=CARTESIAN_POINT('Ctrl Pts',(-0.865109513097841,3.07423831390616,
23.9688082405364));
#101178=CARTESIAN_POINT('Ctrl Pts',(-1.91559325183167,2.25747821289124,
24.0398982646323));
#101179=CARTESIAN_POINT('Ctrl Pts',(-2.14321747322427,2.01117680924495,
24.058));
#101180=CARTESIAN_POINT('',(0.261321691565681,2.93037113238532,24.0579967072125));
#101181=CARTESIAN_POINT('Origin',(0.,0.,24.058));
#101182=CARTESIAN_POINT('',(-2.94199917298087,-0.00220594195414625,23.3221761170896));
#101183=CARTESIAN_POINT('Ctrl Pts',(0.261321691565681,2.93037113238532,
24.0579967072125));
#101184=CARTESIAN_POINT('Ctrl Pts',(0.359057733722356,2.92165532585111,
24.0527226020593));
#101185=CARTESIAN_POINT('Ctrl Pts',(0.456247631980505,2.90805537680646,
24.0474484969061));
#101186=CARTESIAN_POINT('Ctrl Pts',(0.552404207582251,2.88967361330747,
24.0421743917529));
#101187=CARTESIAN_POINT('Ctrl Pts',(0.648847947472514,2.87123695407197,
24.0368845358865));
#101188=CARTESIAN_POINT('Ctrl Pts',(0.744251823606086,2.84798999998556,
24.03159468002));
#101189=CARTESIAN_POINT('Ctrl Pts',(0.838140963850976,2.82008576548923,
24.0263048241535));
#101190=CARTESIAN_POINT('Ctrl Pts',(0.932174041408198,2.79213875223801,
24.0210068586416));
#101191=CARTESIAN_POINT('Ctrl Pts',(1.02468739675793,2.75952034278332,24.0157088931297));
#101192=CARTESIAN_POINT('Ctrl Pts',(1.1152259313767,2.72243183973171,24.0104109276178));
#101193=CARTESIAN_POINT('Ctrl Pts',(1.20603083901619,2.68523421875994,24.0050973749851));
#101194=CARTESIAN_POINT('Ctrl Pts',(1.29484896517312,2.6435403648311,23.9997838223524));
#101195=CARTESIAN_POINT('Ctrl Pts',(1.3812482474766,2.5975983675008,23.9944702697197));
#101196=CARTESIAN_POINT('Ctrl Pts',(1.4529996823673,2.55944522383677,23.9900575591555));
#101197=CARTESIAN_POINT('Ctrl Pts',(1.52308332424415,2.51836314368226,23.9856448485912));
#101198=CARTESIAN_POINT('Ctrl Pts',(1.591268138782,2.47451605581723,23.981232138027));
#101199=CARTESIAN_POINT('Ctrl Pts',(1.66945284296764,2.42423841529911,23.9761722654958));
#101200=CARTESIAN_POINT('Ctrl Pts',(1.7453902427937,2.37016300472242,23.9711123929647));
#101201=CARTESIAN_POINT('Ctrl Pts',(1.81868893726781,2.31251692955093,23.9660525204335));
#101202=CARTESIAN_POINT('Ctrl Pts',(1.89188680650336,2.25495014882422,23.9609996079561));
#101203=CARTESIAN_POINT('Ctrl Pts',(1.96245283852198,2.19382273562446,23.9559466954787));
#101204=CARTESIAN_POINT('Ctrl Pts',(2.03002345584912,2.12940573134911,23.9508937830013));
#101205=CARTESIAN_POINT('Ctrl Pts',(2.09752182464432,2.06505760366796,23.9458462732496));
#101206=CARTESIAN_POINT('Ctrl Pts',(2.16203082654755,1.99742718056391,23.9407987634979));
#101207=CARTESIAN_POINT('Ctrl Pts',(2.2232197764767,1.92682584202176,23.9357512537462));
#101208=CARTESIAN_POINT('Ctrl Pts',(2.28436421696083,1.85627585958885,23.9307074156028));
#101209=CARTESIAN_POINT('Ctrl Pts',(2.34219311717723,1.78275959127877,23.9256635774594));
#101210=CARTESIAN_POINT('Ctrl Pts',(2.39641324748676,1.7066246064293,23.920619739316));
#101211=CARTESIAN_POINT('Ctrl Pts',(2.4506133994977,1.63051767476695,23.9155777596577));
#101212=CARTESIAN_POINT('Ctrl Pts',(2.5012071669494,1.55179430389707,23.9105357799994));
#101213=CARTESIAN_POINT('Ctrl Pts',(2.54794279767852,1.47083360709435,23.9054938003411));
#101214=CARTESIAN_POINT('Ctrl Pts',(2.59467416993196,1.3898802873004,23.9004522800999));
#101215=CARTESIAN_POINT('Ctrl Pts',(2.63754788331948,1.30669043042103,23.8954107598587));
#101216=CARTESIAN_POINT('Ctrl Pts',(2.67635715586578,1.22166950287139,23.8903692396175));
#101217=CARTESIAN_POINT('Ctrl Pts',(2.71517365562128,1.13663274240374,23.8853267805253));
#101218=CARTESIAN_POINT('Ctrl Pts',(2.74992402779534,1.04976463689369,23.8802843214332));
#101219=CARTESIAN_POINT('Ctrl Pts',(2.78044928756233,0.961491424451683,
23.8752418623411));
#101220=CARTESIAN_POINT('Ctrl Pts',(2.81100731255043,0.873123461257484,
23.8701939907713));
#101221=CARTESIAN_POINT('Ctrl Pts',(2.83733102728764,0.783347799512513,
23.8651461192015));
#101222=CARTESIAN_POINT('Ctrl Pts',(2.85931117778128,0.692606373501589,
23.8600982476317));
#101223=CARTESIAN_POINT('Ctrl Pts',(2.88130456619673,0.601810296913911,
23.8550473358948));
#101224=CARTESIAN_POINT('Ctrl Pts',(2.8989490981255,0.510047732412025,23.849996424158));
#101225=CARTESIAN_POINT('Ctrl Pts',(2.91218695661328,0.417769230235415,
23.8449455124211));
#101226=CARTESIAN_POINT('Ctrl Pts',(2.92544578927689,0.325344521213357,
23.8398865979767));
#101227=CARTESIAN_POINT('Ctrl Pts',(2.93428396748588,0.232402682732934,
23.8348276835322));
#101228=CARTESIAN_POINT('Ctrl Pts',(2.93869568164846,0.139397599192756,
23.8297687690878));
#101229=CARTESIAN_POINT('Ctrl Pts',(2.94085508511951,0.0938743642728768,
23.8272925802395));
#101230=CARTESIAN_POINT('Ctrl Pts',(2.94195478478335,0.0483359531580007,
23.8248163913912));
#101231=CARTESIAN_POINT('Ctrl Pts',(2.94199863385711,0.00283520421246993,
23.822340202543));
#101232=CARTESIAN_POINT('Ctrl Pts',(2.94208825862301,-0.0901654825415715,
23.8172790273149));
#101233=CARTESIAN_POINT('Ctrl Pts',(2.93776390565251,-0.18333064952558,
23.8122178520868));
#101234=CARTESIAN_POINT('Ctrl Pts',(2.92900549655993,-0.276207894749105,
23.8071566768588));
#101235=CARTESIAN_POINT('Ctrl Pts',(2.92025884316683,-0.368960478407758,
23.8021022948342));
#101236=CARTESIAN_POINT('Ctrl Pts',(2.90709000256503,-0.46142547144831,
23.7970479128096));
#101237=CARTESIAN_POINT('Ctrl Pts',(2.88953090489682,-0.553150205320539,
23.791993530785));
#101238=CARTESIAN_POINT('Ctrl Pts',(2.87199000635214,-0.644779871109348,
23.7869443873737));
#101239=CARTESIAN_POINT('Ctrl Pts',(2.85006797892551,-0.735670370570118,
23.7818952439624));
#101240=CARTESIAN_POINT('Ctrl Pts',(2.82384846507248,-0.825374973153284,
23.7768461005511));
#101241=CARTESIAN_POINT('Ctrl Pts',(2.79764677704639,-0.915018588384454,
23.7718003898944));
#101242=CARTESIAN_POINT('Ctrl Pts',(2.76715353378432,-1.0034774857748,23.7667546792377));
#101243=CARTESIAN_POINT('Ctrl Pts',(2.73250306386018,-1.09031692915167,
23.761708968581));
#101244=CARTESIAN_POINT('Ctrl Pts',(2.69786434134265,-1.17712693170844,
23.7566649685509));
#101245=CARTESIAN_POINT('Ctrl Pts',(2.6590713562346,-1.26231816054592,23.7516209685208));
#101246=CARTESIAN_POINT('Ctrl Pts',(2.61630737697131,-1.3454737861458,23.7465769684907));
#101247=CARTESIAN_POINT('Ctrl Pts',(2.57354605543116,-1.42862424373665,
23.7415332819383));
#101248=CARTESIAN_POINT('Ctrl Pts',(2.52681443305615,-1.50973895632797,
23.7364895953859));
#101249=CARTESIAN_POINT('Ctrl Pts',(2.47634223213565,-1.58842473833085,
23.7314459088336));
#101250=CARTESIAN_POINT('Ctrl Pts',(2.4258591936746,-1.66712741597801,23.7264011392859));
#101251=CARTESIAN_POINT('Ctrl Pts',(2.37163422037517,-1.74339975488208,
23.7213563697382));
#101252=CARTESIAN_POINT('Ctrl Pts',(2.31394031524762,-1.81687760112555,
23.7163116001905));
#101253=CARTESIAN_POINT('Ctrl Pts',(2.25618215362255,-1.89043728320652,
23.7112612120385));
#101254=CARTESIAN_POINT('Ctrl Pts',(2.19494762177065,-1.96119591149916,
23.7062108238865));
#101255=CARTESIAN_POINT('Ctrl Pts',(2.13054978681914,-2.02882271425694,
23.7011604357345));
#101256=CARTESIAN_POINT('Ctrl Pts',(2.06611164201707,-2.09649184803898,
23.6961068862901));
#101257=CARTESIAN_POINT('Ctrl Pts',(1.99850657162384,-2.16102494801463,
23.6910533368456));
#101258=CARTESIAN_POINT('Ctrl Pts',(1.92808265482739,-2.22212989632779,
23.6859997874012));
#101259=CARTESIAN_POINT('Ctrl Pts',(1.85754493690038,-2.28333358683703,
23.680938071702));
#101260=CARTESIAN_POINT('Ctrl Pts',(1.78417962593036,-2.34109779290347,
23.6758763560029));
#101261=CARTESIAN_POINT('Ctrl Pts',(1.70836568544675,-2.39517237057964,
23.6708146403037));
#101262=CARTESIAN_POINT('Ctrl Pts',(1.67158805140991,-2.42140415612968,
23.6683591825556));
#101263=CARTESIAN_POINT('Ctrl Pts',(1.63423459445879,-2.44676835059095,
23.6659037248074));
#101264=CARTESIAN_POINT('Ctrl Pts',(1.59635063320942,-2.4712403071842,23.6634482670592));
#101265=CARTESIAN_POINT('Ctrl Pts',(1.51850564244454,-2.52152594712721,
23.6584027259007));
#101266=CARTESIAN_POINT('Ctrl Pts',(1.43813897262431,-2.56822233179505,
23.6533571847421));
#101267=CARTESIAN_POINT('Ctrl Pts',(1.35561614290803,-2.61106661598037,
23.6483116435836));
#101268=CARTESIAN_POINT('Ctrl Pts',(1.27320874086602,-2.65385097231182,
23.6432731598064));
#101269=CARTESIAN_POINT('Ctrl Pts',(1.18865156332485,-2.69279373056832,
23.6382346760293));
#101270=CARTESIAN_POINT('Ctrl Pts',(1.10233885300424,-2.72767539365616,
23.6331961922521));
#101271=CARTESIAN_POINT('Ctrl Pts',(1.01612000238436,-2.76251912510628,
23.6281631875125));
#101272=CARTESIAN_POINT('Ctrl Pts',(0.928149824009637,-2.79331037246852,
23.6231301827729));
#101273=CARTESIAN_POINT('Ctrl Pts',(0.838845895604781,-2.81987616100903,
23.6180971780333));
#101274=CARTESIAN_POINT('Ctrl Pts',(0.749608033340722,-2.84642229644852,
23.6130678966595));
#101275=CARTESIAN_POINT('Ctrl Pts',(0.659038807994886,-2.86874905938527,
23.6080386152858));
#101276=CARTESIAN_POINT('Ctrl Pts',(0.567573443485155,-2.88673247569816,
23.6030093339121));
#101277=CARTESIAN_POINT('Ctrl Pts',(0.47614235849875,-2.90470915215993,
23.5979819374198));
#101278=CARTESIAN_POINT('Ctrl Pts',(0.383816238285809,-2.91834562964665,
23.5929545409275));
#101279=CARTESIAN_POINT('Ctrl Pts',(0.291042030199817,-2.9275687074187,
23.5879271444352));
#101280=CARTESIAN_POINT('Ctrl Pts',(0.198276447765538,-2.93679092767809,
23.5829002153634));
#101281=CARTESIAN_POINT('Ctrl Pts',(0.105063303727384,-2.94160052004931,
23.5778732862916));
#101282=CARTESIAN_POINT('Ctrl Pts',(0.0118550622816464,-2.9419761143657,
23.5728463572199));
#101283=CARTESIAN_POINT('Ctrl Pts',(-0.0813707797332918,-2.94235177960579,
23.56781847891));
#101284=CARTESIAN_POINT('Ctrl Pts',(-0.174591271718575,-2.93829178273634,
23.5627906006002));
#101285=CARTESIAN_POINT('Ctrl Pts',(-0.267354722522535,-2.92982686388546,
23.5577627222904));
#101286=CARTESIAN_POINT('Ctrl Pts',(-0.360219976310396,-2.92135265523358,
23.5527293261498));
#101287=CARTESIAN_POINT('Ctrl Pts',(-0.452626743240865,-2.90846391566424,
23.5476959300093));
#101288=CARTESIAN_POINT('Ctrl Pts',(-0.544129547265214,-2.89124316441785,
23.5426625338688));
#101289=CARTESIAN_POINT('Ctrl Pts',(-0.635688320105321,-2.87401187988711,
23.5376260589896));
#101290=CARTESIAN_POINT('Ctrl Pts',(-0.726341596185885,-2.85244341210413,
23.5325895841104));
#101291=CARTESIAN_POINT('Ctrl Pts',(-0.815657327205701,-2.82667067847948,
23.5275531092312));
#101292=CARTESIAN_POINT('Ctrl Pts',(-0.905118546569044,-2.80085596308656,
23.5225084303282));
#101293=CARTESIAN_POINT('Ctrl Pts',(-0.993237450076915,-2.77082345365114,
23.5174637514251));
#101294=CARTESIAN_POINT('Ctrl Pts',(-1.07960046519243,-2.73675480004261,
23.5124190725221));
#101295=CARTESIAN_POINT('Ctrl Pts',(-1.12446952612382,-2.71905476383421,
23.5097981588732));
#101296=CARTESIAN_POINT('Ctrl Pts',(-1.16886501045896,-2.70026605650189,
23.5071772452242));
#101297=CARTESIAN_POINT('Ctrl Pts',(-1.21273165315311,-2.68041898542756,
23.5045563315753));
#101298=CARTESIAN_POINT('Ctrl Pts',(-1.29731811114346,-2.64214859725665,
23.4995025187315));
#101299=CARTESIAN_POINT('Ctrl Pts',(-1.38024241671689,-2.59980191982492,
23.4944487058877));
#101300=CARTESIAN_POINT('Ctrl Pts',(-1.46108486777875,-2.55354557608591,
23.4893948930439));
#101301=CARTESIAN_POINT('Ctrl Pts',(-1.54181597956702,-2.50735293832865,
23.4843480405018));
#101302=CARTESIAN_POINT('Ctrl Pts',(-1.62047055244664,-2.4572615527917,
23.4793011879597));
#101303=CARTESIAN_POINT('Ctrl Pts',(-1.69664992645296,-2.40348559951316,
23.4742543354176));
#101304=CARTESIAN_POINT('Ctrl Pts',(-1.77274788113775,-2.34976712113105,
23.4692128768725));
#101305=CARTESIAN_POINT('Ctrl Pts',(-1.84637553453101,-2.29237215718286,
23.4641714183273));
#101306=CARTESIAN_POINT('Ctrl Pts',(-1.91716082674176,-2.23155962600304,
23.4591299597822));
#101307=CARTESIAN_POINT('Ctrl Pts',(-1.98789512770512,-2.17079090204257,
23.4540921329273));
#101308=CARTESIAN_POINT('Ctrl Pts',(-2.05579080156047,-2.10660979278462,
23.4490543060725));
#101309=CARTESIAN_POINT('Ctrl Pts',(-2.12050752097289,-2.03931651626162,
23.4440164792177));
#101310=CARTESIAN_POINT('Ctrl Pts',(-2.18520071905583,-1.97204769751927,
23.4389804833639));
#101311=CARTESIAN_POINT('Ctrl Pts',(-2.24671695063373,-1.90166927830933,
23.4339444875102));
#101312=CARTESIAN_POINT('Ctrl Pts',(-2.30475229808391,-1.82851875693878,
23.4289084916565));
#101313=CARTESIAN_POINT('Ctrl Pts',(-2.36278276014744,-1.7553743933427,
23.4238729197304));
#101314=CARTESIAN_POINT('Ctrl Pts',(-2.41733264491014,-1.67945873945854,
23.4188373478043));
#101315=CARTESIAN_POINT('Ctrl Pts',(-2.46813867034164,-1.60114193748219,
23.4138017758782));
#101316=CARTESIAN_POINT('Ctrl Pts',(-2.51895460740193,-1.52280985686392,
23.4087652215741));
#101317=CARTESIAN_POINT('Ctrl Pts',(-2.56602499328706,-1.44207607044779,
23.4037286672701));
#101318=CARTESIAN_POINT('Ctrl Pts',(-2.60913080260939,-1.35933824152595,
23.398692112966));
#101319=CARTESIAN_POINT('Ctrl Pts',(-2.65228381918497,-1.27650980241248,
23.3936500428881));
#101320=CARTESIAN_POINT('Ctrl Pts',(-2.6914633869885,-1.19167333417574,
23.3886079728102));
#101321=CARTESIAN_POINT('Ctrl Pts',(-2.72649739255411,-1.10524927884872,
23.3835659027323));
#101322=CARTESIAN_POINT('Ctrl Pts',(-2.76155287297451,-1.01877224801954,
23.3785207420081));
#101323=CARTESIAN_POINT('Ctrl Pts',(-2.79245758527019,-0.930706111303744,
23.3734755812838));
#101324=CARTESIAN_POINT('Ctrl Pts',(-2.81908905840467,-0.841487302805616,
23.3684304205595));
#101325=CARTESIAN_POINT('Ctrl Pts',(-2.84576348825401,-0.752124583871262,
23.3633771219629));
#101326=CARTESIAN_POINT('Ctrl Pts',(-2.86815081188743,-0.661605911771167,
23.3583238233662));
#101327=CARTESIAN_POINT('Ctrl Pts',(-2.88617953089253,-0.570378572052812,
23.3532705247695));
#101328=CARTESIAN_POINT('Ctrl Pts',(-2.89522502556831,-0.524607354725887,
23.3507351485434));
#101329=CARTESIAN_POINT('Ctrl Pts',(-2.90317414490181,-0.478657840198326,
23.3481997723174));
#101330=CARTESIAN_POINT('Ctrl Pts',(-2.91002279202621,-0.432586811967262,
23.3456643960914));
#101331=CARTESIAN_POINT('Ctrl Pts',(-2.93117191285364,-0.290316123318043,
23.3378349697574));
#101332=CARTESIAN_POINT('Ctrl Pts',(-2.94189101104494,-0.146458298840477,
23.3300055434235));
#101333=CARTESIAN_POINT('Ctrl Pts',(-2.94199917298087,-0.00220594195414625,
23.3221761170896));
#101334=CARTESIAN_POINT('',(-2.94164694255709,-0.000931396376265734,22.3221761729126));
#101335=CARTESIAN_POINT('Ctrl Pts',(-2.94442704671558,-0.00218612406040982,
23.3221749436185));
#101336=CARTESIAN_POINT('Ctrl Pts',(-2.93738112964605,0.830075128864581,
23.2770407826148));
#101337=CARTESIAN_POINT('Ctrl Pts',(-2.13351380414281,2.65076091012592,
23.1789426431165));
#101338=CARTESIAN_POINT('Ctrl Pts',(0.955635603265417,3.34439215967238,
23.0278805251237));
#101339=CARTESIAN_POINT('Ctrl Pts',(3.32881183697859,1.00834644561564,22.8689885896398));
#101340=CARTESIAN_POINT('Ctrl Pts',(2.65081929289952,-2.25190969884369,
22.7100966541558));
#101341=CARTESIAN_POINT('Ctrl Pts',(-0.456994034995296,-3.44805916202772,
22.5512047186722));
#101342=CARTESIAN_POINT('Ctrl Pts',(-2.64523118583122,-1.84941700741083,
22.4218981138432));
#101343=CARTESIAN_POINT('Ctrl Pts',(-2.93865671149535,-0.434669198947471,
22.3455554875091));
#101344=CARTESIAN_POINT('Ctrl Pts',(-2.9374317399157,-0.00094243306318272,
22.3221768396696));
#101345=CARTESIAN_POINT('',(-2.94199878572312,0.00267297655470239,21.3221761170605));
#101346=CARTESIAN_POINT('Ctrl Pts',(-2.9419998528588,-0.000930472349394172,
22.3221761170896));
#101347=CARTESIAN_POINT('Ctrl Pts',(-2.94203019000661,0.094990577261412,
22.3170138242079));
#101348=CARTESIAN_POINT('Ctrl Pts',(-2.93736506348151,0.190871573344608,
22.3118515313263));
#101349=CARTESIAN_POINT('Ctrl Pts',(-2.92804241566056,0.286236985892223,
22.3066892384446));
#101350=CARTESIAN_POINT('Ctrl Pts',(-2.91871313585854,0.381670239853906,
22.3015232731912));
#101351=CARTESIAN_POINT('Ctrl Pts',(-2.9047197783399,0.476586770599642,
22.2963573079377));
#101352=CARTESIAN_POINT('Ctrl Pts',(-2.88615187045034,0.570518519152539,
22.2911913426843));
#101353=CARTESIAN_POINT('Ctrl Pts',(-2.8675510357606,0.66461683854007,22.2860162165331));
#101354=CARTESIAN_POINT('Ctrl Pts',(-2.84435952707144,0.757726482815267,
22.2808410903819));
#101355=CARTESIAN_POINT('Ctrl Pts',(-2.81671762109817,0.849391454510266,
22.2756659642308));
#101356=CARTESIAN_POINT('Ctrl Pts',(-2.78904978270547,0.941142422246759,
22.270485983004));
#101357=CARTESIAN_POINT('Ctrl Pts',(-2.75692336416446,1.03144562881346,
22.2653060017773));
#101358=CARTESIAN_POINT('Ctrl Pts',(-2.72052719543667,1.11986417876879,
22.2601260205505));
#101359=CARTESIAN_POINT('Ctrl Pts',(-2.68405381864556,1.20847029310912,
22.2549350509057));
#101360=CARTESIAN_POINT('Ctrl Pts',(-2.64329276694592,1.29518338866856,
22.2497440812609));
#101361=CARTESIAN_POINT('Ctrl Pts',(-2.59847956311998,1.37958977962575,
22.2445531116161));
#101362=CARTESIAN_POINT('Ctrl Pts',(-2.56644493080924,1.43992752538238,
22.2408423569788));
#101363=CARTESIAN_POINT('Ctrl Pts',(-2.53234058057719,1.49908706191697,
22.2371316023416));
#101364=CARTESIAN_POINT('Ctrl Pts',(-2.49626575990915,1.55692686273479,
22.2334208477043));
#101365=CARTESIAN_POINT('Ctrl Pts',(-2.44714850223653,1.63567797910606,
22.228368512355));
#101366=CARTESIAN_POINT('Ctrl Pts',(-2.39421284353252,1.71224383471465,
22.2233161770058));
#101367=CARTESIAN_POINT('Ctrl Pts',(-2.33767924232075,1.78623060102068,
22.2182638416566));
#101368=CARTESIAN_POINT('Ctrl Pts',(-2.28122359605779,1.86011534597203,
22.213218473041));
#101369=CARTESIAN_POINT('Ctrl Pts',(-2.22118013331467,1.9314277185992,22.2081731044254));
#101370=CARTESIAN_POINT('Ctrl Pts',(-2.15781367650433,1.9998010244749,22.2031277358099));
#101371=CARTESIAN_POINT('Ctrl Pts',(-2.09451501869394,2.0681011742678,22.1980877654912));
#101372=CARTESIAN_POINT('Ctrl Pts',(-2.02790073414699,2.13346818371392,
22.1930477951725));
#101373=CARTESIAN_POINT('Ctrl Pts',(-1.958276479213,2.19556763297357,22.1880078248538));
#101374=CARTESIAN_POINT('Ctrl Pts',(-1.88870239469447,2.25762233410381,
22.1829714862782));
#101375=CARTESIAN_POINT('Ctrl Pts',(-1.816122981461,2.31641386022739,22.1779351477026));
#101376=CARTESIAN_POINT('Ctrl Pts',(-1.74088064128557,2.37164470205744,
22.172898809127));
#101377=CARTESIAN_POINT('Ctrl Pts',(-1.66566564784683,2.42685547030546,
22.1678643010025));
#101378=CARTESIAN_POINT('Ctrl Pts',(-1.58779000794011,2.47850786257356,
22.162829792878));
#101379=CARTESIAN_POINT('Ctrl Pts',(-1.50762826327053,2.52634538806314,
22.1577952847535));
#101380=CARTESIAN_POINT('Ctrl Pts',(-1.42747322991276,2.5741789084933,22.1527611981287));
#101381=CARTESIAN_POINT('Ctrl Pts',(-1.34503285391046,2.61819796967141,
22.1477271115039));
#101382=CARTESIAN_POINT('Ctrl Pts',(-1.26070865911788,2.65819067728882,
22.1426930248791));
#101383=CARTESIAN_POINT('Ctrl Pts',(-1.17636793669289,2.69819122351972,
22.137657951568));
#101384=CARTESIAN_POINT('Ctrl Pts',(-1.0901430637071,2.73416365887391,22.1326228782568));
#101385=CARTESIAN_POINT('Ctrl Pts',(-1.00245698571702,2.76594359880804,
22.1275878049457));
#101386=CARTESIAN_POINT('Ctrl Pts',(-0.914674577582191,2.79775845153885,
22.1225472002053));
#101387=CARTESIAN_POINT('Ctrl Pts',(-0.825428178482752,2.82537146355402,
22.1175065954648));
#101388=CARTESIAN_POINT('Ctrl Pts',(-0.735157102062007,2.84866776498906,
22.1124659907244));
#101389=CARTESIAN_POINT('Ctrl Pts',(-0.64483055526435,2.87197838169178,
22.1074222885993));
#101390=CARTESIAN_POINT('Ctrl Pts',(-0.553478512257664,2.89096691674169,
22.1023785864742));
#101391=CARTESIAN_POINT('Ctrl Pts',(-0.461549559709994,2.90556982430839,
22.0973348843492));
#101392=CARTESIAN_POINT('Ctrl Pts',(-0.369471830695332,2.92019636500629,
22.0922830195706));
#101393=CARTESIAN_POINT('Ctrl Pts',(-0.276815769208732,2.93042306002186,
22.0872311547921));
#101394=CARTESIAN_POINT('Ctrl Pts',(-0.184033963419593,2.93623832484832,
22.0821792900136));
#101395=CARTESIAN_POINT('Ctrl Pts',(-0.137198725494143,2.93917380675052,
22.0796291640825));
#101396=CARTESIAN_POINT('Ctrl Pts',(-0.0903314332698338,2.9409860316533,
22.0770790381515));
#101397=CARTESIAN_POINT('Ctrl Pts',(-0.0434899276352311,2.94167853889481,
22.0745289122205));
#101398=CARTESIAN_POINT('Ctrl Pts',(0.0493134496888117,2.94305054882409,
22.0694765490269));
#101399=CARTESIAN_POINT('Ctrl Pts',(0.142348327697592,2.94002910592505,
22.0644241858333));
#101400=CARTESIAN_POINT('Ctrl Pts',(0.235164237631819,2.932586193335,22.0593718226397));
#101401=CARTESIAN_POINT('Ctrl Pts',(0.327852170320183,2.92515354324687,
22.0543264257898));
#101402=CARTESIAN_POINT('Ctrl Pts',(0.42032129591086,2.91331157310301,22.0492810289399));
#101403=CARTESIAN_POINT('Ctrl Pts',(0.512119923029994,2.89708425566737,
22.04423563209));
#101404=CARTESIAN_POINT('Ctrl Pts',(0.603820337012713,2.88087429944715,
22.0391956331884));
#101405=CARTESIAN_POINT('Ctrl Pts',(0.69485124325998,2.86028839847612,22.0341556342869));
#101406=CARTESIAN_POINT('Ctrl Pts',(0.784765960818846,2.83540233242834,
22.0291156353853));
#101407=CARTESIAN_POINT('Ctrl Pts',(0.874615894393207,2.8105341969103,22.0240792678271));
#101408=CARTESIAN_POINT('Ctrl Pts',(0.96335081086689,2.7813721727628,22.0190429002689));
#101409=CARTESIAN_POINT('Ctrl Pts',(1.05053515120018,2.74804292107907,22.0140065327107));
#101410=CARTESIAN_POINT('Ctrl Pts',(1.13768780878291,2.71472578123061,22.0089719953662));
#101411=CARTESIAN_POINT('Ctrl Pts',(1.22329059510423,2.67724458077506,22.0039374580218));
#101412=CARTESIAN_POINT('Ctrl Pts',(1.30692502077597,2.63577521614984,21.9989029206773));
#101413=CARTESIAN_POINT('Ctrl Pts',(1.3905524477864,2.59430932174679,21.9938688046309));
#101414=CARTESIAN_POINT('Ctrl Pts',(1.47221144372437,2.54885612423029,21.9888346885845));
#101415=CARTESIAN_POINT('Ctrl Pts',(1.55150639027973,2.49963835802725,21.983800572538));
#101416=CARTESIAN_POINT('Ctrl Pts',(1.63081688125524,2.45041094352164,21.9787654696392));
#101417=CARTESIAN_POINT('Ctrl Pts',(1.70776202524664,2.39741772927431,21.9737303667403));
#101418=CARTESIAN_POINT('Ctrl Pts',(1.78197453581782,2.34092519181987,21.9686952638414));
#101419=CARTESIAN_POINT('Ctrl Pts',(1.85626857534372,2.28437059235602,21.9636546294401));
#101420=CARTESIAN_POINT('Ctrl Pts',(1.92782363501229,2.22430926548201,21.9586139950389));
#101421=CARTESIAN_POINT('Ctrl Pts',(1.9963051829809,2.16104826794859,21.9535733606376));
#101422=CARTESIAN_POINT('Ctrl Pts',(2.06482881286728,2.09774839652614,21.9485296287661));
#101423=CARTESIAN_POINT('Ctrl Pts',(2.13027485970737,2.0312452565218,21.9434858968945));
#101424=CARTESIAN_POINT('Ctrl Pts',(2.19234691041335,1.96188150111087,21.938442165023));
#101425=CARTESIAN_POINT('Ctrl Pts',(2.25451941509935,1.89240549122758,21.9333902706542));
#101426=CARTESIAN_POINT('Ctrl Pts',(2.31330674307987,1.82005996813581,21.9283383762854));
#101427=CARTESIAN_POINT('Ctrl Pts',(2.36845399122824,1.7452190955393,21.9232864819167));
#101428=CARTESIAN_POINT('Ctrl Pts',(2.39628837899023,1.70744477427684,21.9207366468566));
#101429=CARTESIAN_POINT('Ctrl Pts',(2.42319615647617,1.66903519809311,21.9181868117966));
#101430=CARTESIAN_POINT('Ctrl Pts',(2.44914897657549,1.63004088615569,21.9156369767366));
#101431=CARTESIAN_POINT('Ctrl Pts',(2.50057304152298,1.55277583280201,21.9105846208373));
#101432=CARTESIAN_POINT('Ctrl Pts',(2.54842948649866,1.47293629093071,21.905532264938));
#101433=CARTESIAN_POINT('Ctrl Pts',(2.59245074570147,1.39088573618105,21.9004799090386));
#101434=CARTESIAN_POINT('Ctrl Pts',(2.63641130662138,1.30894831603668,21.8954345195309));
#101435=CARTESIAN_POINT('Ctrl Pts',(2.6765469817218,1.22480632910527,21.8903891300231));
#101436=CARTESIAN_POINT('Ctrl Pts',(2.71263324413171,1.13885244120187,21.8853437405153));
#101437=CARTESIAN_POINT('Ctrl Pts',(2.74868089839694,1.05299051405911,21.8803037489933));
#101438=CARTESIAN_POINT('Ctrl Pts',(2.78068758024804,0.965320946466707,
21.8752637574712));
#101439=CARTESIAN_POINT('Ctrl Pts',(2.80847502456532,0.876260256084261,
21.8702237659491));
#101440=CARTESIAN_POINT('Ctrl Pts',(2.83624244773248,0.787263734879458,
21.8651874057947));
#101441=CARTESIAN_POINT('Ctrl Pts',(2.85979654387253,0.696878505994045,
21.8601510456403));
#101442=CARTESIAN_POINT('Ctrl Pts',(2.87900784223665,0.605539300409035,
21.8551146854859));
#101443=CARTESIAN_POINT('Ctrl Pts',(2.89821215916643,0.514233287722003,
21.8500801555575));
#101444=CARTESIAN_POINT('Ctrl Pts',(2.91307672221103,0.421974421338534,
21.845045625629));
#101445=CARTESIAN_POINT('Ctrl Pts',(2.92352269319776,0.329209754347786,
21.8400110957006));
#101446=CARTESIAN_POINT('Ctrl Pts',(2.93396779004153,0.23645285011844,21.8349769870733));
#101447=CARTESIAN_POINT('Ctrl Pts',(2.93999498046764,0.143190670907543,
21.829942878446));
#101448=CARTESIAN_POINT('Ctrl Pts',(2.94157718631606,0.0498764167204417,
21.8249087698186));
#101449=CARTESIAN_POINT('Ctrl Pts',(2.94315970233135,-0.0434561302754896,
21.8198736743326));
#101450=CARTESIAN_POINT('Ctrl Pts',(2.94029549606274,-0.136840328366542,
21.8148385788465));
#101451=CARTESIAN_POINT('Ctrl Pts',(2.93300960511188,-0.229823097885035,
21.8098034833604));
#101452=CARTESIAN_POINT('Ctrl Pts',(2.92571570987932,-0.322908018298392,
21.8047628563172));
#101453=CARTESIAN_POINT('Ctrl Pts',(2.91399046826226,-0.415590186266749,
21.7997222292739));
#101454=CARTESIAN_POINT('Ctrl Pts',(2.89791077156557,-0.507422072878408,
21.7946816022306));
#101455=CARTESIAN_POINT('Ctrl Pts',(2.88182119381464,-0.599310390644901,
21.7896378776967));
#101456=CARTESIAN_POINT('Ctrl Pts',(2.86137193120887,-0.690346953737875,
21.7845941531628));
#101457=CARTESIAN_POINT('Ctrl Pts',(2.83669044521521,-0.780096992703287,
21.779550428629));
#101458=CARTESIAN_POINT('Ctrl Pts',(2.81196901550317,-0.869992280227979,
21.7744985414945));
#101459=CARTESIAN_POINT('Ctrl Pts',(2.7830018265317,-0.95859646532433,21.76944665436));
#101460=CARTESIAN_POINT('Ctrl Pts',(2.74996531240784,-1.04549260186461,
21.7643947672255));
#101461=CARTESIAN_POINT('Ctrl Pts',(2.73329033706895,-1.08935288713628,
21.7618448585679));
#101462=CARTESIAN_POINT('Ctrl Pts',(2.71557938353974,-1.1327783733076,21.7592949499103));
#101463=CARTESIAN_POINT('Ctrl Pts',(2.69685956413281,-1.1757178621359,21.7567450412526));
#101464=CARTESIAN_POINT('Ctrl Pts',(2.65976838277848,-1.26079754868474,
21.7516926888554));
#101465=CARTESIAN_POINT('Ctrl Pts',(2.61858059949813,-1.34427296168509,
21.7466403364581));
#101466=CARTESIAN_POINT('Ctrl Pts',(2.57345680430365,-1.42572229988285,
21.7415879840608));
#101467=CARTESIAN_POINT('Ctrl Pts',(2.52839522836952,-1.50705933109143,
21.736542598135));
#101468=CARTESIAN_POINT('Ctrl Pts',(2.47940863847927,-1.58637545365499,
21.7314972122091));
#101469=CARTESIAN_POINT('Ctrl Pts',(2.42670547512277,-1.66326923166671,
21.7264518262833));
#101470=CARTESIAN_POINT('Ctrl Pts',(2.37405869889898,-1.74008074099873,
21.7214118384175));
#101471=CARTESIAN_POINT('Ctrl Pts',(2.31770350264379,-1.81447469265057,
21.7163718505518));
#101472=CARTESIAN_POINT('Ctrl Pts',(2.25789343583091,-1.88607561683822,
21.7113318626861));
#101473=CARTESIAN_POINT('Ctrl Pts',(2.19812646397875,-1.95762495039608,
21.706295506284));
#101474=CARTESIAN_POINT('Ctrl Pts',(2.13490985345959,-2.02638491657892,
21.7012591498818));
#101475=CARTESIAN_POINT('Ctrl Pts',(2.06853889501785,-2.09201119495053,
21.6962227934797));
#101476=CARTESIAN_POINT('Ctrl Pts',(2.00219205673494,-2.15761362379073,
21.6911882673618));
#101477=CARTESIAN_POINT('Ctrl Pts',(1.93269346342445,-2.22008431519057,
21.6861537412438));
#101478=CARTESIAN_POINT('Ctrl Pts',(1.86037619083133,-2.27911483444514,
21.6811192151259));
#101479=CARTESIAN_POINT('Ctrl Pts',(1.78806497068942,-2.33814041325707,
21.6760851103627));
#101480=CARTESIAN_POINT('Ctrl Pts',(1.71293588455987,-2.39372611160138,
21.6710510055994));
#101481=CARTESIAN_POINT('Ctrl Pts',(1.63535521318685,-2.44560367326814,
21.6660169008362));
#101482=CARTESIAN_POINT('Ctrl Pts',(1.55775933407516,-2.4974914042256,21.6609818092634));
#101483=CARTESIAN_POINT('Ctrl Pts',(1.47771128477066,-2.54566930828948,
21.6559467176906));
#101484=CARTESIAN_POINT('Ctrl Pts',(1.39560547561088,-2.58991300171356,
21.6509116261178));
#101485=CARTESIAN_POINT('Ctrl Pts',(1.31340946575208,-2.6342053008589,21.6458710030389));
#101486=CARTESIAN_POINT('Ctrl Pts',(1.22915157522609,-2.67455455091527,
21.6408303799601));
#101487=CARTESIAN_POINT('Ctrl Pts',(1.1432496373168,-2.71078296194568,21.6357897568812));
#101488=CARTESIAN_POINT('Ctrl Pts',(1.05729491279115,-2.74703363528217,
21.6307460363468));
#101489=CARTESIAN_POINT('Ctrl Pts',(0.969694546411809,-2.77915827554041,
21.6257023158124));
#101490=CARTESIAN_POINT('Ctrl Pts',(0.880883039653029,-2.80702851258259,
21.620658595278));
#101491=CARTESIAN_POINT('Ctrl Pts',(0.791927803389455,-2.83494385386312,
21.6156067121588));
#101492=CARTESIAN_POINT('Ctrl Pts',(0.701757942888001,-2.85859093399181,
21.6105548290395));
#101493=CARTESIAN_POINT('Ctrl Pts',(0.610819505872041,-2.87789220285372,
21.6055029459203));
#101494=CARTESIAN_POINT('Ctrl Pts',(0.564918172951121,-2.88763455159973,
21.6029529992031));
#101495=CARTESIAN_POINT('Ctrl Pts',(0.51882113440247,-2.89627052047224,
21.600403052486));
#101496=CARTESIAN_POINT('Ctrl Pts',(0.472586115470197,-2.90379516554884,
21.5978531057688));
#101497=CARTESIAN_POINT('Ctrl Pts',(0.380978007886807,-2.91870417849233,
21.592800749382));
#101498=CARTESIAN_POINT('Ctrl Pts',(0.288499320069357,-2.9293006517501,
21.5877483929951));
#101499=CARTESIAN_POINT('Ctrl Pts',(0.195591599580818,-2.93549108773531,
21.5826960366083));
#101500=CARTESIAN_POINT('Ctrl Pts',(0.102811984375719,-2.94167298807296,
21.5776506466344));
#101501=CARTESIAN_POINT('Ctrl Pts',(0.00960495143632237,-2.94346089414566,
21.5726052566605));
#101502=CARTESIAN_POINT('Ctrl Pts',(-0.0835791501822573,-2.94081256214245,
21.5675598666867));
#101503=CARTESIAN_POINT('Ctrl Pts',(-0.176663555147768,-2.93816706356073,
21.5625198747204));
#101504=CARTESIAN_POINT('Ctrl Pts',(-0.269724635881426,-2.93109477341955,
21.5574798827542));
#101505=CARTESIAN_POINT('Ctrl Pts',(-0.362309434755363,-2.91960543113059,
21.552439890788));
#101506=CARTESIAN_POINT('Ctrl Pts',(-0.454827524660897,-2.90812436711389,
21.5474035302242));
#101507=CARTESIAN_POINT('Ctrl Pts',(-0.546869575213149,-2.89223263129561,
21.5423671696604));
#101508=CARTESIAN_POINT('Ctrl Pts',(-0.637986201359988,-2.87199192319099,
21.5373308090966));
#101509=CARTESIAN_POINT('Ctrl Pts',(-0.729069715103207,-2.85175857069778,
21.5322962787806));
#101510=CARTESIAN_POINT('Ctrl Pts',(-0.819228039316954,-2.82717948188605,
21.5272617484646));
#101511=CARTESIAN_POINT('Ctrl Pts',(-0.908021485893451,-2.79836755647929,
21.5222272181486));
#101512=CARTESIAN_POINT('Ctrl Pts',(-0.996807501635577,-2.76955804224873,
21.5171931091561));
#101513=CARTESIAN_POINT('Ctrl Pts',(-1.08422844434704,-2.73651653300771,
21.5121590001635));
#101514=CARTESIAN_POINT('Ctrl Pts',(-1.16986041220074,-2.69940560419614,
21.507124891171));
#101515=CARTESIAN_POINT('Ctrl Pts',(-1.25550916647857,-2.66228740053375,
21.5020897953427));
#101516=CARTESIAN_POINT('Ctrl Pts',(-1.33936784198538,-2.62109836998623,
21.4970546995144));
#101517=CARTESIAN_POINT('Ctrl Pts',(-1.42103417753485,-2.5760484984328,
21.492019603686));
#101518=CARTESIAN_POINT('Ctrl Pts',(-1.5027902311323,-2.53094913541497,
21.4869789763377));
#101519=CARTESIAN_POINT('Ctrl Pts',(-1.58234874756784,-2.48198067978894,
21.4819383489894));
#101520=CARTESIAN_POINT('Ctrl Pts',(-1.65933394333949,-2.42939804570627,
21.4768977216411));
#101521=CARTESIAN_POINT('Ctrl Pts',(-1.73636644658095,-2.37678309954918,
21.4718539968228));
#101522=CARTESIAN_POINT('Ctrl Pts',(-1.81082212685152,-2.32054982106105,
21.4668102720046));
#101523=CARTESIAN_POINT('Ctrl Pts',(-1.88235771278168,-2.26099390559358,
21.4617665471864));
#101524=CARTESIAN_POINT('Ctrl Pts',(-1.95400906908359,-2.2013416071807,
21.4567146598028));
#101525=CARTESIAN_POINT('Ctrl Pts',(-2.02273056957333,-2.1383562366254,
21.4516627724192));
#101526=CARTESIAN_POINT('Ctrl Pts',(-2.08821540652036,-2.07237072358471,
21.4466108850356));
#101527=CARTESIAN_POINT('Ctrl Pts',(-2.12126842117285,-2.03906499616646,
21.4440609801187));
#101528=CARTESIAN_POINT('Ctrl Pts',(-2.15349747733302,-2.00499547140519,
21.4415110752018));
#101529=CARTESIAN_POINT('Ctrl Pts',(-2.18486715170584,-1.97020799140518,
21.4389611702849));
#101530=CARTESIAN_POINT('Ctrl Pts',(-2.24637569772523,-1.90199793321173,
21.4339614070722));
#101531=CARTESIAN_POINT('Ctrl Pts',(-2.30480892287151,-1.83076923906431,
21.4289616438594));
#101532=CARTESIAN_POINT('Ctrl Pts',(-2.35985162593047,-1.75683360156656,
21.4239618806467));
#101533=CARTESIAN_POINT('Ctrl Pts',(-2.41482437391578,-1.68299193061985,
21.4189684717513));
#101534=CARTESIAN_POINT('Ctrl Pts',(-2.46641488452217,-1.60645050518711,
21.4139750628559));
#101535=CARTESIAN_POINT('Ctrl Pts',(-2.51434576883271,-1.52755666171604,
21.4089816539605));
#101536=CARTESIAN_POINT('Ctrl Pts',(-2.56222981774856,-1.44873990892149,
21.4039931243465));
#101537=CARTESIAN_POINT('Ctrl Pts',(-2.6064611061311,-1.36757568765215,
21.3990045947326));
#101538=CARTESIAN_POINT('Ctrl Pts',(-2.6468042042926,-1.28444209839876,
21.3940160651187));
#101539=CARTESIAN_POINT('Ctrl Pts',(-2.6871197281023,-1.20136533063258,
21.3890309451455));
#101540=CARTESIAN_POINT('Ctrl Pts',(-2.72355214294089,-1.1163222758734,
21.3840458251723));
#101541=CARTESIAN_POINT('Ctrl Pts',(-2.75591147754233,-1.02971643084418,
21.3790607051992));
#101542=CARTESIAN_POINT('Ctrl Pts',(-2.78826639365761,-0.9431224113587,
21.3740762659162));
#101543=CARTESIAN_POINT('Ctrl Pts',(-2.81654916256314,-0.854966445684254,
21.3690918266333));
#101544=CARTESIAN_POINT('Ctrl Pts',(-2.84061796367395,-0.765671982282783,
21.3641073873503));
#101545=CARTESIAN_POINT('Ctrl Pts',(-2.86468387395497,-0.67638824376513,
21.3591235467331));
#101546=CARTESIAN_POINT('Ctrl Pts',(-2.88453671004305,-0.585966719553561,
21.3541397061159));
#101547=CARTESIAN_POINT('Ctrl Pts',(-2.9000850035322,-0.494844391993714,
21.3491558654986));
#101548=CARTESIAN_POINT('Ctrl Pts',(-2.91564403480524,-0.403659134578519,
21.3441685829986));
#101549=CARTESIAN_POINT('Ctrl Pts',(-2.92689251344888,-0.311772556206746,
21.3391813004986));
#101550=CARTESIAN_POINT('Ctrl Pts',(-2.93379052609947,-0.219629572164131,
21.3341940179986));
#101551=CARTESIAN_POINT('Ctrl Pts',(-2.93933126112593,-0.145616971000863,
21.3301880510289));
#101552=CARTESIAN_POINT('Ctrl Pts',(-2.94206612089074,-0.0714391666931478,
21.3261820840593));
#101553=CARTESIAN_POINT('Ctrl Pts',(-2.94199878572361,0.00267297601551483,
21.3221761170896));
#101554=CARTESIAN_POINT('',(-2.94199995448535,-0.000517501908736848,20.3221761170572));
#101555=CARTESIAN_POINT('Ctrl Pts',(-2.94199878572312,0.00267297655470376,
21.3221761170605));
#101556=CARTESIAN_POINT('Ctrl Pts',(-2.94189240953056,0.11975542114466,
21.3158474860343));
#101557=CARTESIAN_POINT('Ctrl Pts',(-2.93479312830803,0.236526265844601,
21.3095188550082));
#101558=CARTESIAN_POINT('Ctrl Pts',(-2.92083380798487,0.352269592971963,
21.3031902239821));
#101559=CARTESIAN_POINT('Ctrl Pts',(-2.90660046919479,0.470284936810828,
21.2967373632849));
#101560=CARTESIAN_POINT('Ctrl Pts',(-2.88523514508262,0.587232220707165,
21.2902845025877));
#101561=CARTESIAN_POINT('Ctrl Pts',(-2.85692692874275,0.702376340592786,
21.2838316418906));
#101562=CARTESIAN_POINT('Ctrl Pts',(-2.8514251294196,0.724754996783811,
21.2825775061941));
#101563=CARTESIAN_POINT('Ctrl Pts',(-2.84566121807922,0.747065607135637,
21.2813233704976));
#101564=CARTESIAN_POINT('Ctrl Pts',(-2.83963679003616,0.769302866674205,
21.2800692348011));
#101565=CARTESIAN_POINT('Ctrl Pts',(-2.81536704985242,0.858886891504768,
21.2750168800727));
#101566=CARTESIAN_POINT('Ctrl Pts',(-2.78681035035391,0.947482047980881,
21.2699645253443));
#101567=CARTESIAN_POINT('Ctrl Pts',(-2.75406396661295,1.03464760561465,
21.264912170616));
#101568=CARTESIAN_POINT('Ctrl Pts',(-2.72136273518789,1.12169297511333,
21.2598667823215));
#101569=CARTESIAN_POINT('Ctrl Pts',(-2.6844834539253,1.20731225054544,21.254821394027));
#101570=CARTESIAN_POINT('Ctrl Pts',(-2.643573709314,1.29107786110049,21.2497760057324));
#101571=CARTESIAN_POINT('Ctrl Pts',(-2.6027077337561,1.37475385140695,21.244736015464));
#101572=CARTESIAN_POINT('Ctrl Pts',(-2.55782005984269,1.45657972176175,
21.2396960251957));
#101573=CARTESIAN_POINT('Ctrl Pts',(-2.50910669122713,1.53614700209298,
21.2346560349273));
#101574=CARTESIAN_POINT('Ctrl Pts',(-2.46042842165539,1.61565695246453,
21.2296196760817));
#101575=CARTESIAN_POINT('Ctrl Pts',(-2.40793016759864,1.69291116964257,
21.2245833172361));
#101576=CARTESIAN_POINT('Ctrl Pts',(-2.35185377514653,1.76752590372221,
21.2195469583906));
#101577=CARTESIAN_POINT('Ctrl Pts',(-2.29579776137878,1.84211352211112,
21.2145124298048));
#101578=CARTESIAN_POINT('Ctrl Pts',(-2.23616645908777,1.91406320821207,
21.2094779012191));
#101579=CARTESIAN_POINT('Ctrl Pts',(-2.17324433457103,1.98302119561414,
21.2044433726333));
#101580=CARTESIAN_POINT('Ctrl Pts',(-2.11032747592742,2.05197341200932,
21.1994092653809));
#101581=CARTESIAN_POINT('Ctrl Pts',(-2.04412064219976,2.11793409946989,
21.1943751581285));
#101582=CARTESIAN_POINT('Ctrl Pts',(-1.97494701584284,2.18058439061951,
21.1893410508761));
#101583=CARTESIAN_POINT('Ctrl Pts',(-1.90575982949065,2.24324696300544,
21.1843059567957));
#101584=CARTESIAN_POINT('Ctrl Pts',(-1.83360502499238,2.30259755237567,
21.1792708627153));
#101585=CARTESIAN_POINT('Ctrl Pts',(-1.75884001937715,2.35835658589565,
21.1742357686349));
#101586=CARTESIAN_POINT('Ctrl Pts',(-1.68399287745445,2.4141768758963,21.1691951430357));
#101587=CARTESIAN_POINT('Ctrl Pts',(-1.6065301671167,2.46639746806327,21.1641545174365));
#101588=CARTESIAN_POINT('Ctrl Pts',(-1.52683928116303,2.51478146356648,
21.1591138918373));
#101589=CARTESIAN_POINT('Ctrl Pts',(-1.44709942512561,2.56319519105577,
21.1540701687715));
#101590=CARTESIAN_POINT('Ctrl Pts',(-1.36512905761604,2.60776741632088,
21.1490264457057));
#101591=CARTESIAN_POINT('Ctrl Pts',(-1.28133927752646,2.64830769659947,
21.1439827226398));
#101592=CARTESIAN_POINT('Ctrl Pts',(-1.1974138951143,2.68891358578833,21.1389308369967));
#101593=CARTESIAN_POINT('Ctrl Pts',(-1.111663629993,2.72547432934193,21.1338789513535));
#101594=CARTESIAN_POINT('Ctrl Pts',(-1.02451842458105,2.75784807371508,
21.1288270657103));
#101595=CARTESIAN_POINT('Ctrl Pts',(-0.980532177941858,2.77418861130289,
21.1262771435793));
#101596=CARTESIAN_POINT('Ctrl Pts',(-0.936190770239545,2.78946322732056,
21.1237272214482));
#101597=CARTESIAN_POINT('Ctrl Pts',(-0.891550584329987,2.80365860182385,
21.1211772993172));
#101598=CARTESIAN_POINT('Ctrl Pts',(-0.803101577759515,2.83178498049207,
21.1161249440295));
#101599=CARTESIAN_POINT('Ctrl Pts',(-0.713161579104362,2.85577217652358,
21.1110725887419));
#101600=CARTESIAN_POINT('Ctrl Pts',(-0.622153749527225,2.87546321693553,
21.1060202334542));
#101601=CARTESIAN_POINT('Ctrl Pts',(-0.531271405829407,2.89512710641407,
21.1009748445918));
#101602=CARTESIAN_POINT('Ctrl Pts',(-0.439324587436848,2.91050651838266,
21.0959294557295));
#101603=CARTESIAN_POINT('Ctrl Pts',(-0.346752647075515,2.92149389897465,
21.0908840668671));
#101604=CARTESIAN_POINT('Ctrl Pts',(-0.254279748641262,2.93246952426214,
21.0858440760231));
#101605=CARTESIAN_POINT('Ctrl Pts',(-0.161183496380621,2.9390624060705,
21.0808040851791));
#101606=CARTESIAN_POINT('Ctrl Pts',(-0.0679134145633014,2.9412160356088,
21.0757640943351));
#101607=CARTESIAN_POINT('Ctrl Pts',(0.0252894643036301,2.94336811341415,
21.0707277349049));
#101608=CARTESIAN_POINT('Ctrl Pts',(0.118665480934454,2.94108728633357,
21.0656913754746));
#101609=CARTESIAN_POINT('Ctrl Pts',(0.211761057785966,2.93436897039302,
21.0606550160444));
#101610=CARTESIAN_POINT('Ctrl Pts',(0.304822802940564,2.92765309594363,
21.0556204868684));
#101611=CARTESIAN_POINT('Ctrl Pts',(0.397603868137938,2.91650296822374,
21.0505859576925));
#101612=CARTESIAN_POINT('Ctrl Pts',(0.489652792247862,2.90096607064679,
21.0455514285166));
#101613=CARTESIAN_POINT('Ctrl Pts',(0.581694012986908,2.88543047331844,
21.0405173206694));
#101614=CARTESIAN_POINT('Ctrl Pts',(0.673002776447296,2.86550891017267,
21.0354832128221));
#101615=CARTESIAN_POINT('Ctrl Pts',(0.763135984593806,2.84130031306408,
21.0304491049748));
#101616=CARTESIAN_POINT('Ctrl Pts',(0.853286861478556,2.81708697036422,
21.0254140102955));
#101617=CARTESIAN_POINT('Ctrl Pts',(0.942261296475986,2.78858504027873,
21.0203789156162));
#101618=CARTESIAN_POINT('Ctrl Pts',(1.02963067704451,2.75594351699901,21.0153438209369));
#101619=CARTESIAN_POINT('Ctrl Pts',(1.11709604102944,2.7232661339604,21.0103031947363));
#101620=CARTESIAN_POINT('Ctrl Pts',(1.20295241404228,2.68644023564748,21.0052625685357));
#101621=CARTESIAN_POINT('Ctrl Pts',(1.28679081669276,2.64566312936382,21.0002219423351));
#101622=CARTESIAN_POINT('Ctrl Pts',(1.37068073811,2.60486096551512,20.9951782186656));
#101623=CARTESIAN_POINT('Ctrl Pts',(1.45254983097636,2.56010297292139,20.9901344949961));
#101624=CARTESIAN_POINT('Ctrl Pts',(1.53201532440119,2.51163155056627,20.9850907713266));
#101625=CARTESIAN_POINT('Ctrl Pts',(1.61160942182922,2.46308168386145,20.9800388850821));
#101626=CARTESIAN_POINT('Ctrl Pts',(1.68879178678088,2.41080663864604,20.9749869988375));
#101627=CARTESIAN_POINT('Ctrl Pts',(1.76321028395472,2.35509097373251,20.969935112593));
#101628=CARTESIAN_POINT('Ctrl Pts',(1.80077267675144,2.32696874915272,20.9673851963398));
#101629=CARTESIAN_POINT('Ctrl Pts',(1.83763147156774,2.29797058715442,20.9648352800866));
#101630=CARTESIAN_POINT('Ctrl Pts',(1.87374493010958,2.26813666627226,20.9622853638334));
#101631=CARTESIAN_POINT('Ctrl Pts',(1.9452994429478,2.20902430869222,20.9572330087656));
#101632=CARTESIAN_POINT('Ctrl Pts',(2.01418231319909,2.14641649512292,20.9521806536979));
#101633=CARTESIAN_POINT('Ctrl Pts',(2.08003236992982,2.08058389401728,20.9471282986302));
#101634=CARTESIAN_POINT('Ctrl Pts',(2.14579162946986,2.0148420660337,20.94208290999));
#101635=CARTESIAN_POINT('Ctrl Pts',(2.20852607379946,1.94588459762376,20.9370375213498));
#101636=CARTESIAN_POINT('Ctrl Pts',(2.2679073017104,1.87402253744416,20.9319921327096));
#101637=CARTESIAN_POINT('Ctrl Pts',(2.32722499812845,1.8022373618984,20.9269521420897));
#101638=CARTESIAN_POINT('Ctrl Pts',(2.38319632753376,1.72755411202577,20.9219121514698));
#101639=CARTESIAN_POINT('Ctrl Pts',(2.43553028618555,1.65032003716641,20.9168721608499));
#101640=CARTESIAN_POINT('Ctrl Pts',(2.48782653715735,1.57314161102642,20.9118358016455));
#101641=CARTESIAN_POINT('Ctrl Pts',(2.53649037810421,1.49341637973467,20.9067994424412));
#101642=CARTESIAN_POINT('Ctrl Pts',(2.58127225646249,1.41152312698625,20.9017630832369));
#101643=CARTESIAN_POINT('Ctrl Pts',(2.6260378607082,1.3296596349371,20.896728554288));
#101644=CARTESIAN_POINT('Ctrl Pts',(2.66692409202634,1.24563007601361,20.8916940253391));
#101645=CARTESIAN_POINT('Ctrl Pts',(2.7037263109431,1.15983965939867,20.8866594963902));
#101646=CARTESIAN_POINT('Ctrl Pts',(2.74052544995759,1.07405642240787,20.8816253887707));
#101647=CARTESIAN_POINT('Ctrl Pts',(2.77324108115085,0.986513029051207,
20.8765912811513));
#101648=CARTESIAN_POINT('Ctrl Pts',(2.80171634164585,0.897635527903511,
20.8715571735318));
#101649=CARTESIAN_POINT('Ctrl Pts',(2.83019718411992,0.808740604181175,
20.8665220790808));
#101650=CARTESIAN_POINT('Ctrl Pts',(2.85443586987536,0.718511476424425,
20.8614869846299));
#101651=CARTESIAN_POINT('Ctrl Pts',(2.87432546396001,0.627389135410446,
20.8564518901789));
#101652=CARTESIAN_POINT('Ctrl Pts',(2.8942369086229,0.536166687987395,20.8514112642061));
#101653=CARTESIAN_POINT('Ctrl Pts',(2.90978962952486,0.444049503253866,
20.8463706382332));
#101654=CARTESIAN_POINT('Ctrl Pts',(2.92092793772647,0.351488239645315,
20.8413300122604));
#101655=CARTESIAN_POINT('Ctrl Pts',(2.93207309042788,0.258870097062211,
20.8362862888186));
#101656=CARTESIAN_POINT('Ctrl Pts',(2.9387983980545,0.16580777509446,20.8312425653768));
#101657=CARTESIAN_POINT('Ctrl Pts',(2.94110027163261,0.0727543277242745,
20.826198841935));
#101658=CARTESIAN_POINT('Ctrl Pts',(2.94340587047861,-0.0204497139370955,
20.821146955916));
#101659=CARTESIAN_POINT('Ctrl Pts',(2.94127375394385,-0.113644408764254,
20.8160950698969));
#101660=CARTESIAN_POINT('Ctrl Pts',(2.9347523666932,-0.206379616698647,
20.8110431838779));
#101661=CARTESIAN_POINT('Ctrl Pts',(2.93146072353358,-0.253187328174839,
20.8084932653684));
#101662=CARTESIAN_POINT('Ctrl Pts',(2.92705165208535,-0.29987809960563,
20.8059433468589));
#101663=CARTESIAN_POINT('Ctrl Pts',(2.92153631622689,-0.346395082192867,
20.8033934283495));
#101664=CARTESIAN_POINT('Ctrl Pts',(2.91060834546502,-0.438562855595892,
20.7983410733104));
#101665=CARTESIAN_POINT('Ctrl Pts',(2.89529496721321,-0.530378368764436,
20.7932887182714));
#101666=CARTESIAN_POINT('Ctrl Pts',(2.87562805568234,-0.621391410765094,
20.7882363632323));
#101667=CARTESIAN_POINT('Ctrl Pts',(2.85598826182905,-0.712278959633502,
20.7831909746219));
#101668=CARTESIAN_POINT('Ctrl Pts',(2.83200695617007,-0.802365805612182,
20.7781455860114));
#101669=CARTESIAN_POINT('Ctrl Pts',(2.80376770668779,-0.891207409604904,
20.773100197401));
#101670=CARTESIAN_POINT('Ctrl Pts',(2.77555867015495,-0.979953962668943,
20.7680602068118));
#101671=CARTESIAN_POINT('Ctrl Pts',(2.74310087848207,-1.06745750075294,
20.7630202162227));
#101672=CARTESIAN_POINT('Ctrl Pts',(2.70652858702614,-1.15328531058462,
20.7579802256336));
#101673=CARTESIAN_POINT('Ctrl Pts',(2.6699826466595,-1.23905127971149,20.7529438664615));
#101674=CARTESIAN_POINT('Ctrl Pts',(2.6293282726804,-1.3231435129482,20.7479075072894));
#101675=CARTESIAN_POINT('Ctrl Pts',(2.58474868127479,-1.40514705801502,
20.7428711481173));
#101676=CARTESIAN_POINT('Ctrl Pts',(2.54018529047687,-1.48712080228686,
20.7378366192016));
#101677=CARTESIAN_POINT('Ctrl Pts',(2.49169972802963,-1.56700697641706,
20.7328020902858));
#101678=CARTESIAN_POINT('Ctrl Pts',(2.4395217518428,-1.64441406655557,20.72776756137));
#101679=CARTESIAN_POINT('Ctrl Pts',(2.38734814233266,-1.7218146786403,20.7227334537845));
#101680=CARTESIAN_POINT('Ctrl Pts',(2.33148298192939,-1.79673625097007,
20.717699346199));
#101681=CARTESIAN_POINT('Ctrl Pts',(2.27219942586216,-1.86881614106676,
20.7126652386135));
#101682=CARTESIAN_POINT('Ctrl Pts',(2.21290424850348,-1.94091016090645,
20.7076301441973));
#101683=CARTESIAN_POINT('Ctrl Pts',(2.1501896271088,-2.01016104936067,20.7025950497811));
#101684=CARTESIAN_POINT('Ctrl Pts',(2.08436832254254,-2.07624003814135,
20.6975599553649));
#101685=CARTESIAN_POINT('Ctrl Pts',(2.01847470713354,-2.14239162085491,
20.6925193294279));
#101686=CARTESIAN_POINT('Ctrl Pts',(1.9494679098428,-2.20536403295075,20.6874787034908));
#101687=CARTESIAN_POINT('Ctrl Pts',(1.87769657750741,-2.26486634546433,
20.6824380775537));
#101688=CARTESIAN_POINT('Ctrl Pts',(1.80588114163647,-2.32440522219192,
20.6773943541484));
#101689=CARTESIAN_POINT('Ctrl Pts',(1.73129814356105,-2.38046948745456,
20.6723506307431));
#101690=CARTESIAN_POINT('Ctrl Pts',(1.6543264659011,-2.43281070866995,20.6673069073377));
#101691=CARTESIAN_POINT('Ctrl Pts',(1.57723022010592,-2.48523663699477,
20.6622550213557));
#101692=CARTESIAN_POINT('Ctrl Pts',(1.49773795559287,-2.53392726090745,
20.6572031353737));
#101693=CARTESIAN_POINT('Ctrl Pts',(1.4162542918173,-2.57867946455334,20.6521512493917));
#101694=CARTESIAN_POINT('Ctrl Pts',(1.37512574490992,-2.60126795679305,
20.6496013305497));
#101695=CARTESIAN_POINT('Ctrl Pts',(1.33349019287243,-2.62285381878076,
20.6470514117076));
#101696=CARTESIAN_POINT('Ctrl Pts',(1.2914014689021,-2.6434156400607,20.6445014928655));
#101697=CARTESIAN_POINT('Ctrl Pts',(1.20800776383333,-2.68415639667532,
20.6394491377499));
#101698=CARTESIAN_POINT('Ctrl Pts',(1.12253461990779,-2.72102006398541,
20.6343967826342));
#101699=CARTESIAN_POINT('Ctrl Pts',(1.03537774009605,-2.7537895590102,20.6293444275185));
#101700=CARTESIAN_POINT('Ctrl Pts',(0.948341036332749,-2.78651386989772,
20.6242990388302));
#101701=CARTESIAN_POINT('Ctrl Pts',(0.859625622245854,-2.81515507133425,
20.6192536501419));
#101702=CARTESIAN_POINT('Ctrl Pts',(0.769650435297222,-2.8395426053234,
20.6142082614536));
#101703=CARTESIAN_POINT('Ctrl Pts',(0.679771512067372,-2.86390404728881,
20.6091682707855));
#101704=CARTESIAN_POINT('Ctrl Pts',(0.588635921442568,-2.88402075195228,
20.6041282801174));
#101705=CARTESIAN_POINT('Ctrl Pts',(0.496680117319169,-2.89977117391352,
20.5990882894493));
#101706=CARTESIAN_POINT('Ctrl Pts',(0.404790569221353,-2.91551024737567,
20.5940519301969));
#101707=CARTESIAN_POINT('Ctrl Pts',(0.312082418887491,-2.92688921646361,
20.5890155709445));
#101708=CARTESIAN_POINT('Ctrl Pts',(0.219003712426472,-2.93383731211249,
20.5839792116921));
#101709=CARTESIAN_POINT('Ctrl Pts',(0.125958831554236,-2.94078288276467,
20.5789446826952));
#101710=CARTESIAN_POINT('Ctrl Pts',(0.032544104639384,-2.94330074581374,
20.5739101536984));
#101711=CARTESIAN_POINT('Ctrl Pts',(-0.0607869127297559,-2.94137195050894,
20.5688756247015));
#101712=CARTESIAN_POINT('Ctrl Pts',(-0.154110119414693,-2.93944331662113,
20.5638415170342));
#101713=CARTESIAN_POINT('Ctrl Pts',(-0.247349186341164,-2.93306877362979,
20.5588074093669));
#101714=CARTESIAN_POINT('Ctrl Pts',(-0.340051318546357,-2.92228148896626,
20.5537733016995));
#101715=CARTESIAN_POINT('Ctrl Pts',(-0.432771623061142,-2.91149208968173,
20.548738207201));
#101716=CARTESIAN_POINT('Ctrl Pts',(-0.524954342625254,-2.89628828249211,
20.5437031127024));
#101717=CARTESIAN_POINT('Ctrl Pts',(-0.616153702080383,-2.87675487579541,
20.5386680182038));
#101718=CARTESIAN_POINT('Ctrl Pts',(-0.707453252544559,-2.85720000982817,
20.5336273921839));
#101719=CARTESIAN_POINT('Ctrl Pts',(-0.797766851411304,-2.83330614307377,
20.528586766164));
#101720=CARTESIAN_POINT('Ctrl Pts',(-0.886661091238355,-2.8052087461157,
20.5235461401442));
#101721=CARTESIAN_POINT('Ctrl Pts',(-0.975609956645429,-2.77709408328519,
20.5185024166557));
#101722=CARTESIAN_POINT('Ctrl Pts',(-1.06313731021647,-2.74477090163821,
20.5134586931671));
#101723=CARTESIAN_POINT('Ctrl Pts',(-1.14882908750468,-2.7084231072163,
20.5084149696786));
#101724=CARTESIAN_POINT('Ctrl Pts',(-1.23465954521045,-2.67201648886205,
20.5033630836137));
#101725=CARTESIAN_POINT('Ctrl Pts',(-1.31864809640367,-2.63157244728363,
20.4983111975488));
#101726=CARTESIAN_POINT('Ctrl Pts',(-1.40040482739467,-2.58732107002778,
20.4932593114839));
#101727=CARTESIAN_POINT('Ctrl Pts',(-1.44167119011148,-2.56498537530976,
20.4907093934498));
#101728=CARTESIAN_POINT('Ctrl Pts',(-1.48236940596208,-2.54168038747084,
20.4881594754158));
#101729=CARTESIAN_POINT('Ctrl Pts',(-1.52245231683729,-2.51743975954873,
20.4856095573817));
#101730=CARTESIAN_POINT('Ctrl Pts',(-1.60187177098416,-2.46940987859161,
20.4805572023017));
#101731=CARTESIAN_POINT('Ctrl Pts',(-1.67915864883517,-2.41753188053811,
20.4755048472216));
#101732=CARTESIAN_POINT('Ctrl Pts',(-1.75391612625696,-2.36202079204561,
20.4704524921416));
#101733=CARTESIAN_POINT('Ctrl Pts',(-1.82857052450901,-2.30658624488531,
20.4654071034893));
#101734=CARTESIAN_POINT('Ctrl Pts',(-1.90070209918824,-2.2475288243089,
20.460361714837));
#101735=CARTESIAN_POINT('Ctrl Pts',(-1.96994054805034,-2.18510828956991,
20.4553163261848));
#101736=CARTESIAN_POINT('Ctrl Pts',(-2.03910491925542,-2.1227545380567,
20.450276335553));
#101737=CARTESIAN_POINT('Ctrl Pts',(-2.10538198891141,-2.05704512015461,
20.4452363449213));
#101738=CARTESIAN_POINT('Ctrl Pts',(-2.1684331651186,-1.98828106876612,
20.4401963542896));
#101739=CARTESIAN_POINT('Ctrl Pts',(-2.23143891166714,-1.91956656327938,
20.4351599950739));
#101740=CARTESIAN_POINT('Ctrl Pts',(-2.29122308531933,-1.84780212544846,
20.4301236358583));
#101741=CARTESIAN_POINT('Ctrl Pts',(-2.34748349618322,-1.7733260374639,
20.4250872766426));
#101742=CARTESIAN_POINT('Ctrl Pts',(-2.40372346153572,-1.69887701472258,
20.4200527476827));
#101743=CARTESIAN_POINT('Ctrl Pts',(-2.45644194058178,-1.62171865361694,
20.4150182187228));
#101744=CARTESIAN_POINT('Ctrl Pts',(-2.50537731626918,-1.54222193705181,
20.4099836897629));
#101745=CARTESIAN_POINT('Ctrl Pts',(-2.55430859665226,-1.46273187340888,
20.4049495821327));
#101746=CARTESIAN_POINT('Ctrl Pts',(-2.59945717043663,-1.38090422179658,
20.3999154745025));
#101747=CARTESIAN_POINT('Ctrl Pts',(-2.64060564193848,-1.29713755776428,
20.3948813668723));
#101748=CARTESIAN_POINT('Ctrl Pts',(-2.68176217973455,-1.21335447303556,
20.3898462724109));
#101749=CARTESIAN_POINT('Ctrl Pts',(-2.71891686242717,-1.12763201986958,
20.3848111779496));
#101750=CARTESIAN_POINT('Ctrl Pts',(-2.75189950511258,-1.04039084663465,
20.3797760834882));
#101751=CARTESIAN_POINT('Ctrl Pts',(-2.78491838231024,-0.953053830826071,
20.3747354575055));
#101752=CARTESIAN_POINT('Ctrl Pts',(-2.81375591321227,-0.864195180694685,
20.3696948315229));
#101753=CARTESIAN_POINT('Ctrl Pts',(-2.83829119787571,-0.77425259189832,
20.3646542055402));
#101754=CARTESIAN_POINT('Ctrl Pts',(-2.86284155949075,-0.68425473331088,
20.3596104820889));
#101755=CARTESIAN_POINT('Ctrl Pts',(-2.88308431540144,-0.593172043357264,
20.3545667586376));
#101756=CARTESIAN_POINT('Ctrl Pts',(-2.89894975734376,-0.50145219552474,
20.3495230351863));
#101757=CARTESIAN_POINT('Ctrl Pts',(-2.9148408753344,-0.409583911660327,
20.3444711491583));
#101758=CARTESIAN_POINT('Ctrl Pts',(-2.926340482152,-0.317076851642814,
20.3394192631303));
#101759=CARTESIAN_POINT('Ctrl Pts',(-2.93343077091723,-0.224383404546675,
20.3343673771022));
#101760=CARTESIAN_POINT('Ctrl Pts',(-2.9370095645982,-0.177596773745147,
20.3318174587008));
#101761=CARTESIAN_POINT('Ctrl Pts',(-2.9394658317974,-0.130762655653171,
20.3292675402993));
#101762=CARTESIAN_POINT('Ctrl Pts',(-2.94080231530881,-0.0839389199023072,
20.3267176218979));
#101763=CARTESIAN_POINT('Ctrl Pts',(-2.94159575851465,-0.0561406158553956,
20.3252037869618));
#101764=CARTESIAN_POINT('Ctrl Pts',(-2.94199506204502,-0.0283310083262269,
20.3236899520257));
#101765=CARTESIAN_POINT('Ctrl Pts',(-2.94199995448524,-0.000517502503631551,
20.3221761170896));
#101766=CARTESIAN_POINT('',(-2.94199904186917,-0.0023743716766289,19.3221761171224));
#101767=CARTESIAN_POINT('Ctrl Pts',(-2.94199995448535,-0.000517501908740767,
20.3221761170572));
#101768=CARTESIAN_POINT('Ctrl Pts',(-2.94201620488574,0.0918660746620151,
20.3171478589648));
#101769=CARTESIAN_POINT('Ctrl Pts',(-2.9376766891411,0.184422648897923,
20.3121196008723));
#101770=CARTESIAN_POINT('Ctrl Pts',(-2.92895857371174,0.276705029734675,
20.3070913427799));
#101771=CARTESIAN_POINT('Ctrl Pts',(-2.92025239438784,0.368861065349422,
20.3020699689526));
#101772=CARTESIAN_POINT('Ctrl Pts',(-2.90717956698,0.460743210390338,20.2970485951254));
#101773=CARTESIAN_POINT('Ctrl Pts',(-2.88976926150288,0.551903628610208,
20.2920272212981));
#101774=CARTESIAN_POINT('Ctrl Pts',(-2.87182607555534,0.64585421077106,
20.2868521573446));
#101775=CARTESIAN_POINT('Ctrl Pts',(-2.84927557040695,0.739037686100096,
20.2816770933911));
#101776=CARTESIAN_POINT('Ctrl Pts',(-2.82220749584933,0.830968621773331,
20.2765020294376));
#101777=CARTESIAN_POINT('Ctrl Pts',(-2.79598934880378,0.920012960127909,
20.2714894605748));
#101778=CARTESIAN_POINT('Ctrl Pts',(-2.76553324655604,1.00788178111871,
20.266476891712));
#101779=CARTESIAN_POINT('Ctrl Pts',(-2.7309724190848,1.09414516687601,20.2614643228493));
#101780=CARTESIAN_POINT('Ctrl Pts',(-2.69642279554893,1.18038058775313,
20.256453378962));
#101781=CARTESIAN_POINT('Ctrl Pts',(-2.65777125670995,1.26501119075463,
20.2514424350747));
#101782=CARTESIAN_POINT('Ctrl Pts',(-2.61519994227204,1.34762504501079,
20.2464314911874));
#101783=CARTESIAN_POINT('Ctrl Pts',(-2.57263022705451,1.43023579582132,
20.2414207355396));
#101784=CARTESIAN_POINT('Ctrl Pts',(-2.52614123529246,1.51082954974157,
20.2364099798918));
#101785=CARTESIAN_POINT('Ctrl Pts',(-2.47596147827404,1.58901817425196,
20.231399224244));
#101786=CARTESIAN_POINT('Ctrl Pts',(-2.42576922385174,1.66722627185024,
20.226387220654));
#101787=CARTESIAN_POINT('Ctrl Pts',(-2.37188462195081,1.74302767324794,
20.221375217064));
#101788=CARTESIAN_POINT('Ctrl Pts',(-2.31457931158189,1.81606349294212,
20.216363213474));
#101789=CARTESIAN_POINT('Ctrl Pts',(-2.25720983495547,1.88918109275723,
20.2113455978123));
#101790=CARTESIAN_POINT('Ctrl Pts',(-2.19641228545946,1.95952657909388,
20.2063279821506));
#101791=CARTESIAN_POINT('Ctrl Pts',(-2.13249808730623,2.02677475503206,
20.2013103664888));
#101792=CARTESIAN_POINT('Ctrl Pts',(-2.06854077114854,2.09406829815366,
20.1962893658269));
#101793=CARTESIAN_POINT('Ctrl Pts',(-2.00146294661669,2.15826006370198,
20.1912683651649));
#101794=CARTESIAN_POINT('Ctrl Pts',(-1.9316107009224,2.21906378909712,20.186247364503));
#101795=CARTESIAN_POINT('Ctrl Pts',(-1.86165120023888,2.27996087588454,
20.1812186543198));
#101796=CARTESIAN_POINT('Ctrl Pts',(-1.78890913164896,2.33745926826067,
20.1761899441366));
#101797=CARTESIAN_POINT('Ctrl Pts',(-1.71376084649715,2.39131506937362,
20.1711612339534));
#101798=CARTESIAN_POINT('Ctrl Pts',(-1.6971455403518,2.40322260154667,20.1700493847736));
#101799=CARTESIAN_POINT('Ctrl Pts',(-1.68041270353207,2.41495224119587,
20.1689375355938));
#101800=CARTESIAN_POINT('Ctrl Pts',(-1.66356656305616,2.42650165676463,
20.167825686414));
#101801=CARTESIAN_POINT('Ctrl Pts',(-1.58701599746003,2.47898336884331,
20.1627733313245));
#101802=CARTESIAN_POINT('Ctrl Pts',(-1.50784212642289,2.52793320386305,
20.157720976235));
#101803=CARTESIAN_POINT('Ctrl Pts',(-1.42640471145188,2.57307862280729,
20.1526686211455));
#101804=CARTESIAN_POINT('Ctrl Pts',(-1.3450795862654,2.61816179309878,20.1476232324837));
#101805=CARTESIAN_POINT('Ctrl Pts',(-1.2614975043014,2.6594507577,20.1425778438219));
#101806=CARTESIAN_POINT('Ctrl Pts',(-1.17604800636927,2.69671561101924,
20.1375324551601));
#101807=CARTESIAN_POINT('Ctrl Pts',(-1.09068993016381,2.73394059497333,
20.1324924645189));
#101808=CARTESIAN_POINT('Ctrl Pts',(-1.00346881420423,2.76714984858702,
20.1274524738776));
#101809=CARTESIAN_POINT('Ctrl Pts',(-0.91479868509532,2.79615939562606,
20.1224124832364));
#101810=CARTESIAN_POINT('Ctrl Pts',(-0.826192444622468,2.82514804069493,
20.1173761240111));
#101811=CARTESIAN_POINT('Ctrl Pts',(-0.736139687189324,2.84994285600389,
20.1123397647859));
#101812=CARTESIAN_POINT('Ctrl Pts',(-0.64507332202963,2.87040840460128,
20.1073034055606));
#101813=CARTESIAN_POINT('Ctrl Pts',(-0.554040051160576,2.89086651584447,
20.1022688765911));
#101814=CARTESIAN_POINT('Ctrl Pts',(-0.461994337333051,2.9069983885859,
20.0972343476216));
#101815=CARTESIAN_POINT('Ctrl Pts',(-0.369382107035341,2.91871904420452,
20.0921998186521));
#101816=CARTESIAN_POINT('Ctrl Pts',(-0.276777627271035,2.93043871894477,
20.0871657110123));
#101817=CARTESIAN_POINT('Ctrl Pts',(-0.183607166047962,2.93774785495905,
20.0821316033725));
#101818=CARTESIAN_POINT('Ctrl Pts',(-0.0903235080035432,2.94061314421022,
20.0770974957327));
#101819=CARTESIAN_POINT('Ctrl Pts',(0.00297843634419862,2.94347899514122,
20.0720624012618));
#101820=CARTESIAN_POINT('Ctrl Pts',(0.0963931775675672,2.94189925598673,
20.0670273067909));
#101821=CARTESIAN_POINT('Ctrl Pts',(0.189467334651144,2.93589273119782,
20.0619922123199));
#101822=CARTESIAN_POINT('Ctrl Pts',(0.282643742384046,2.92987960768076,
20.0569515863277));
#101823=CARTESIAN_POINT('Ctrl Pts',(0.375478375100996,2.91943001959899,
20.0519109603355));
#101824=CARTESIAN_POINT('Ctrl Pts',(0.467522688922141,2.90461469653774,
20.0468703343433));
#101825=CARTESIAN_POINT('Ctrl Pts',(0.559623564045482,2.88979026944898,
20.0418266108825));
#101826=CARTESIAN_POINT('Ctrl Pts',(0.650932719021392,2.87059485787772,
20.0367828874217));
#101827=CARTESIAN_POINT('Ctrl Pts',(0.741013672775681,2.84714993225849,
20.031739163961));
#101828=CARTESIAN_POINT('Ctrl Pts',(0.831240410233106,2.82366706423374,
20.0266872779236));
#101829=CARTESIAN_POINT('Ctrl Pts',(0.920234554756113,2.79592108465082,
20.0216353918862));
#101830=CARTESIAN_POINT('Ctrl Pts',(1.00757677343834,2.7640826770608,20.0165835058489));
#101831=CARTESIAN_POINT('Ctrl Pts',(1.05166239229028,2.748012374256,20.0140335875426));
#101832=CARTESIAN_POINT('Ctrl Pts',(1.0953274965222,2.73090020389196,20.0114836692364));
#101833=CARTESIAN_POINT('Ctrl Pts',(1.13852051928327,2.71277257195861,20.0089337509301));
#101834=CARTESIAN_POINT('Ctrl Pts',(1.22410227600109,2.67685485917033,20.0038813958462));
#101835=CARTESIAN_POINT('Ctrl Pts',(1.30813624208454,2.63681886627311,19.9988290407623));
#101836=CARTESIAN_POINT('Ctrl Pts',(1.39019844753919,2.59281936826683,19.9937766856784));
#101837=CARTESIAN_POINT('Ctrl Pts',(1.47214750171708,2.5488805388637,19.9887312970223));
#101838=CARTESIAN_POINT('Ctrl Pts',(1.55212980967024,2.50098927224878,19.9836859083661));
#101839=CARTESIAN_POINT('Ctrl Pts',(1.629741106866,2.44934846940797,19.97864051971));
#101840=CARTESIAN_POINT('Ctrl Pts',(1.70726936836178,2.39776291664501,19.9736005290745));
#101841=CARTESIAN_POINT('Ctrl Pts',(1.78243129336603,2.34243604609097,19.9685605384389));
#101842=CARTESIAN_POINT('Ctrl Pts',(1.85484796074386,2.28361622049861,19.9635205478034));
#101843=CARTESIAN_POINT('Ctrl Pts',(1.92721245043526,2.22483877579073,19.9584841885839));
#101844=CARTESIAN_POINT('Ctrl Pts',(1.99683527024948,2.16257365770787,19.9534478293644));
#101845=CARTESIAN_POINT('Ctrl Pts',(2.06336807148347,2.09711139465279,19.948411470145));
#101846=CARTESIAN_POINT('Ctrl Pts',(2.12987669413183,2.03167292114067,19.9433769411813));
#101847=CARTESIAN_POINT('Ctrl Pts',(2.19329721269772,1.963039922091,19.9383424122176));
#101848=CARTESIAN_POINT('Ctrl Pts',(2.25331664124461,1.89154120079106,19.9333078832539));
#101849=CARTESIAN_POINT('Ctrl Pts',(2.31333104688447,1.82004846307742,19.9282737756199));
#101850=CARTESIAN_POINT('Ctrl Pts',(2.36994464293867,1.74569082031407,19.923239667986));
#101851=CARTESIAN_POINT('Ctrl Pts',(2.4228841615683,1.66883083013871,19.918205560352));
#101852=CARTESIAN_POINT('Ctrl Pts',(2.47583405787918,1.59195577317584,19.9131704658869));
#101853=CARTESIAN_POINT('Ctrl Pts',(2.52510819472144,1.51257776064216,19.9081353714219));
#101854=CARTESIAN_POINT('Ctrl Pts',(2.57047678576047,1.43108808040125,19.9031002769568));
#101855=CARTESIAN_POINT('Ctrl Pts',(2.61589521843168,1.34950887613994,19.8980596509705));
#101856=CARTESIAN_POINT('Ctrl Pts',(2.6573993243255,1.2658137621942,19.8930190249841));
#101857=CARTESIAN_POINT('Ctrl Pts',(2.69480558441763,1.18041808787886,19.8879783989978));
#101858=CARTESIAN_POINT('Ctrl Pts',(2.73223483068551,1.09496993785559,19.8829346755429));
#101859=CARTESIAN_POINT('Ctrl Pts',(2.7655610594934,1.00781956170815,19.877890952088));
#101860=CARTESIAN_POINT('Ctrl Pts',(2.79464993773324,0.919399654952938,
19.872847228633));
#101861=CARTESIAN_POINT('Ctrl Pts',(2.82378589234436,0.830836652670853,
19.8677953426015));
#101862=CARTESIAN_POINT('Ctrl Pts',(2.84867068767718,0.741000445689483,
19.86274345657));
#101863=CARTESIAN_POINT('Ctrl Pts',(2.86922064706356,0.650335973527639,
19.8576915705384));
#101864=CARTESIAN_POINT('Ctrl Pts',(2.8795931531915,0.604573460064577,19.8551416521744));
#101865=CARTESIAN_POINT('Ctrl Pts',(2.88886209993438,0.558600050050892,
19.8525917338103));
#101866=CARTESIAN_POINT('Ctrl Pts',(2.8970217502022,0.512473393314626,19.8500418154463));
#101867=CARTESIAN_POINT('Ctrl Pts',(2.91318911112535,0.421078997334762,
19.844989460362));
#101868=CARTESIAN_POINT('Ctrl Pts',(2.92505631463085,0.328754798638797,
19.8399371052778));
#101869=CARTESIAN_POINT('Ctrl Pts',(2.93252379981452,0.23594101703904,19.8348847501935));
#101870=CARTESIAN_POINT('Ctrl Pts',(2.93998098847401,0.143255211501282,
19.8298393615371));
#101871=CARTESIAN_POINT('Ctrl Pts',(2.94305047849443,0.0500816034598757,
19.8247939728806));
#101872=CARTESIAN_POINT('Ctrl Pts',(2.94168383686064,-0.0431300817628487,
19.8197485842242));
#101873=CARTESIAN_POINT('Ctrl Pts',(2.9403186573857,-0.136242040556156,
19.8147085935883));
#101874=CARTESIAN_POINT('Ctrl Pts',(2.93452678649661,-0.229391553749678,
19.8096686029524));
#101875=CARTESIAN_POINT('Ctrl Pts',(2.92431173361142,-0.322125572816807,
19.8046286123166));
#101876=CARTESIAN_POINT('Ctrl Pts',(2.91410404088029,-0.414792775130863,
19.7995922530968));
#101877=CARTESIAN_POINT('Ctrl Pts',(2.89947954925317,-0.507044638062517,
19.794555893877));
#101878=CARTESIAN_POINT('Ctrl Pts',(2.88049377246798,-0.598430970767051,
19.7895195346573));
#101879=CARTESIAN_POINT('Ctrl Pts',(2.86151489527552,-0.689784092901165,
19.7844850056933));
#101880=CARTESIAN_POINT('Ctrl Pts',(2.83817797182982,-0.780271875163795,
19.7794504767293));
#101881=CARTESIAN_POINT('Ctrl Pts',(2.81058984458734,-0.869453118634081,
19.7744159477653));
#101882=CARTESIAN_POINT('Ctrl Pts',(2.7830040261406,-0.95862689870266,19.769381840131));
#101883=CARTESIAN_POINT('Ctrl Pts',(2.75116784272559,-1.04649393303362,
19.7643477324968));
#101884=CARTESIAN_POINT('Ctrl Pts',(2.71523802490897,-1.13262812435877,
19.7593136248626));
#101885=CARTESIAN_POINT('Ctrl Pts',(2.67930116380589,-1.21877920048377,
19.7542785303972));
#101886=CARTESIAN_POINT('Ctrl Pts',(2.6392692459469,-1.30319634915029,19.7492434359319));
#101887=CARTESIAN_POINT('Ctrl Pts',(2.59534670545318,-1.38547445970445,
19.7442083414665));
#101888=CARTESIAN_POINT('Ctrl Pts',(2.551375911949,-1.46784296044286,19.7391677154799));
#101889=CARTESIAN_POINT('Ctrl Pts',(2.50350617351727,-1.54806733982987,
19.7341270894933));
#101890=CARTESIAN_POINT('Ctrl Pts',(2.45198721241842,-1.62576834454868,
19.7290864635067));
#101891=CARTESIAN_POINT('Ctrl Pts',(2.40043659287825,-1.7035170965948,19.7240427400516));
#101892=CARTESIAN_POINT('Ctrl Pts',(2.34523254902948,-1.77873902912197,
19.7189990165964));
#101893=CARTESIAN_POINT('Ctrl Pts',(2.28666602757342,-1.8510868370613,19.7139552931413));
#101894=CARTESIAN_POINT('Ctrl Pts',(2.22800472421211,-1.92355173003328,
19.7089034071095));
#101895=CARTESIAN_POINT('Ctrl Pts',(2.16597037481727,-1.99313288135999,
19.7038515210777));
#101896=CARTESIAN_POINT('Ctrl Pts',(2.10089165831102,-2.05951893412981,
19.698799635046));
#101897=CARTESIAN_POINT('Ctrl Pts',(2.06804344813789,-2.09302701681822,
19.6962497166848));
#101898=CARTESIAN_POINT('Ctrl Pts',(2.03442017375972,-2.12572171390069,
19.6936997983236));
#101899=CARTESIAN_POINT('Ctrl Pts',(2.00006718655783,-2.15756697445401,
19.6911498799624));
#101900=CARTESIAN_POINT('Ctrl Pts',(1.93200089383406,-2.22066450987208,
19.6860975248768));
#101901=CARTESIAN_POINT('Ctrl Pts',(1.86082366896969,-2.28065109878669,
19.6810451697912));
#101902=CARTESIAN_POINT('Ctrl Pts',(1.78685161924509,-2.33720458899113,
19.6759928147056));
#101903=CARTESIAN_POINT('Ctrl Pts',(1.7129815657048,-2.39368010055051,19.6709474260478));
#101904=CARTESIAN_POINT('Ctrl Pts',(1.63632469483503,-2.44673165243948,
19.66590203739));
#101905=CARTESIAN_POINT('Ctrl Pts',(1.55723279960355,-2.49607492031768,
19.6608566487321));
#101906=CARTESIAN_POINT('Ctrl Pts',(1.47822552415187,-2.54536539623216,
19.6558166580949));
#101907=CARTESIAN_POINT('Ctrl Pts',(1.39678877747987,-2.59095524019785,
19.6507766674576));
#101908=CARTESIAN_POINT('Ctrl Pts',(1.31330528277103,-2.63260198933407,
19.6457366768203));
#101909=CARTESIAN_POINT('Ctrl Pts',(1.22988193962321,-2.67421873113793,
19.6407003175992));
#101910=CARTESIAN_POINT('Ctrl Pts',(1.14441517603931,-2.71189782742285,
19.635663958378));
#101911=CARTESIAN_POINT('Ctrl Pts',(1.05731348343144,-2.74544207692569,
19.6306275991568));
#101912=CARTESIAN_POINT('Ctrl Pts',(0.97024344431919,-2.77897413616308,
19.6255930701913));
#101913=CARTESIAN_POINT('Ctrl Pts',(0.881540070663633,-2.80837417428135,
19.6205585412259));
#101914=CARTESIAN_POINT('Ctrl Pts',(0.791632099835083,-2.83349300661052,
19.6155240122605));
#101915=CARTESIAN_POINT('Ctrl Pts',(0.701731653226236,-2.85860973679444,
19.6104899046248));
#101916=CARTESIAN_POINT('Ctrl Pts',(0.610627237784615,-2.87944585418853,
19.6054557969891));
#101917=CARTESIAN_POINT('Ctrl Pts',(0.518761920775194,-2.89590228936572,
19.6004216893534));
#101918=CARTESIAN_POINT('Ctrl Pts',(0.426878595499444,-2.91236195048146,
19.5953865948866));
#101919=CARTESIAN_POINT('Ctrl Pts',(0.334234509743728,-2.92444014634262,
19.5903515004198));
#101920=CARTESIAN_POINT('Ctrl Pts',(0.241280930547855,-2.93208927431515,
19.5853164059531));
#101921=CARTESIAN_POINT('Ctrl Pts',(0.148225233168343,-2.93974680556879,
19.580275779965));
#101922=CARTESIAN_POINT('Ctrl Pts',(0.0548598070819101,-2.9429655198555,
19.5752351539769));
#101923=CARTESIAN_POINT('Ctrl Pts',(-0.0383612835256337,-2.94174988942403,
19.5701945279889));
#101924=CARTESIAN_POINT('Ctrl Pts',(-0.131639658565474,-2.94053351198671,
19.5651508045322));
#101925=CARTESIAN_POINT('Ctrl Pts',(-0.224773078460283,-2.93487739197961,
19.5601070810756));
#101926=CARTESIAN_POINT('Ctrl Pts',(-0.317312003031018,-2.92483796008128,
19.555063357619));
#101927=CARTESIAN_POINT('Ctrl Pts',(-0.410000689195166,-2.91478228073546,
19.5500114715857));
#101928=CARTESIAN_POINT('Ctrl Pts',(-0.502092520991421,-2.90032919643848,
19.5449595855525));
#101929=CARTESIAN_POINT('Ctrl Pts',(-0.593147736187301,-2.88158632753834,
19.5399076995192));
#101930=CARTESIAN_POINT('Ctrl Pts',(-0.639107475240012,-2.87212594284871,
19.5373577811723));
#101931=CARTESIAN_POINT('Ctrl Pts',(-0.684803347257254,-2.86157345247506,
19.5348078628254));
#101932=CARTESIAN_POINT('Ctrl Pts',(-0.730180482178185,-2.84994744924289,
19.5322579444784));
#101933=CARTESIAN_POINT('Ctrl Pts',(-0.820089791871933,-2.82691192866796,
19.5272055893937));
#101934=CARTESIAN_POINT('Ctrl Pts',(-0.909069278997653,-2.79957625496688,
19.522153234309));
#101935=CARTESIAN_POINT('Ctrl Pts',(-0.996676917005936,-2.76803163332855,
19.5171008792243));
#101936=CARTESIAN_POINT('Ctrl Pts',(-1.08416375743151,-2.73653050691653,
19.5120554905673));
#101937=CARTESIAN_POINT('Ctrl Pts',(-1.17028209318973,-2.70083211405906,
19.5070101019103));
#101938=CARTESIAN_POINT('Ctrl Pts',(-1.25460236430888,-2.66107814756925,
19.5019647132533));
#101939=CARTESIAN_POINT('Ctrl Pts',(-1.33883242185103,-2.62136671352708,
19.4969247226169));
#101940=CARTESIAN_POINT('Ctrl Pts',(-1.42126783880829,-2.57760851875703,
19.4918847319805));
#101941=CARTESIAN_POINT('Ctrl Pts',(-1.5014974883339,-2.52999393132217,
19.4868447413441));
#101942=CARTESIAN_POINT('Ctrl Pts',(-1.58166933075983,-2.48241365116919,
19.4818083821238));
#101943=CARTESIAN_POINT('Ctrl Pts',(-1.65963818378397,-2.43098272730459,
19.4767720229035));
#101944=CARTESIAN_POINT('Ctrl Pts',(-1.7350170079866,-2.37593770583263,
19.4717356636832));
#101945=CARTESIAN_POINT('Ctrl Pts',(-1.81036843888357,-2.32091268818953,
19.4667011347187));
#101946=CARTESIAN_POINT('Ctrl Pts',(-1.88313135242865,-2.26227644386214,
19.4616666057541));
#101947=CARTESIAN_POINT('Ctrl Pts',(-1.95294810376865,-2.20030854745111,
19.4566320767896));
#101948=CARTESIAN_POINT('Ctrl Pts',(-2.02275901228322,-2.13834583701042,
19.4515979691548));
#101949=CARTESIAN_POINT('Ctrl Pts',(-2.0896239166873,-2.07305232387743,
19.44656386152));
#101950=CARTESIAN_POINT('Ctrl Pts',(-2.15321953545585,-2.00474677506444,
19.4415297538852));
#101951=CARTESIAN_POINT('Ctrl Pts',(-2.21682762081048,-1.93642783638246,
19.4364946594193));
#101952=CARTESIAN_POINT('Ctrl Pts',(-2.27716484532294,-1.86509601475816,
19.4314595649534));
#101953=CARTESIAN_POINT('Ctrl Pts',(-2.33394674751587,-1.79110484890195,
19.4264244704875));
#101954=CARTESIAN_POINT('Ctrl Pts',(-2.39079102992836,-1.71703239684375,
19.4213838445003));
#101955=CARTESIAN_POINT('Ctrl Pts',(-2.44407192261281,-1.64029512179496,
19.4163432185131));
#101956=CARTESIAN_POINT('Ctrl Pts',(-2.49354722184721,-1.56127712223617,
19.411302592526));
#101957=CARTESIAN_POINT('Ctrl Pts',(-2.54305292369132,-1.48221056605544,
19.4062588690702));
#101958=CARTESIAN_POINT('Ctrl Pts',(-2.58874815910735,-1.40086088226812,
19.4012151456145));
#101959=CARTESIAN_POINT('Ctrl Pts',(-2.6304368500518,-1.31763651205086,
19.3961714221588));
#101960=CARTESIAN_POINT('Ctrl Pts',(-2.67219300844091,-1.23427745457275,
19.3911195361264));
#101961=CARTESIAN_POINT('Ctrl Pts',(-2.70992949818134,-1.14903805952311,
19.3860676500941));
#101962=CARTESIAN_POINT('Ctrl Pts',(-2.74349856672358,-1.06234627800245,
19.3810157640618));
#101963=CARTESIAN_POINT('Ctrl Pts',(-2.76044241373679,-1.01858896368972,
19.3784658457061));
#101964=CARTESIAN_POINT('Ctrl Pts',(-2.77632532715895,-0.974461864885243,
19.3759159273504));
#101965=CARTESIAN_POINT('Ctrl Pts',(-2.79113321301135,-0.930021175686314,
19.3733660089946));
#101966=CARTESIAN_POINT('Ctrl Pts',(-2.82599674499543,-0.825390480614395,
19.3673625078171));
#101967=CARTESIAN_POINT('Ctrl Pts',(-2.8550003049623,-0.718715539266835,
19.3613590066396));
#101968=CARTESIAN_POINT('Ctrl Pts',(-2.8779384302806,-0.610601663536891,
19.3553555054621));
#101969=CARTESIAN_POINT('Ctrl Pts',(-2.90063211165595,-0.503639921283632,
19.3494159815922));
#101970=CARTESIAN_POINT('Ctrl Pts',(-2.91738889183095,-0.395269828056337,
19.3434764577223));
#101971=CARTESIAN_POINT('Ctrl Pts',(-2.92805595837851,-0.286098417688969,
19.3375369338524));
#101972=CARTESIAN_POINT('Ctrl Pts',(-2.93725169291171,-0.191985260723234,
19.3324166616091));
#101973=CARTESIAN_POINT('Ctrl Pts',(-2.9419224497351,-0.0972769462315368,
19.3272963893658));
#101974=CARTESIAN_POINT('Ctrl Pts',(-2.94199904186917,-0.00237437167659856,
19.3221761171224));
#101975=CARTESIAN_POINT('',(-2.94199948962717,0.00173292627207862,18.3221761170896));
#101976=CARTESIAN_POINT('Ctrl Pts',(-2.94199904186967,-0.00237437106792486,
19.3221761170896));
#101977=CARTESIAN_POINT('Ctrl Pts',(-2.94207416580396,0.0907090335007012,
19.3171539944026));
#101978=CARTESIAN_POINT('Ctrl Pts',(-2.93772732127096,0.183853550265652,
19.3121318717157));
#101979=CARTESIAN_POINT('Ctrl Pts',(-2.92896782757791,0.276607058864309,
19.3071097490287));
#101980=CARTESIAN_POINT('Ctrl Pts',(-2.92021036671541,0.369339041998981,
19.3020887918343));
#101981=CARTESIAN_POINT('Ctrl Pts',(-2.90704233305619,0.461679753029792,
19.2970678346399));
#101982=CARTESIAN_POINT('Ctrl Pts',(-2.88952502403285,0.553180924732574,
19.2920468774454));
#101983=CARTESIAN_POINT('Ctrl Pts',(-2.87200682498055,0.644686745476608,
19.2870256651435));
#101984=CARTESIAN_POINT('Ctrl Pts',(-2.85013899630507,0.735352503844594,
19.2820044528415));
#101985=CARTESIAN_POINT('Ctrl Pts',(-2.82403397171941,0.82474003575351,
19.2769832405396));
#101986=CARTESIAN_POINT('Ctrl Pts',(-2.79695214293673,0.917472292201672,
19.2717741432872));
#101987=CARTESIAN_POINT('Ctrl Pts',(-2.76530992063666,1.00882828203394,
19.2665650460348));
#101988=CARTESIAN_POINT('Ctrl Pts',(-2.72928894331806,1.09833777312891,
19.2613559487824));
#101989=CARTESIAN_POINT('Ctrl Pts',(-2.69451270762369,1.18475417243064,
19.2563268572005));
#101990=CARTESIAN_POINT('Ctrl Pts',(-2.65565561648089,1.26944920412853,
19.2512977656186));
#101991=CARTESIAN_POINT('Ctrl Pts',(-2.61292887903296,1.35202317772869,
19.2462686740367));
#101992=CARTESIAN_POINT('Ctrl Pts',(-2.57017004308213,1.4346591851065,19.2412358043449));
#101993=CARTESIAN_POINT('Ctrl Pts',(-2.5235359999055,1.51517057890675,19.2362029346531));
#101994=CARTESIAN_POINT('Ctrl Pts',(-2.47328191787931,1.59318566234172,
19.2311700649612));
#101995=CARTESIAN_POINT('Ctrl Pts',(-2.4229493979775,1.67132251374389,19.2261293398358));
#101996=CARTESIAN_POINT('Ctrl Pts',(-2.36898582885025,1.74695492290091,
19.2210886147103));
#101997=CARTESIAN_POINT('Ctrl Pts',(-2.3116870171327,1.8197437003106,19.2160478895848));
#101998=CARTESIAN_POINT('Ctrl Pts',(-2.30572373548415,1.82731907521868,
19.2155232842268));
#101999=CARTESIAN_POINT('Ctrl Pts',(-2.29972436162034,1.83486368309387,
19.2149986788688));
#102000=CARTESIAN_POINT('Ctrl Pts',(-2.29368925134959,1.84237716503526,
19.2144740735107));
#102001=CARTESIAN_POINT('Ctrl Pts',(-2.23556647467933,1.91473780358269,
19.2094217184257));
#102002=CARTESIAN_POINT('Ctrl Pts',(-2.17391183306994,1.98447512038605,
19.2043693633407));
#102003=CARTESIAN_POINT('Ctrl Pts',(-2.10899100269114,2.05122425652775,
19.1993170082556));
#102004=CARTESIAN_POINT('Ctrl Pts',(-2.04415968824456,2.11788135578218,
19.1942716195984));
#102005=CARTESIAN_POINT('Ctrl Pts',(-1.9760714412638,2.18155814614139,19.1892262309411));
#102006=CARTESIAN_POINT('Ctrl Pts',(-1.90503276494137,2.24192198002068,
19.1841808422839));
#102007=CARTESIAN_POINT('Ctrl Pts',(-1.83407009232494,2.30222123112167,
19.1791408516472));
#102008=CARTESIAN_POINT('Ctrl Pts',(-1.76016360138424,2.35921428487592,
19.1741008610105));
#102009=CARTESIAN_POINT('Ctrl Pts',(-1.68365650684848,2.41260538981135,
19.1690608703738));
#102010=CARTESIAN_POINT('Ctrl Pts',(-1.60720453723539,2.46595802536628,
19.1640245111532));
#102011=CARTESIAN_POINT('Ctrl Pts',(-1.52815605170076,2.5157136170833,19.1589881519326));
#102012=CARTESIAN_POINT('Ctrl Pts',(-1.44688636636842,2.56161742709898,
19.153951792712));
#102013=CARTESIAN_POINT('Ctrl Pts',(-1.36564621513072,2.60750455527981,
19.1489172637472));
#102014=CARTESIAN_POINT('Ctrl Pts',(-1.28218685410517,2.64954246429721,
19.1438827347823));
#102015=CARTESIAN_POINT('Ctrl Pts',(-1.19691064003318,2.68752096173692,
19.1388482058175));
#102016=CARTESIAN_POINT('Ctrl Pts',(-1.11164156255831,2.72549628083156,
19.1338140981824));
#102017=CARTESIAN_POINT('Ctrl Pts',(-1.0245563402353,2.75941268323711,19.1287799905473));
#102018=CARTESIAN_POINT('Ctrl Pts',(-0.936078824233458,2.7891074620426,
19.1237458829122));
#102019=CARTESIAN_POINT('Ctrl Pts',(-0.84758396407199,2.8188080618861,19.118710788446));
#102020=CARTESIAN_POINT('Ctrl Pts',(-0.757696689436905,2.84428525360216,
19.1136756939798));
#102021=CARTESIAN_POINT('Ctrl Pts',(-0.666856478877766,2.86542604800381,
19.1086405995136));
#102022=CARTESIAN_POINT('Ctrl Pts',(-0.57591647186845,2.88659006754136,
19.1035999735261));
#102023=CARTESIAN_POINT('Ctrl Pts',(-0.484021872569202,2.90340807954448,
19.0985593475386));
#102024=CARTESIAN_POINT('Ctrl Pts',(-0.391622530990364,2.91581820304708,
19.0935187215512));
#102025=CARTESIAN_POINT('Ctrl Pts',(-0.29916640994461,2.92823595258018,
19.0884749980952));
#102026=CARTESIAN_POINT('Ctrl Pts',(-0.206205371415175,2.93624038313473,
19.0834312746391));
#102027=CARTESIAN_POINT('Ctrl Pts',(-0.113192377192708,2.93982167584115,
19.0783875511831));
#102028=CARTESIAN_POINT('Ctrl Pts',(-0.0200288541598324,2.94340876438002,
19.0733356651505));
#102029=CARTESIAN_POINT('Ctrl Pts',(0.0731863487657453,2.94255842859601,
19.0682837791178));
#102030=CARTESIAN_POINT('Ctrl Pts',(0.166002467893603,2.93731291840914,
19.0632318930852));
#102031=CARTESIAN_POINT('Ctrl Pts',(0.212851015954096,2.93466526907409,
19.0606819747324));
#102032=CARTESIAN_POINT('Ctrl Pts',(0.259598001505305,2.93089868913091,
19.0581320563796));
#102033=CARTESIAN_POINT('Ctrl Pts',(0.306186427613535,2.92602355963606,
19.0555821380269));
#102034=CARTESIAN_POINT('Ctrl Pts',(0.398495764220038,2.91636407965072,
19.050529782942));
#102035=CARTESIAN_POINT('Ctrl Pts',(0.490513180381778,2.90231476261001,
19.0454774278571));
#102036=CARTESIAN_POINT('Ctrl Pts',(0.581788069406744,2.88390128858392,
19.0404250727722));
#102037=CARTESIAN_POINT('Ctrl Pts',(0.67293710426812,2.86551320393268,19.0353796841151));
#102038=CARTESIAN_POINT('Ctrl Pts',(0.763345214788649,2.84277300694814,
19.030334295458));
#102039=CARTESIAN_POINT('Ctrl Pts',(0.852566754704504,2.81575814458072,
19.0252889068009));
#102040=CARTESIAN_POINT('Ctrl Pts',(0.941692837215947,2.78877218519619,
19.0202489161644));
#102041=CARTESIAN_POINT('Ctrl Pts',(1.02963444955838,2.7575207788669,19.0152089255278));
#102042=CARTESIAN_POINT('Ctrl Pts',(1.11595707314046,2.72213221774913,19.0101689348913));
#102043=CARTESIAN_POINT('Ctrl Pts',(1.2022174995107,2.6867691548118,19.0051325756708));
#102044=CARTESIAN_POINT('Ctrl Pts',(1.28686084587408,2.64727503007975,19.0000962164504));
#102045=CARTESIAN_POINT('Ctrl Pts',(1.36946967966179,2.60382733615097,18.9950598572299));
#102046=CARTESIAN_POINT('Ctrl Pts',(1.45204849269696,2.56039543148355,18.9900253282652));
#102047=CARTESIAN_POINT('Ctrl Pts',(1.53259386919414,2.51301301848245,18.9849907993005));
#102048=CARTESIAN_POINT('Ctrl Pts',(1.61071117277391,2.46190444938493,18.9799562703358));
#102049=CARTESIAN_POINT('Ctrl Pts',(1.68882193887125,2.41080015746233,18.9749221627009));
#102050=CARTESIAN_POINT('Ctrl Pts',(1.76450466441769,2.35597057281577,18.969888055066));
#102051=CARTESIAN_POINT('Ctrl Pts',(1.83739298489219,2.29768383792657,18.964853947431));
#102052=CARTESIAN_POINT('Ctrl Pts',(1.91029559359169,2.23938567714668,18.959818852965));
#102053=CARTESIAN_POINT('Ctrl Pts',(1.98040236262021,2.17762929792242,18.9547837584989));
#102054=CARTESIAN_POINT('Ctrl Pts',(2.04738025380189,2.11272291045042,18.9497486640329));
#102055=CARTESIAN_POINT('Ctrl Pts',(2.114431726449,2.04774521725319,18.9447080380456));
#102056=CARTESIAN_POINT('Ctrl Pts',(2.17834714035993,1.9796109177247,18.9396674120583));
#102057=CARTESIAN_POINT('Ctrl Pts',(2.23883079961385,1.9086646249932,18.934626786071));
#102058=CARTESIAN_POINT('Ctrl Pts',(2.29935162612304,1.83767473571008,18.9295830626151));
#102059=CARTESIAN_POINT('Ctrl Pts',(2.35643622814713,1.76386976430429,18.9245393391592));
#102060=CARTESIAN_POINT('Ctrl Pts',(2.4098309863379,1.68762514122233,18.9194956157033));
#102061=CARTESIAN_POINT('Ctrl Pts',(2.46331215664244,1.61125712664527,18.9144437296709));
#102062=CARTESIAN_POINT('Ctrl Pts',(2.51309132483308,1.53244195335265,18.9093918436384));
#102063=CARTESIAN_POINT('Ctrl Pts',(2.55895983008073,1.45158140937158,18.9043399576059));
#102064=CARTESIAN_POINT('Ctrl Pts',(2.58211176634023,1.41076738785398,18.9017900392516));
#102065=CARTESIAN_POINT('Ctrl Pts',(2.60426813968415,1.36943262154935,18.8992401208973));
#102066=CARTESIAN_POINT('Ctrl Pts',(2.62540680139961,1.32763064410424,18.896690202543));
#102067=CARTESIAN_POINT('Ctrl Pts',(2.6672905051767,1.24480507717982,18.8916378474581));
#102068=CARTESIAN_POINT('Ctrl Pts',(2.70532608200568,1.15984695171912,18.8865854923732));
#102069=CARTESIAN_POINT('Ctrl Pts',(2.73929102786788,1.07314894802284,18.8815331372883));
#102070=CARTESIAN_POINT('Ctrl Pts',(2.77320914124541,0.986570487662384,
18.8764877486311));
#102071=CARTESIAN_POINT('Ctrl Pts',(2.80306761633522,0.898257326286103,
18.871442359974));
#102072=CARTESIAN_POINT('Ctrl Pts',(2.82869015019114,0.808626016284171,
18.8663969713168));
#102073=CARTESIAN_POINT('Ctrl Pts',(2.85428527070502,0.719090602096955,
18.8613569806803));
#102074=CARTESIAN_POINT('Ctrl Pts',(2.87565333658132,0.628240267261544,
18.8563169900437));
#102075=CARTESIAN_POINT('Ctrl Pts',(2.89266681195559,0.536509752950196,
18.8512769994071));
#102076=CARTESIAN_POINT('Ctrl Pts',(2.90966802877374,0.4448453323459,18.8462406401866));
#102077=CARTESIAN_POINT('Ctrl Pts',(2.9223208106768,0.352302428338124,18.8412042809661));
#102078=CARTESIAN_POINT('Ctrl Pts',(2.93054823392241,0.259328071473634,
18.8361679217457));
#102079=CARTESIAN_POINT('Ctrl Pts',(2.93877266725247,0.166387502280889,
18.8311333927809));
#102080=CARTESIAN_POINT('Ctrl Pts',(2.94257489769723,0.0730162337843075,
18.8260988638162));
#102081=CARTESIAN_POINT('Ctrl Pts',(2.94192973916421,-0.0203324819239022,
18.8210643348515));
#102082=CARTESIAN_POINT('Ctrl Pts',(2.94128463462324,-0.113673385462975,
18.8160302272165));
#102083=CARTESIAN_POINT('Ctrl Pts',(2.93619288436819,-0.206991295738175,
18.8109961195815));
#102084=CARTESIAN_POINT('Ctrl Pts',(2.92668142602032,-0.299833004500295,
18.8059620119466));
#102085=CARTESIAN_POINT('Ctrl Pts',(2.9171681031507,-0.392692912930471,
18.8009269174805));
#102086=CARTESIAN_POINT('Ctrl Pts',(2.90323339717147,-0.485075992593114,
18.7958918230144));
#102087=CARTESIAN_POINT('Ctrl Pts',(2.88495597832126,-0.576535344231749,
18.7908567285483));
#102088=CARTESIAN_POINT('Ctrl Pts',(2.86665848002041,-0.668095172505063,
18.7858161025609));
#102089=CARTESIAN_POINT('Ctrl Pts',(2.84400883282038,-0.758728810793993,
18.7807754765736));
#102090=CARTESIAN_POINT('Ctrl Pts',(2.81713653443116,-0.848001029700555,
18.7757348505862));
#102091=CARTESIAN_POINT('Ctrl Pts',(2.79024772299382,-0.937328106454573,
18.7706911271303));
#102092=CARTESIAN_POINT('Ctrl Pts',(2.75913124262189,-1.0252916798351,18.7656474036744));
#102093=CARTESIAN_POINT('Ctrl Pts',(2.72396528790127,-1.11147519554372,
18.7606036802185));
#102094=CARTESIAN_POINT('Ctrl Pts',(2.6887424218923,-1.19779818748587,18.755551794186));
#102095=CARTESIAN_POINT('Ctrl Pts',(2.64945718524543,-1.28233496828952,
18.7504999081535));
#102096=CARTESIAN_POINT('Ctrl Pts',(2.60633428179739,-1.36469249705847,
18.7454480221209));
#102097=CARTESIAN_POINT('Ctrl Pts',(2.58456817657085,-1.40626211538306,
18.742898103767));
#102098=CARTESIAN_POINT('Ctrl Pts',(2.56182505668172,-1.44727696979346,
18.7403481854131));
#102099=CARTESIAN_POINT('Ctrl Pts',(2.53813792349735,-1.48768944383718,
18.7377982670592));
#102100=CARTESIAN_POINT('Ctrl Pts',(2.49120473145713,-1.56776187769192,
18.7327459119742));
#102101=CARTESIAN_POINT('Ctrl Pts',(2.44039445977421,-1.64575485479938,
18.7276935568893));
#102102=CARTESIAN_POINT('Ctrl Pts',(2.38591665779354,-1.72126863158059,
18.7226412018044));
#102103=CARTESIAN_POINT('Ctrl Pts',(2.33151397240029,-1.79667828637065,
18.7175958131472));
#102104=CARTESIAN_POINT('Ctrl Pts',(2.27345406320861,-1.86961517656822,
18.71255042449));
#102105=CARTESIAN_POINT('Ctrl Pts',(2.21199157264906,-1.93970546282922,
18.7075050358328));
#102106=CARTESIAN_POINT('Ctrl Pts',(2.1505948403116,-2.00972076005923,18.7024650451962));
#102107=CARTESIAN_POINT('Ctrl Pts',(2.08580305376895,-2.07689517465094,
18.6974250545596));
#102108=CARTESIAN_POINT('Ctrl Pts',(2.01791256126694,-2.14088600702632,
18.692385063923));
#102109=CARTESIAN_POINT('Ctrl Pts',(1.9500709852501,-2.20483073270121,18.6873487047025));
#102110=CARTESIAN_POINT('Ctrl Pts',(1.87913546338631,-2.26559613165534,
18.682312345482));
#102111=CARTESIAN_POINT('Ctrl Pts',(1.80544009027429,-2.32287539063772,
18.6772759862615));
#102112=CARTESIAN_POINT('Ctrl Pts',(1.73177149868744,-2.38013383385039,
18.6722414572967));
#102113=CARTESIAN_POINT('Ctrl Pts',(1.65534539872847,-2.43390838156707,
18.667206928332));
#102114=CARTESIAN_POINT('Ctrl Pts',(1.5765291405612,-2.48393233985175,18.6621723993672));
#102115=CARTESIAN_POINT('Ctrl Pts',(1.49771947837047,-2.53395211173043,
18.6571382917322));
#102116=CARTESIAN_POINT('Ctrl Pts',(1.41652043084509,-2.58022168034536,
18.6521041840973));
#102117=CARTESIAN_POINT('Ctrl Pts',(1.33332754630043,-2.62251818950346,
18.6470700764623));
#102118=CARTESIAN_POINT('Ctrl Pts',(1.25011835353707,-2.66482299000431,
18.6420349819961));
#102119=CARTESIAN_POINT('Ctrl Pts',(1.16491494366667,-2.70315298328898,
18.63699988753));
#102120=CARTESIAN_POINT('Ctrl Pts',(1.07813558496178,-2.73733221594295,
18.6319647930639));
#102121=CARTESIAN_POINT('Ctrl Pts',(0.991260891031381,-2.77154899767426,
18.6269241670765));
#102122=CARTESIAN_POINT('Ctrl Pts',(0.902807206311567,-2.80160575344233,
18.6218835410892));
#102123=CARTESIAN_POINT('Ctrl Pts',(0.813210522501238,-2.82737557570501,
18.6168429151018));
#102124=CARTESIAN_POINT('Ctrl Pts',(0.723558781459588,-2.85316123354336,
18.6117991916459));
#102125=CARTESIAN_POINT('Ctrl Pts',(0.632763075009238,-2.87465461119352,
18.6067554681899));
#102126=CARTESIAN_POINT('Ctrl Pts',(0.541270075704358,-2.8917798507402,
18.601711744734));
#102127=CARTESIAN_POINT('Ctrl Pts',(0.449629007492839,-2.908932805145,18.5966598587015));
#102128=CARTESIAN_POINT('Ctrl Pts',(0.357288833070872,-2.9217034478382,
18.5916079726689));
#102129=CARTESIAN_POINT('Ctrl Pts',(0.264701653862861,-2.93006775253445,
18.5865560866364));
#102130=CARTESIAN_POINT('Ctrl Pts',(0.217968662251847,-2.93428960035988,
18.5840061682827));
#102131=CARTESIAN_POINT('Ctrl Pts',(0.17117275126887,-2.93738968091731,
18.581456249929));
#102132=CARTESIAN_POINT('Ctrl Pts',(0.124371822788037,-2.93936994093911,
18.5789063315753));
#102133=CARTESIAN_POINT('Ctrl Pts',(0.031641438442038,-2.94329358687708,
18.5738539764904));
#102134=CARTESIAN_POINT('Ctrl Pts',(-0.061441185936314,-2.94283182361192,
18.5688016214055));
#102135=CARTESIAN_POINT('Ctrl Pts',(-0.154426523870621,-2.93794425555102,
18.5637492663206));
#102136=CARTESIAN_POINT('Ctrl Pts',(-0.247283649193262,-2.9330634267017,
18.5587038776634));
#102137=CARTESIAN_POINT('Ctrl Pts',(-0.340043314851987,-2.92376894264891,
18.5536584890063));
#102138=CARTESIAN_POINT('Ctrl Pts',(-0.432253342304631,-2.91007234412935,
18.5486131003491));
#102139=CARTESIAN_POINT('Ctrl Pts',(-0.524364714993929,-2.89639039948988,
18.5435731097126));
#102140=CARTESIAN_POINT('Ctrl Pts',(-0.615927181263999,-2.87831576672546,
18.538533119076));
#102141=CARTESIAN_POINT('Ctrl Pts',(-0.706492146231467,-2.85591191168657,
18.5334931284394));
#102142=CARTESIAN_POINT('Ctrl Pts',(-0.796991857293626,-2.83352419908241,
18.5284567692189));
#102143=CARTESIAN_POINT('Ctrl Pts',(-0.88649506560938,-2.80681357061309,
18.5234204099985));
#102144=CARTESIAN_POINT('Ctrl Pts',(-0.974562894613587,-2.77589466018478,
18.518384050778));
#102145=CARTESIAN_POINT('Ctrl Pts',(-1.06259871902001,-2.74498698595138,
18.5133495218133));
#102146=CARTESIAN_POINT('Ctrl Pts',(-1.149199781652,-2.70987421494151,18.5083149928485));
#102147=CARTESIAN_POINT('Ctrl Pts',(-1.23394291503919,-2.67072066724032,
18.5032804638838));
#102148=CARTESIAN_POINT('Ctrl Pts',(-1.31867895644151,-2.63157039622194,
18.4982463562488));
#102149=CARTESIAN_POINT('Ctrl Pts',(-1.4015569745436,-2.58838020735632,
18.4932122486139));
#102150=CARTESIAN_POINT('Ctrl Pts',(-1.48217537615585,-2.54136187000538,
18.4881781409789));
#102151=CARTESIAN_POINT('Ctrl Pts',(-1.56280958131321,-2.49433431569653,
18.4831430465128));
#102152=CARTESIAN_POINT('Ctrl Pts',(-1.64118290674502,-2.4434773466619,
18.4781079520467));
#102153=CARTESIAN_POINT('Ctrl Pts',(-1.71692087743556,-2.38904723700179,
18.4730728575807));
#102154=CARTESIAN_POINT('Ctrl Pts',(-1.79274205335657,-2.33455733078551,
18.4680322315933));
#102155=CARTESIAN_POINT('Ctrl Pts',(-1.8659217341141,-2.27648670798884,
18.462991605606));
#102156=CARTESIAN_POINT('Ctrl Pts',(-1.93611707088297,-2.21513310837872,
18.4579509796186));
#102157=CARTESIAN_POINT('Ctrl Pts',(-2.00635554274028,-2.15374180693444,
18.4529072561627));
#102158=CARTESIAN_POINT('Ctrl Pts',(-2.07360569975744,-2.08906382015598,
18.4478635327068));
#102159=CARTESIAN_POINT('Ctrl Pts',(-2.13756181851492,-2.02143351907185,
18.4428198092509));
#102160=CARTESIAN_POINT('Ctrl Pts',(-2.20162144150386,-1.95369376759464,
18.4377679232184));
#102161=CARTESIAN_POINT('Ctrl Pts',(-2.26237609450512,-1.88299249981471,
18.4327160371859));
#102162=CARTESIAN_POINT('Ctrl Pts',(-2.31956068179755,-1.80969672692937,
18.4276641511534));
#102163=CARTESIAN_POINT('Ctrl Pts',(-2.34842436315619,-1.77270099200033,
18.4251142327994));
#102164=CARTESIAN_POINT('Ctrl Pts',(-2.37637919570815,-1.7350447160066,
18.4225643144454));
#102165=CARTESIAN_POINT('Ctrl Pts',(-2.40339545084291,-1.69677762445984,
18.4200143960914));
#102166=CARTESIAN_POINT('Ctrl Pts',(-2.45748613940064,-1.62016103490882,
18.4149090682491));
#102167=CARTESIAN_POINT('Ctrl Pts',(-2.50800397783905,-1.54082190742877,
18.4098037404068));
#102168=CARTESIAN_POINT('Ctrl Pts',(-2.55466696623876,-1.45912326128003,
18.4046984125645));
#102169=CARTESIAN_POINT('Ctrl Pts',(-2.60126251559766,-1.37754268897355,
18.399600463127));
#102170=CARTESIAN_POINT('Ctrl Pts',(-2.64401407535284,-1.29360974706232,
18.3945025136894));
#102171=CARTESIAN_POINT('Ctrl Pts',(-2.68268178742546,-1.20771785919383,
18.3894045642518));
#102172=CARTESIAN_POINT('Ctrl Pts',(-2.72130365097083,-1.12192781382781,
18.384312659482));
#102173=CARTESIAN_POINT('Ctrl Pts',(-2.75585111713689,-1.03418383174471,
18.3792207547122));
#102174=CARTESIAN_POINT('Ctrl Pts',(-2.78612980181422,-0.944904612880396,
18.3741288499424));
#102175=CARTESIAN_POINT('Ctrl Pts',(-2.81637713708088,-0.855717830359562,
18.3690422171392));
#102176=CARTESIAN_POINT('Ctrl Pts',(-2.84236434750889,-0.764999381684115,
18.363955584336));
#102177=CARTESIAN_POINT('Ctrl Pts',(-2.86394525918279,-0.673187605652688,
18.3588689515328));
#102178=CARTESIAN_POINT('Ctrl Pts',(-2.8855131439674,-0.581431249978891,
18.3537853891745));
#102179=CARTESIAN_POINT('Ctrl Pts',(-2.90267992053475,-0.48858329900202,
18.3487018268163));
#102180=CARTESIAN_POINT('Ctrl Pts',(-2.91534955181019,-0.395096179126181,
18.3436182644581));
#102181=CARTESIAN_POINT('Ctrl Pts',(-2.92801563564908,-0.301635235199658,
18.3385361254732));
#102182=CARTESIAN_POINT('Ctrl Pts',(-2.93618701854107,-0.207535905832476,
18.3334539864883));
#102183=CARTESIAN_POINT('Ctrl Pts',(-2.93981911662979,-0.11325882525462,
18.3283718475034));
#102184=CARTESIAN_POINT('Ctrl Pts',(-2.94129510280155,-0.0749471762164033,
18.3263066040321));
#102185=CARTESIAN_POINT('Ctrl Pts',(-2.94202207254817,-0.0366062362852832,
18.3242413605609));
#102186=CARTESIAN_POINT('Ctrl Pts',(-2.94199948962717,0.00173292627207862,
18.3221761170896));
#102187=CARTESIAN_POINT('',(-2.94199959735173,0.00153921481298652,17.3221761170896));
#102188=CARTESIAN_POINT('Ctrl Pts',(-2.93820320684436,0.00175244785142763,
18.3221749435376));
#102189=CARTESIAN_POINT('Ctrl Pts',(-2.94022008061527,0.379058827004991,
18.3018241158943));
#102190=CARTESIAN_POINT('Ctrl Pts',(-2.69739443497224,1.73582009319941,
18.2285093097562));
#102191=CARTESIAN_POINT('Ctrl Pts',(-0.652918847946833,3.41637487504018,
18.1022305251237));
#102192=CARTESIAN_POINT('Ctrl Pts',(2.51804505593664,2.39945189680271,17.9433385896398));
#102193=CARTESIAN_POINT('Ctrl Pts',(3.38092917609235,-0.816846506422659,
17.7844466541558));
#102194=CARTESIAN_POINT('Ctrl Pts',(1.14480032856239,-3.28441052801307,
17.6255547186722));
#102195=CARTESIAN_POINT('Ctrl Pts',(-2.04137315956266,-2.75784263173558,
17.4714650030246));
#102196=CARTESIAN_POINT('Ctrl Pts',(-2.94019247693566,-0.885490005612207,
17.3703392658718));
#102197=CARTESIAN_POINT('Ctrl Pts',(-2.94584118639794,0.00151562255014574,
17.3221775072136));
#102198=CARTESIAN_POINT('',(-2.94199883051083,-0.00262321804808858,16.3221761170896));
#102199=CARTESIAN_POINT('Ctrl Pts',(-2.94199959735173,0.00153921481298652,
17.3221761170896));
#102200=CARTESIAN_POINT('Ctrl Pts',(-2.94195338985515,0.0898585547750324,
17.3173743606278));
#102201=CARTESIAN_POINT('Ctrl Pts',(-2.93793050094627,0.178071157293918,
17.3125726041661));
#102202=CARTESIAN_POINT('Ctrl Pts',(-2.92995744410738,0.265919867102419,
17.3077708477044));
#102203=CARTESIAN_POINT('Ctrl Pts',(-2.92156828181176,0.358353308746736,
17.3027184926196));
#102204=CARTESIAN_POINT('Ctrl Pts',(-2.90878568317249,0.450555224986806,
17.2976661375348));
#102205=CARTESIAN_POINT('Ctrl Pts',(-2.89162912925254,0.542074698596224,
17.29261378245));
#102206=CARTESIAN_POINT('Ctrl Pts',(-2.87449623160611,0.633467980797424,
17.2875683937929));
#102207=CARTESIAN_POINT('Ctrl Pts',(-2.85300144423318,0.724180257378679,
17.2825230051358));
#102208=CARTESIAN_POINT('Ctrl Pts',(-2.82721607839617,0.813764859193481,
17.2774776164788));
#102209=CARTESIAN_POINT('Ctrl Pts',(-2.80145830011376,0.903253615166505,
17.2724376258423));
#102210=CARTESIAN_POINT('Ctrl Pts',(-2.77141918981817,0.991616669841535,
17.2673976352058));
#102211=CARTESIAN_POINT('Ctrl Pts',(-2.7372210521935,1.07841778148763,17.2623576445692));
#102212=CARTESIAN_POINT('Ctrl Pts',(-2.70304755502481,1.16515635116161,
17.2573212853488));
#102213=CARTESIAN_POINT('Ctrl Pts',(-2.66472114919312,1.25033480259103,
17.2522849261284));
#102214=CARTESIAN_POINT('Ctrl Pts',(-2.62241357013272,1.3335333018653,17.2472485669079));
#102215=CARTESIAN_POINT('Ctrl Pts',(-2.58012136600628,1.41670156609753,
17.2422140379432));
#102216=CARTESIAN_POINT('Ctrl Pts',(-2.53385106402202,1.49789091201869,
17.2371795089785));
#102217=CARTESIAN_POINT('Ctrl Pts',(-2.4838215683074,1.57670365535537,17.2321449800138));
#102218=CARTESIAN_POINT('Ctrl Pts',(-2.43379625946213,1.65550980300973,
17.2271108723789));
#102219=CARTESIAN_POINT('Ctrl Pts',(-2.38001262062241,1.73193936857028,
17.2220767647439));
#102220=CARTESIAN_POINT('Ctrl Pts',(-2.32273373080331,1.80562233476121,
17.217042657109));
#102221=CARTESIAN_POINT('Ctrl Pts',(-2.2654436126604,1.87931974495073,17.2120075626429));
#102222=CARTESIAN_POINT('Ctrl Pts',(-2.2046571557093,1.95026913599676,17.2069724681769));
#102223=CARTESIAN_POINT('Ctrl Pts',(-2.14067796118339,2.0181332628208,17.2019373737108));
#102224=CARTESIAN_POINT('Ctrl Pts',(-2.07662847954028,2.0860719447228,17.1968967477235));
#102225=CARTESIAN_POINT('Ctrl Pts',(-2.00937956411379,2.15091827292692,
17.1918561217361));
#102226=CARTESIAN_POINT('Ctrl Pts',(-1.93927172914376,2.21237184047885,
17.1868154957488));
#102227=CARTESIAN_POINT('Ctrl Pts',(-1.86912081285496,2.27386317129553,
17.1817717722929));
#102228=CARTESIAN_POINT('Ctrl Pts',(-1.7961078269276,2.33195731453227,17.176728048837));
#102229=CARTESIAN_POINT('Ctrl Pts',(-1.72060467862743,2.38639551204016,
17.1716843253811));
#102230=CARTESIAN_POINT('Ctrl Pts',(-1.6449793388078,2.44092181032556,17.1666324393486));
#102231=CARTESIAN_POINT('Ctrl Pts',(-1.5668561630896,2.49178010898528,17.1615805533161));
#102232=CARTESIAN_POINT('Ctrl Pts',(-1.48663403208002,2.53875624167849,
17.1565286672836));
#102233=CARTESIAN_POINT('Ctrl Pts',(-1.44614224683807,2.562467248262,17.1539787489291));
#102234=CARTESIAN_POINT('Ctrl Pts',(-1.40511607543183,2.5851899471607,17.1514288305747));
#102235=CARTESIAN_POINT('Ctrl Pts',(-1.36360874186484,2.60690145558089,
17.1488789122202));
#102236=CARTESIAN_POINT('Ctrl Pts',(-1.28136697618504,2.64992018587747,
17.1438265571353));
#102237=CARTESIAN_POINT('Ctrl Pts',(-1.19693993558253,2.68912047926456,
17.1387742020504));
#102238=CARTESIAN_POINT('Ctrl Pts',(-1.11071720343281,2.7242744527669,17.1337218469654));
#102239=CARTESIAN_POINT('Ctrl Pts',(-1.02461335929191,2.75937995429663,
17.1286764583083));
#102240=CARTESIAN_POINT('Ctrl Pts',(-0.936719151501308,2.79045005638599,
17.1236310696511));
#102241=CARTESIAN_POINT('Ctrl Pts',(-0.847448668608993,2.81730274448325,
17.118585680994));
#102242=CARTESIAN_POINT('Ctrl Pts',(-0.75827369548509,2.84412670310647,
17.1135456903574));
#102243=CARTESIAN_POINT('Ctrl Pts',(-0.667725797136911,2.8667420891036,
17.1085056997208));
#102244=CARTESIAN_POINT('Ctrl Pts',(-0.57623791980171,2.88501540026784,
17.1034657090842));
#102245=CARTESIAN_POINT('Ctrl Pts',(-0.484815961348971,2.90327554513851,
17.0984293498637));
#102246=CARTESIAN_POINT('Ctrl Pts',(-0.392455804470684,2.9171997468574,
17.0933929906432));
#102247=CARTESIAN_POINT('Ctrl Pts',(-0.299603379615979,2.92670494155504,
17.0883566314227));
#102248=CARTESIAN_POINT('Ctrl Pts',(-0.206784698121945,2.9362066819841,
17.083322102458));
#102249=CARTESIAN_POINT('Ctrl Pts',(-0.113474545530137,2.94129256050306,
17.0782875734933));
#102250=CARTESIAN_POINT('Ctrl Pts',(-0.0201257847241223,2.94193116044364,
17.0732530445286));
#102251=CARTESIAN_POINT('Ctrl Pts',(0.0732151639092051,2.94256970694105,
17.0682189368936));
#102252=CARTESIAN_POINT('Ctrl Pts',(0.1665942701018,2.93876171199624,17.0631848292586));
#102253=CARTESIAN_POINT('Ctrl Pts',(0.259557998022685,2.93052787832883,
17.0581507216237));
#102254=CARTESIAN_POINT('Ctrl Pts',(0.352539949530698,2.92229243059119,
17.0531156271576));
#102255=CARTESIAN_POINT('Ctrl Pts',(0.44510591860608,2.9096294606468,17.0480805326915));
#102256=CARTESIAN_POINT('Ctrl Pts',(0.536807966405932,2.89261148569993,
17.0430454382254));
#102257=CARTESIAN_POINT('Ctrl Pts',(0.628610757464931,2.87557481491908,
17.0380048122381));
#102258=CARTESIAN_POINT('Ctrl Pts',(0.719547295281639,2.8541736701438,17.0329641862508));
#102259=CARTESIAN_POINT('Ctrl Pts',(0.809180610807341,2.82853155172317,
17.0279235602634));
#102260=CARTESIAN_POINT('Ctrl Pts',(0.898869006074743,2.80287367620094,
17.0228798368075));
#102261=CARTESIAN_POINT('Ctrl Pts',(0.98725216425927,2.77296978110414,17.0178361133516));
#102262=CARTESIAN_POINT('Ctrl Pts',(1.07391111998423,2.73899231586622,17.0127923898957));
#102263=CARTESIAN_POINT('Ctrl Pts',(1.16071032137726,2.7049598627477,17.0077405038632));
#102264=CARTESIAN_POINT('Ctrl Pts',(1.24577934477105,2.66684085979808,17.0026886178307));
#102265=CARTESIAN_POINT('Ctrl Pts',(1.32872209638949,2.62485458465156,16.9976367317981));
#102266=CARTESIAN_POINT('Ctrl Pts',(1.37058710349889,2.60366218780907,16.9950868134443));
#102267=CARTESIAN_POINT('Ctrl Pts',(1.41191083470068,2.58148523977796,16.9925368950905));
#102268=CARTESIAN_POINT('Ctrl Pts',(1.45264522422215,2.55835608400093,16.9899869767367));
#102269=CARTESIAN_POINT('Ctrl Pts',(1.533355494699,2.51252845676519,16.9849346216518));
#102270=CARTESIAN_POINT('Ctrl Pts',(1.61203982124248,2.46279552056619,16.9798822665668));
#102271=CARTESIAN_POINT('Ctrl Pts',(1.68829561642655,2.40936130780647,16.9748299114819));
#102272=CARTESIAN_POINT('Ctrl Pts',(1.76444626648908,2.35600077268372,16.9697845228247));
#102273=CARTESIAN_POINT('Ctrl Pts',(1.83817467858619,2.29894935502687,16.9647391341676));
#102274=CARTESIAN_POINT('Ctrl Pts',(1.90910354697363,2.23845653228574,16.9596937455104));
#102275=CARTESIAN_POINT('Ctrl Pts',(1.9799565291378,2.17802843032696,16.9546537548738));
#102276=CARTESIAN_POINT('Ctrl Pts',(2.04801558483876,2.11416652841203,16.9496137642372));
#102277=CARTESIAN_POINT('Ctrl Pts',(2.11293397163064,2.04716243408509,16.9445737736006));
#102278=CARTESIAN_POINT('Ctrl Pts',(2.17780558340019,1.98020661757531,16.9395374143801));
#102279=CARTESIAN_POINT('Ctrl Pts',(2.23954071589448,1.91011342683583,16.9345010551596));
#102280=CARTESIAN_POINT('Ctrl Pts',(2.29782799052727,1.83721270569017,16.9294646959391));
#102281=CARTESIAN_POINT('Ctrl Pts',(2.3560940830689,1.76433847728639,16.9244301669743));
#102282=CARTESIAN_POINT('Ctrl Pts',(2.41091452979415,1.68865909199619,16.9193956380096));
#102283=CARTESIAN_POINT('Ctrl Pts',(2.46201761031975,1.61053819776975,16.9143611090448));
#102284=CARTESIAN_POINT('Ctrl Pts',(2.51311641412983,1.5324238413261,16.9093270014098));
#102285=CARTESIAN_POINT('Ctrl Pts',(2.56049822724371,1.45186875405722,16.9042928937748));
#102286=CARTESIAN_POINT('Ctrl Pts',(2.6039347751051,1.36926538223909,16.8992587861398));
#102287=CARTESIAN_POINT('Ctrl Pts',(2.64737983778979,1.28664581776409,16.8942236916737));
#102288=CARTESIAN_POINT('Ctrl Pts',(2.68687789285477,1.2019775646535,16.8891885972076));
#102289=CARTESIAN_POINT('Ctrl Pts',(2.72224725165072,1.11567643198202,16.8841535027415));
#102290=CARTESIAN_POINT('Ctrl Pts',(2.75765546698875,1.02928048946079,16.8791128767541));
#102291=CARTESIAN_POINT('Ctrl Pts',(2.78892576343315,0.94124849829791,16.8740722507667));
#102292=CARTESIAN_POINT('Ctrl Pts',(2.81592524984324,0.8520146637795,16.8690316247793));
#102293=CARTESIAN_POINT('Ctrl Pts',(2.8429413274586,0.762725995000777,16.8639879013234));
#102294=CARTESIAN_POINT('Ctrl Pts',(2.86568126215085,0.672234443114071,
16.8589441778675));
#102295=CARTESIAN_POINT('Ctrl Pts',(2.88406306069973,0.580985595266636,
16.8539004544115));
#102296=CARTESIAN_POINT('Ctrl Pts',(2.90247460767559,0.489589073638481,
16.848848568379));
#102297=CARTESIAN_POINT('Ctrl Pts',(2.91651387117682,0.397433247954863,
16.8437966823464));
#102298=CARTESIAN_POINT('Ctrl Pts',(2.92615061005617,0.304969846489582,
16.8387447963138));
#102299=CARTESIAN_POINT('Ctrl Pts',(2.93101471371576,0.258299331175658,
16.8361948779601));
#102300=CARTESIAN_POINT('Ctrl Pts',(2.93475802142384,0.211550476305253,
16.8336449596063));
#102301=CARTESIAN_POINT('Ctrl Pts',(2.93738168348325,0.164781205048134,
16.8310950412526));
#102302=CARTESIAN_POINT('Ctrl Pts',(2.94258015280972,0.0721135456674554,
16.8260426861677));
#102303=CARTESIAN_POINT('Ctrl Pts',(2.94339847148584,-0.020966626985196,
16.8209903310827));
#102304=CARTESIAN_POINT('Ctrl Pts',(2.93979006601469,-0.114010384445283,
16.8159379759978));
#102305=CARTESIAN_POINT('Ctrl Pts',(2.93618663598482,-0.206925848742052,
16.8108925873407));
#102306=CARTESIAN_POINT('Ctrl Pts',(2.92816862786905,-0.299804557566006,
16.8058471986835));
#102307=CARTESIAN_POINT('Ctrl Pts',(2.91574136311853,-0.392194216428167,
16.8008018100264));
#102308=CARTESIAN_POINT('Ctrl Pts',(2.90332739419818,-0.484485028340664,
16.7957618193898));
#102309=CARTESIAN_POINT('Ctrl Pts',(2.88651360415682,-0.576287392381419,
16.7907218287532));
#102310=CARTESIAN_POINT('Ctrl Pts',(2.86535728393064,-0.667151883326165,
16.7856818381167));
#102311=CARTESIAN_POINT('Ctrl Pts',(2.84421620726486,-0.757950904551132,
16.7806454788962));
#102312=CARTESIAN_POINT('Ctrl Pts',(2.818738919959,-0.847812964418424,16.7756091196757));
#102313=CARTESIAN_POINT('Ctrl Pts',(2.78903400980932,-0.936297651458644,
16.7705727604552));
#102314=CARTESIAN_POINT('Ctrl Pts',(2.75933989467654,-1.02475018241126,
16.7655382314905));
#102315=CARTESIAN_POINT('Ctrl Pts',(2.72542135007341,-1.11182591421406,
16.7605037025258));
#102316=CARTESIAN_POINT('Ctrl Pts',(2.68743686130267,-1.19709945974078,
16.7554691735611));
#102317=CARTESIAN_POINT('Ctrl Pts',(2.6494555513785,-1.2823658688935,16.7504350659261));
#102318=CARTESIAN_POINT('Ctrl Pts',(2.60740915475619,-1.3658299859131,16.7454009582911));
#102319=CARTESIAN_POINT('Ctrl Pts',(2.56150389821012,-1.44708734340894,
16.7403668506562));
#102320=CARTESIAN_POINT('Ctrl Pts',(2.51558964290223,-1.52836062970383,
16.7353317561901));
#102321=CARTESIAN_POINT('Ctrl Pts',(2.4658152441783,-1.60742591077158,16.730296661724));
#102322=CARTESIAN_POINT('Ctrl Pts',(2.41243180226208,-1.68390522281823,
16.7252615672579));
#102323=CARTESIAN_POINT('Ctrl Pts',(2.35898971365203,-1.76046855452786,
16.7202209412706));
#102324=CARTESIAN_POINT('Ctrl Pts',(2.3019309221703,-1.8344398815566,16.7151803152832));
#102325=CARTESIAN_POINT('Ctrl Pts',(2.2415484246982,-1.90547229308983,16.7101396892959));
#102326=CARTESIAN_POINT('Ctrl Pts',(2.18112882213468,-1.97654835409491,
16.70509596584));
#102327=CARTESIAN_POINT('Ctrl Pts',(2.117381750805,-2.04468158012666,16.7000522423841));
#102328=CARTESIAN_POINT('Ctrl Pts',(2.05063734592326,-2.10956167852585,
16.6950085189282));
#102329=CARTESIAN_POINT('Ctrl Pts',(1.98378492435044,-2.17454677649105,
16.6899566328956));
#102330=CARTESIAN_POINT('Ctrl Pts',(1.9139258177695,-2.2362679426719,16.6849047468631));
#102331=CARTESIAN_POINT('Ctrl Pts',(1.84142335717426,-2.2944550594102,16.6798528608306));
#102332=CARTESIAN_POINT('Ctrl Pts',(1.80482804330819,-2.32382476331429,
16.6773029424767));
#102333=CARTESIAN_POINT('Ctrl Pts',(1.76755975267996,-2.35229478787051,
16.6747530241228));
#102334=CARTESIAN_POINT('Ctrl Pts',(1.72966779728228,-2.37983472347234,
16.6722031057688));
#102335=CARTESIAN_POINT('Ctrl Pts',(1.65458946654393,-2.43440177792827,
16.6671507506839));
#102336=CARTESIAN_POINT('Ctrl Pts',(1.57679169355735,-2.48551043379844,
16.662098395599));
#102337=CARTESIAN_POINT('Ctrl Pts',(1.49662660875606,-2.53287836146218,
16.6570460405141));
#102338=CARTESIAN_POINT('Ctrl Pts',(1.41657205939096,-2.58018097597171,
16.6520006518569));
#102339=CARTESIAN_POINT('Ctrl Pts',(1.33415706366861,-2.6237528876472,16.6469552631998));
#102340=CARTESIAN_POINT('Ctrl Pts',(1.24976469250958,-2.66335356521744,
16.6419098745426));
#102341=CARTESIAN_POINT('Ctrl Pts',(1.16546261206667,-2.70291187434267,
16.6368698839061));
#102342=CARTESIAN_POINT('Ctrl Pts',(1.07918776122747,-2.73850720678566,
16.6318298932695));
#102343=CARTESIAN_POINT('Ctrl Pts',(0.991348950535218,-2.76994426988572,
16.6267899026329));
#102344=CARTESIAN_POINT('Ctrl Pts',(0.903573429498407,-2.80135868194034,
16.6217535434124));
#102345=CARTESIAN_POINT('Ctrl Pts',(0.81423660546987,-2.82862063059728,
16.6167171841919));
#102346=CARTESIAN_POINT('Ctrl Pts',(0.72376749934292,-2.85158282483516,
16.6116808249714));
#102347=CARTESIAN_POINT('Ctrl Pts',(0.633331270458338,-2.87453667441643,
16.6066462960067));
#102348=CARTESIAN_POINT('Ctrl Pts',(0.541764007080707,-2.89319376461131,
16.601611767042));
#102349=CARTESIAN_POINT('Ctrl Pts',(0.44950913007251,-2.90745688566167,
16.5965772380772));
#102350=CARTESIAN_POINT('Ctrl Pts',(0.357261973692089,-2.92171881305971,
16.5915431304423));
#102351=CARTESIAN_POINT('Ctrl Pts',(0.264327757146549,-2.93158743474038,
16.5865090228073));
#102352=CARTESIAN_POINT('Ctrl Pts',(0.171158177829341,-2.93701700338322,
16.5814749151723));
#102353=CARTESIAN_POINT('Ctrl Pts',(0.0779703345721042,-2.942447636379,
16.5764398207062));
#102354=CARTESIAN_POINT('Ctrl Pts',(-0.0154525196048733,-2.9434374626752,
16.5714047262401));
#102355=CARTESIAN_POINT('Ctrl Pts',(-0.108656658027342,-2.93999281132902,
16.566369631774));
#102356=CARTESIAN_POINT('Ctrl Pts',(-0.201963189895715,-2.93654437571181,
16.5613290057867));
#102357=CARTESIAN_POINT('Ctrl Pts',(-0.295050081760897,-2.92865175443276,
16.5562883797993));
#102358=CARTESIAN_POINT('Ctrl Pts',(-0.387467014278742,-2.91637331506889,
16.551247753812));
#102359=CARTESIAN_POINT('Ctrl Pts',(-0.479940737073067,-2.90408733059454,
16.5462040303561));
#102360=CARTESIAN_POINT('Ctrl Pts',(-0.571743244163261,-2.88741024198242,
16.5411603069001));
#102361=CARTESIAN_POINT('Ctrl Pts',(-0.662434879041171,-2.86645147020313,
16.5361165834442));
#102362=CARTESIAN_POINT('Ctrl Pts',(-0.753273285926816,-2.84545877951812,
16.5310646974117));
#102363=CARTESIAN_POINT('Ctrl Pts',(-0.84299680448902,-2.82017069252342,
16.5260128113792));
#102364=CARTESIAN_POINT('Ctrl Pts',(-0.931181566508105,-2.7907462962791,
16.5209609253466));
#102365=CARTESIAN_POINT('Ctrl Pts',(-0.975692456452476,-2.77589445529293,
16.5184110069927));
#102366=CARTESIAN_POINT('Ctrl Pts',(-1.01981164286292,-2.75998957632416,
16.5158610886389));
#102367=CARTESIAN_POINT('Ctrl Pts',(-1.06348685220657,-2.7430566372541,
16.513311170285));
#102368=CARTESIAN_POINT('Ctrl Pts',(-1.15002400178893,-2.70950606467081,
16.5082588152));
#102369=CARTESIAN_POINT('Ctrl Pts',(-1.23512720159307,-2.67179620429352,
16.5032064601151));
#102370=CARTESIAN_POINT('Ctrl Pts',(-1.31836838556014,-2.63007011312542,
16.4981541050302));
#102371=CARTESIAN_POINT('Ctrl Pts',(-1.40149479261909,-2.58840155587867,
16.493108716373));
#102372=CARTESIAN_POINT('Ctrl Pts',(-1.48276389197391,-2.54272796945177,
16.4880633277158));
#102373=CARTESIAN_POINT('Ctrl Pts',(-1.56176599207779,-2.49324106054535,
16.4830179390587));
#102374=CARTESIAN_POINT('Ctrl Pts',(-1.64068356847286,-2.44380709728306,
16.4779779484221));
#102375=CARTESIAN_POINT('Ctrl Pts',(-1.71733859210254,-2.39056815541317,
16.4729379577855));
#102376=CARTESIAN_POINT('Ctrl Pts',(-1.7913454550035,-2.33376208316922,
16.4678979671489));
#102377=CARTESIAN_POINT('Ctrl Pts',(-1.86529899444966,-2.27699694085942,
16.4628616079283));
#102378=CARTESIAN_POINT('Ctrl Pts',(-1.93660781431016,-2.21667004650681,
16.4578252487078));
#102379=CARTESIAN_POINT('Ctrl Pts',(-2.00491570790697,-2.15306223880963,
16.4527888894873));
#102380=CARTESIAN_POINT('Ctrl Pts',(-2.07319877783451,-2.08947754673053,
16.4477543605226));
#102381=CARTESIAN_POINT('Ctrl Pts',(-2.13848276323585,-2.02261461240077,
16.4427198315578));
#102382=CARTESIAN_POINT('Ctrl Pts',(-2.20044575423982,-1.95279350742672,
16.4376853025931));
#102383=CARTESIAN_POINT('Ctrl Pts',(-2.26240355968384,-1.88297824564261,
16.4326511949581));
#102384=CARTESIAN_POINT('Ctrl Pts',(-2.3210406285842,-1.81020563781778,
16.4276170873231));
#102385=CARTESIAN_POINT('Ctrl Pts',(-2.37607382587819,-1.73483058941689,
16.4225829796881));
#102386=CARTESIAN_POINT('Ctrl Pts',(-2.43111781127525,-1.65944076532005,
16.417547885222));
#102387=CARTESIAN_POINT('Ctrl Pts',(-2.48255626038281,-1.58144784646101,
16.4125127907559));
#102388=CARTESIAN_POINT('Ctrl Pts',(-2.53014871309665,-1.50123665343455,
16.4074776962898));
#102389=CARTESIAN_POINT('Ctrl Pts',(-2.5777934505621,-1.4209373409256,16.4024370703024));
#102390=CARTESIAN_POINT('Ctrl Pts',(-2.621583530638,-1.33841527239376,16.397396444315));
#102391=CARTESIAN_POINT('Ctrl Pts',(-2.66132408132544,-1.25408059316669,
16.3923558183277));
#102392=CARTESIAN_POINT('Ctrl Pts',(-2.701089052612,-1.16969409021402,16.3873120948717));
#102393=CARTESIAN_POINT('Ctrl Pts',(-2.73679937061715,-1.08349316921749,
16.3822683714158));
#102394=CARTESIAN_POINT('Ctrl Pts',(-2.76830885362323,-0.995906667791344,
16.3772246479598));
#102395=CARTESIAN_POINT('Ctrl Pts',(-2.79986933041819,-0.908178419591311,
16.3721727619273));
#102396=CARTESIAN_POINT('Ctrl Pts',(-2.8272152697665,-0.819060538510984,
16.3671208758947));
#102397=CARTESIAN_POINT('Ctrl Pts',(-2.8502507905131,-0.72899549462217,
16.3620689898622));
#102398=CARTESIAN_POINT('Ctrl Pts',(-2.86187787330175,-0.68353554026831,
16.3595190715085));
#102399=CARTESIAN_POINT('Ctrl Pts',(-2.87240761389315,-0.637834420508285,
16.3569691531547));
#102400=CARTESIAN_POINT('Ctrl Pts',(-2.88183269195836,-0.591949605591588,
16.354419234801));
#102401=CARTESIAN_POINT('Ctrl Pts',(-2.90840445752944,-0.462588284995289,
16.3472303465763));
#102402=CARTESIAN_POINT('Ctrl Pts',(-2.92627321214746,-0.331383124856715,
16.3400414583515));
#102403=CARTESIAN_POINT('Ctrl Pts',(-2.9352414658756,-0.199302626687303,
16.3328525701267));
#102404=CARTESIAN_POINT('Ctrl Pts',(-2.93968114819087,-0.133916937378105,
16.3292937524477));
#102405=CARTESIAN_POINT('Ctrl Pts',(-2.94194025492879,-0.0683170683806231,
16.3257349347686));
#102406=CARTESIAN_POINT('Ctrl Pts',(-2.94199883051083,-0.00262321804808858,
16.3221761170896));
#102407=CARTESIAN_POINT('',(-2.93715977492128,-5.64784450823863E-5,15.3221761170896));
#102408=CARTESIAN_POINT('Ctrl Pts',(-2.94289363775603,-0.00261552165817143,
16.3221756570734));
#102409=CARTESIAN_POINT('Ctrl Pts',(-2.93569250517499,0.776915332964193,
16.2799595378213));
#102410=CARTESIAN_POINT('Ctrl Pts',(-2.21711677136678,2.54616453756175,
16.1847794400746));
#102411=CARTESIAN_POINT('Ctrl Pts',(0.770275962800985,3.39184245653139,
16.0366353638335));
#102412=CARTESIAN_POINT('Ctrl Pts',(3.26835708375775,1.18985809316026,15.8777434283494));
#102413=CARTESIAN_POINT('Ctrl Pts',(2.77061059104582,-2.1027689510703,15.7188514928656));
#102414=CARTESIAN_POINT('Ctrl Pts',(-0.266721235415331,-3.46796483421923,
15.5599595573817));
#102415=CARTESIAN_POINT('Ctrl Pts',(-2.59084841052653,-1.95874493369377,
15.4277344321231));
#102416=CARTESIAN_POINT('Ctrl Pts',(-2.93724320497234,-0.488041625186228,
15.348473285359));
#102417=CARTESIAN_POINT('Ctrl Pts',(-2.93715977492128,-5.64784450823863E-5,
15.3221761170896));
#102418=CARTESIAN_POINT('',(-2.94199880731857,0.0026491010035377,14.3221761170896));
#102419=CARTESIAN_POINT('Ctrl Pts',(-2.93715977492128,-5.64784450823863E-5,
15.3221761170896));
#102420=CARTESIAN_POINT('Ctrl Pts',(-2.937075172149,0.494787953759478,15.2955093068644));
#102421=CARTESIAN_POINT('Ctrl Pts',(-2.58366435956491,1.97257547511542,
15.2158785181446));
#102422=CARTESIAN_POINT('Ctrl Pts',(-0.242551610946432,3.46973904275675,
15.08328375093));
#102423=CARTESIAN_POINT('Ctrl Pts',(2.78519444500115,2.08341359608163,14.9243918154463));
#102424=CARTESIAN_POINT('Ctrl Pts',(3.25998737681471,-1.212601588244,14.7654998799623));
#102425=CARTESIAN_POINT('Ctrl Pts',(0.746624500255915,-3.39712704566971,
14.6066079444785));
#102426=CARTESIAN_POINT('Ctrl Pts',(-2.22736502755342,-2.53281667794069,
14.4588334749138));
#102427=CARTESIAN_POINT('Ctrl Pts',(-2.93553126956538,-0.770202959613324,
14.3640229838439));
#102428=CARTESIAN_POINT('Ctrl Pts',(-2.94268592639251,0.00264317858251727,
14.3221764712686));
#102429=CARTESIAN_POINT('',(-2.94204920351317,-0.00143517523068308,13.3221761001659));
#102430=CARTESIAN_POINT('Ctrl Pts',(-2.94199880731857,0.0026491010035377,
14.3221761170896));
#102431=CARTESIAN_POINT('Ctrl Pts',(-2.94188124569359,0.13320892489109,
14.3151051111609));
#102432=CARTESIAN_POINT('Ctrl Pts',(-2.93306924346563,0.263391909828143,
14.3080341052323));
#102433=CARTESIAN_POINT('Ctrl Pts',(-2.91573305821569,0.392255953719244,
14.3009630993036));
#102434=CARTESIAN_POINT('Ctrl Pts',(-2.90581252724635,0.465997651781654,
14.2969167573727));
#102435=CARTESIAN_POINT('Ctrl Pts',(-2.89310147223706,0.539308078417644,
14.2928704154417));
#102436=CARTESIAN_POINT('Ctrl Pts',(-2.87763831285705,0.612014493600619,
14.2888240735108));
#102437=CARTESIAN_POINT('Ctrl Pts',(-2.85833065837412,0.702797386575274,
14.2837717184259));
#102438=CARTESIAN_POINT('Ctrl Pts',(-2.83468815976649,0.792828605861353,
14.278719363341));
#102439=CARTESIAN_POINT('Ctrl Pts',(-2.80678371344977,0.881662739324452,
14.273667008256));
#102440=CARTESIAN_POINT('Ctrl Pts',(-2.77891774311241,0.970374384054174,
14.2686216195989));
#102441=CARTESIAN_POINT('Ctrl Pts',(-2.746801634558,1.05789180276783,14.2635762309417));
#102442=CARTESIAN_POINT('Ctrl Pts',(-2.71055924304341,1.14377995696373,
14.2585308422846));
#102443=CARTESIAN_POINT('Ctrl Pts',(-2.67435562697068,1.22957622011739,
14.253490851648));
#102444=CARTESIAN_POINT('Ctrl Pts',(-2.63403467456658,1.31374627641001,
14.2484508610114));
#102445=CARTESIAN_POINT('Ctrl Pts',(-2.58976963518443,1.39587149719331,
14.2434108703748));
#102446=CARTESIAN_POINT('Ctrl Pts',(-2.54553648966638,1.47793754507929,
14.2383745111543));
#102447=CARTESIAN_POINT('Ctrl Pts',(-2.49736511581005,1.55796129600922,
14.2333381519338));
#102448=CARTESIAN_POINT('Ctrl Pts',(-2.44547589519023,1.63554628367513,
14.2283017927133));
#102449=CARTESIAN_POINT('Ctrl Pts',(-2.3936055315544,1.71310307629683,14.2232672637486));
#102450=CARTESIAN_POINT('Ctrl Pts',(-2.33802025197507,1.78822249742819,
14.2182327347838));
#102451=CARTESIAN_POINT('Ctrl Pts',(-2.27898464227407,1.8605356756265,14.2131982058191));
#102452=CARTESIAN_POINT('Ctrl Pts',(-2.21995397314617,1.93284280207831,
14.2081640981841));
#102453=CARTESIAN_POINT('Ctrl Pts',(-2.15747382908572,2.0023438085244,14.2031299905491));
#102454=CARTESIAN_POINT('Ctrl Pts',(-2.0918493722751,2.06870254113835,14.1980958829141));
#102455=CARTESIAN_POINT('Ctrl Pts',(-2.02621205116752,2.13507428198861,
14.193060788448));
#102456=CARTESIAN_POINT('Ctrl Pts',(-1.95742950579981,2.19830221008539,
14.1880256939819));
#102457=CARTESIAN_POINT('Ctrl Pts',(-1.88584324157823,2.25808752447591,
14.1829905995158));
#102458=CARTESIAN_POINT('Ctrl Pts',(-1.81417833316336,2.31793851861479,
14.1779499735285));
#102459=CARTESIAN_POINT('Ctrl Pts',(-1.73970389906165,2.37433906447225,
14.1729093475411));
#102460=CARTESIAN_POINT('Ctrl Pts',(-1.66279372134582,2.4270313224705,14.1678687215537));
#102461=CARTESIAN_POINT('Ctrl Pts',(-1.58583628226625,2.47975595990209,
14.1628249980978));
#102462=CARTESIAN_POINT('Ctrl Pts',(-1.50644049753725,2.52876753975748,
14.1577812746419));
#102463=CARTESIAN_POINT('Ctrl Pts',(-1.42500637364472,2.57385330488587,
14.1527375511859));
#102464=CARTESIAN_POINT('Ctrl Pts',(-1.34344045975996,2.619012035159,14.1476856651534));
#102465=CARTESIAN_POINT('Ctrl Pts',(-1.25983001907856,2.66023207077413,
14.1426337791208));
#102466=CARTESIAN_POINT('Ctrl Pts',(-1.17459654456991,2.69734813427641,
14.1375818930883));
#102467=CARTESIAN_POINT('Ctrl Pts',(-1.13157530465883,2.71608231215302,
14.1350319747345));
#102468=CARTESIAN_POINT('Ctrl Pts',(-1.08814083723376,2.73377171078363,
14.1324820563807));
#102469=CARTESIAN_POINT('Ctrl Pts',(-1.04434870727625,2.75039993048473,
14.1299321380268));
#102470=CARTESIAN_POINT('Ctrl Pts',(-0.957579893624153,2.78334673846167,
14.1248797829419));
#102471=CARTESIAN_POINT('Ctrl Pts',(-0.869094768662942,2.81224260057255,
14.119827427857));
#102472=CARTESIAN_POINT('Ctrl Pts',(-0.779307222990149,2.83690751562249,
14.1147750727721));
#102473=CARTESIAN_POINT('Ctrl Pts',(-0.689643480660821,2.86153842151307,
14.1097296841149));
#102474=CARTESIAN_POINT('Ctrl Pts',(-0.598681310840846,2.88194985626464,
14.1046842954578));
#102475=CARTESIAN_POINT('Ctrl Pts',(-0.5068534882937,2.89801027282591,14.0996389068006));
#102476=CARTESIAN_POINT('Ctrl Pts',(-0.415123911592111,2.91405350647724,
14.094598916164));
#102477=CARTESIAN_POINT('Ctrl Pts',(-0.322530958285855,2.92575489857701,
14.0895589255274));
#102478=CARTESIAN_POINT('Ctrl Pts',(-0.229520365786315,2.9330333107023,
14.0845189348909));
#102479=CARTESIAN_POINT('Ctrl Pts',(-0.13657678931646,2.94030647858315,
14.0794825756704));
#102480=CARTESIAN_POINT('Ctrl Pts',(-0.0432166133828939,2.94316296624148,
14.0744462164499));
#102481=CARTESIAN_POINT('Ctrl Pts',(0.0501075226029547,2.94157325867954,
14.0694098572294));
#102482=CARTESIAN_POINT('Ctrl Pts',(0.143397743804282,2.93998412883085,
14.0643753282647));
#102483=CARTESIAN_POINT('Ctrl Pts',(0.236651507348711,2.93395202125452,
14.0593407992999));
#102484=CARTESIAN_POINT('Ctrl Pts',(0.329415424340849,2.92349952594597,
14.0543062703352));
#102485=CARTESIAN_POINT('Ctrl Pts',(0.422171578104676,2.91304790538604,
14.0492721627002));
#102486=CARTESIAN_POINT('Ctrl Pts',(0.514437525396893,2.89817668253496,
14.0442380550652));
#102487=CARTESIAN_POINT('Ctrl Pts',(0.605765399102198,2.87896027781742,
14.0392039474303));
#102488=CARTESIAN_POINT('Ctrl Pts',(0.697111175719796,2.85974010612717,
14.0341688529642));
#102489=CARTESIAN_POINT('Ctrl Pts',(0.787518078926407,2.83617315275461,
14.0291337584981));
#102490=CARTESIAN_POINT('Ctrl Pts',(0.87654995273421,2.80838462115887,14.024098664032));
#102491=CARTESIAN_POINT('Ctrl Pts',(0.965679636365806,2.78056556126733,
14.0190580380446));
#102492=CARTESIAN_POINT('Ctrl Pts',(1.05343085055078,2.74851579813489,14.0140174120573));
#102493=CARTESIAN_POINT('Ctrl Pts',(1.13938438647404,2.71240985469733,14.0089767860699));
#102494=CARTESIAN_POINT('Ctrl Pts',(1.2253907409116,2.6762817241296,14.003933062614));
#102495=CARTESIAN_POINT('Ctrl Pts',(1.30959681727519,2.63609264232766,13.9988893391581));
#102496=CARTESIAN_POINT('Ctrl Pts',(1.39160709644178,2.59206359666056,13.9938456157022));
#102497=CARTESIAN_POINT('Ctrl Pts',(1.47375009802917,2.54796329600462,13.9887937296696));
#102498=CARTESIAN_POINT('Ctrl Pts',(1.55368982763823,2.50001085334448,13.9837418436371));
#102499=CARTESIAN_POINT('Ctrl Pts',(1.6310590374262,2.44847103646956,13.9786899576046));
#102500=CARTESIAN_POINT('Ctrl Pts',(1.67011082259928,2.42245652938108,13.9761400392507));
#102501=CARTESIAN_POINT('Ctrl Pts',(1.7085082324844,2.39552872407528,13.9735901208969));
#102502=CARTESIAN_POINT('Ctrl Pts',(1.7462073827726,2.36772544361682,13.971040202543));
#102503=CARTESIAN_POINT('Ctrl Pts',(1.82090369348704,2.31263660314882,13.9659878474581));
#102504=CARTESIAN_POINT('Ctrl Pts',(1.89312458469929,2.25391070546273,13.9609354923732));
#102505=CARTESIAN_POINT('Ctrl Pts',(1.96249455027468,2.19179815223532,13.9558831372882));
#102506=CARTESIAN_POINT('Ctrl Pts',(2.03176886523832,2.12977124275394,13.9508377486311));
#102507=CARTESIAN_POINT('Ctrl Pts',(2.09819973786452,2.06436725075727,13.9457923599739));
#102508=CARTESIAN_POINT('Ctrl Pts',(2.16144216205209,1.99587869874489,13.9407469713168));
#102509=CARTESIAN_POINT('Ctrl Pts',(2.22461692368092,1.92746342208102,13.9357069806802));
#102510=CARTESIAN_POINT('Ctrl Pts',(2.2846097175847,1.8559704695705,13.9306669900436));
#102511=CARTESIAN_POINT('Ctrl Pts',(2.34111088823028,1.78173056577295,13.9256269994071));
#102512=CARTESIAN_POINT('Ctrl Pts',(2.39757134862952,1.70754415334095,13.9205906401866));
#102513=CARTESIAN_POINT('Ctrl Pts',(2.45054491798368,1.63061507612066,13.9155542809661));
#102514=CARTESIAN_POINT('Ctrl Pts',(2.49976159546301,1.55130782433668,13.9105179217456));
#102515=CARTESIAN_POINT('Ctrl Pts',(2.54896038718329,1.4720293934823,13.9054833927809));
#102516=CARTESIAN_POINT('Ctrl Pts',(2.59440476530919,1.39037488207133,13.9004488638161));
#102517=CARTESIAN_POINT('Ctrl Pts',(2.63586812127884,1.30673763519153,13.8954143348514));
#102518=CARTESIAN_POINT('Ctrl Pts',(2.67732800726243,1.22310738774712,13.8903802272164));
#102519=CARTESIAN_POINT('Ctrl Pts',(2.71480733634799,1.137495132841,13.8853461195814));
#102520=CARTESIAN_POINT('Ctrl Pts',(2.74812605854376,1.05031765021481,13.8803120119465));
#102521=CARTESIAN_POINT('Ctrl Pts',(2.78145131217553,0.963123078273342,
13.8752769174804));
#102522=CARTESIAN_POINT('Ctrl Pts',(2.81061418089074,0.874363084317866,
13.8702418230143));
#102523=CARTESIAN_POINT('Ctrl Pts',(2.83548364557246,0.784472112755514,
13.8652067285482));
#102524=CARTESIAN_POINT('Ctrl Pts',(2.8603804316825,0.694482387570324,13.8601661025608));
#102525=CARTESIAN_POINT('Ctrl Pts',(2.88097428003247,0.603359633453046,
13.8551254765735));
#102526=CARTESIAN_POINT('Ctrl Pts',(2.89718480847178,0.51155076537951,13.8500848505861));
#102527=CARTESIAN_POINT('Ctrl Pts',(2.91340529829334,0.41968548068555,13.8450411271302));
#102528=CARTESIAN_POINT('Ctrl Pts',(2.92523704957329,0.327133683002962,
13.8399974036743));
#102529=CARTESIAN_POINT('Ctrl Pts',(2.93265156961317,0.234347543715293,
13.8349536802183));
#102530=CARTESIAN_POINT('Ctrl Pts',(2.94007808903971,0.14141124275094,13.8299017941858));
#102531=CARTESIAN_POINT('Ctrl Pts',(2.94307309153277,0.0482402865086057,
13.8248499081533));
#102532=CARTESIAN_POINT('Ctrl Pts',(2.9416601995369,-0.0447132023066298,
13.8197980221207));
#102533=CARTESIAN_POINT('Ctrl Pts',(2.94094704820904,-0.0916310871635579,
13.8172481037669));
#102534=CARTESIAN_POINT('Ctrl Pts',(2.93911172949345,-0.138493645669141,
13.814698185413));
#102535=CARTESIAN_POINT('Ctrl Pts',(2.93616226480297,-0.185243501227722,
13.8121482670592));
#102536=CARTESIAN_POINT('Ctrl Pts',(2.93031825693337,-0.277872690744211,
13.8070959119743));
#102537=CARTESIAN_POINT('Ctrl Pts',(2.92007610727964,-0.370391264863159,
13.8020435568893));
#102538=CARTESIAN_POINT('Ctrl Pts',(2.90544288901117,-0.46234794115951,
13.7969912018044));
#102539=CARTESIAN_POINT('Ctrl Pts',(2.89082984772084,-0.55417782321183,
13.7919458131473));
#102540=CARTESIAN_POINT('Ctrl Pts',(2.87183783832533,-0.645446912097945,
13.7869004244901));
#102541=CARTESIAN_POINT('Ctrl Pts',(2.84852586141555,-0.735706746500822,
13.7818550358329));
#102542=CARTESIAN_POINT('Ctrl Pts',(2.82523882580154,-0.825870012636004,
13.7768150451964));
#102543=CARTESIAN_POINT('Ctrl Pts',(2.79764111989872,-0.915025742726424,
13.7717750545598));
#102544=CARTESIAN_POINT('Ctrl Pts',(2.76584300519413,-1.00273449657359,
13.7667350639232));
#102545=CARTESIAN_POINT('Ctrl Pts',(2.73406780168002,-1.09038005447396,
13.7616987047027));
#102546=CARTESIAN_POINT('Ctrl Pts',(2.69809835589883,-1.17658029195788,
13.7566623454822));
#102547=CARTESIAN_POINT('Ctrl Pts',(2.65809479261838,-1.26091081106279,
13.7516259862617));
#102548=CARTESIAN_POINT('Ctrl Pts',(2.61810576697296,-1.34521068374006,
13.746591457297));
#102549=CARTESIAN_POINT('Ctrl Pts',(2.57408572646743,-1.42764178691665,
13.7415569283322));
#102550=CARTESIAN_POINT('Ctrl Pts',(2.52624255585271,-1.50780056671921,
13.7365223993675));
#102551=CARTESIAN_POINT('Ctrl Pts',(2.4784033891381,-1.58795263819239,13.7314882917325));
#102552=CARTESIAN_POINT('Ctrl Pts',(2.42674195628704,-1.66583238302116,
13.7264541840975));
#102553=CARTESIAN_POINT('Ctrl Pts',(2.37151106109142,-1.74106268902674,
13.7214200764626));
#102554=CARTESIAN_POINT('Ctrl Pts',(2.31626933903834,-1.8163077423544,13.7163849819965));
#102555=CARTESIAN_POINT('Ctrl Pts',(2.25745702817861,-1.88890196753801,
13.7113498875304));
#102556=CARTESIAN_POINT('Ctrl Pts',(2.19536834045367,-1.95849989781305,
13.7063147930643));
#102557=CARTESIAN_POINT('Ctrl Pts',(2.13321144250977,-2.02817428791091,
13.7012741670769));
#102558=CARTESIAN_POINT('Ctrl Pts',(2.06777127905937,-2.09484548045587,
13.6962335410895));
#102559=CARTESIAN_POINT('Ctrl Pts',(1.99937997416244,-2.15820381774247,
13.6911929151022));
#102560=CARTESIAN_POINT('Ctrl Pts',(1.93094664275576,-2.22160108877634,
13.6861491916463));
#102561=CARTESIAN_POINT('Ctrl Pts',(1.85955889925544,-2.28168116592815,
13.6811054681903));
#102562=CARTESIAN_POINT('Ctrl Pts',(1.78558139424408,-2.33817516121641,
13.6760617447344));
#102563=CARTESIAN_POINT('Ctrl Pts',(1.71148416675828,-2.39476058430973,
13.6710098587019));
#102564=CARTESIAN_POINT('Ctrl Pts',(1.63478917564768,-2.44774808722873,
13.6659579726693));
#102565=CARTESIAN_POINT('Ctrl Pts',(1.55588926093913,-2.49691261514981,
13.6609060866368));
#102566=CARTESIAN_POINT('Ctrl Pts',(1.51606485885711,-2.52172820506945,
13.658356168283));
#102567=CARTESIAN_POINT('Ctrl Pts',(1.47567909360101,-2.5455705570747,13.6558062499291));
#102568=CARTESIAN_POINT('Ctrl Pts',(1.43478453975205,-2.56841533333075,
13.6532563315753));
#102569=CARTESIAN_POINT('Ctrl Pts',(1.35375692301572,-2.61367949690957,
13.6482039764903));
#102570=CARTESIAN_POINT('Ctrl Pts',(1.27043984828923,-2.65518676429196,
13.6431516214054));
#102571=CARTESIAN_POINT('Ctrl Pts',(1.18521648466747,-2.69269862488777,
13.6380992663205));
#102572=CARTESIAN_POINT('Ctrl Pts',(1.10011063107759,-2.73015876234397,
13.6330538776633));
#102573=CARTESIAN_POINT('Ctrl Pts',(1.01310411479439,-2.76363426280696,
13.6280084890062));
#102574=CARTESIAN_POINT('Ctrl Pts',(0.924605862229365,-2.79293179285336,
13.622963100349));
#102575=CARTESIAN_POINT('Ctrl Pts',(0.836202293229886,-2.82219797770903,
13.6179231097124));
#102576=CARTESIAN_POINT('Ctrl Pts',(0.746310579702538,-2.84729493804633,
13.6128831190759));
#102577=CARTESIAN_POINT('Ctrl Pts',(0.655359832737792,-2.86807731583964,
13.6078431284393));
#102578=CARTESIAN_POINT('Ctrl Pts',(0.564474617642048,-2.88884471950569,
13.6028067692188));
#102579=CARTESIAN_POINT('Ctrl Pts',(0.472532317622279,-2.90530362102314,
13.5977704099983));
#102580=CARTESIAN_POINT('Ctrl Pts',(0.379976410158043,-2.91735872455264,
13.5927340507778));
#102581=CARTESIAN_POINT('Ctrl Pts',(0.287454138297511,-2.92940944715503,
13.5876995218131));
#102582=CARTESIAN_POINT('Ctrl Pts',(0.19431914206243,-2.93705949377639,
13.5826649928483));
#102583=CARTESIAN_POINT('Ctrl Pts',(0.101023249077452,-2.94026500559828,
13.5776304638836));
#102584=CARTESIAN_POINT('Ctrl Pts',(0.0077351638408286,-2.94347024915723,
13.5725963562486));
#102585=CARTESIAN_POINT('Ctrl Pts',(-0.085713347389459,-2.94223168238076,
13.5675622486136));
#102586=CARTESIAN_POINT('Ctrl Pts',(-0.178868350977806,-2.93655752761945,
13.5625281409787));
#102587=CARTESIAN_POINT('Ctrl Pts',(-0.272041615648986,-2.93088226055923,
13.5574930465125));
#102588=CARTESIAN_POINT('Ctrl Pts',(-0.364920815042746,-2.9207697060519,
13.5524579520464));
#102589=CARTESIAN_POINT('Ctrl Pts',(-0.45705618546169,-2.90628003525662,
13.5474228575803));
#102590=CARTESIAN_POINT('Ctrl Pts',(-0.549292775185043,-2.89177444620548,
13.542382231593));
#102591=CARTESIAN_POINT('Ctrl Pts',(-0.64078346525242,-2.87288221132512,
13.5373416056056));
#102592=CARTESIAN_POINT('Ctrl Pts',(-0.731088055541054,-2.8497147673136,
13.5323009796183));
#102593=CARTESIAN_POINT('Ctrl Pts',(-0.82144813807025,-2.82653308688982,
13.5272572561624));
#102594=CARTESIAN_POINT('Ctrl Pts',(-0.91062024555729,-2.79907109790597,
13.5222135327065));
#102595=CARTESIAN_POINT('Ctrl Pts',(-0.998180828609589,-2.76748966274425,
13.5171698092505));
#102596=CARTESIAN_POINT('Ctrl Pts',(-1.0858831164905,-2.7358571173489,13.512117923218));
#102597=CARTESIAN_POINT('Ctrl Pts',(-1.17196826360719,-2.70009198666347,
13.5070660371855));
#102598=CARTESIAN_POINT('Ctrl Pts',(-1.25603429571042,-2.66040257254409,
13.5020141511529));
#102599=CARTESIAN_POINT('Ctrl Pts',(-1.2984662739487,-2.64036950670205,
13.4994642327991));
#102600=CARTESIAN_POINT('Ctrl Pts',(-1.34038425681472,-2.61933737659354,
13.4969143144452));
#102601=CARTESIAN_POINT('Ctrl Pts',(-1.38173930724864,-2.59733719158758,
13.4943643960914));
#102602=CARTESIAN_POINT('Ctrl Pts',(-1.46367934232157,-2.55374648350997,
13.4893120410065));
#102603=CARTESIAN_POINT('Ctrl Pts',(-1.54370159831407,-2.50619622870097,
13.4842596859216));
#102604=CARTESIAN_POINT('Ctrl Pts',(-1.62139802903702,-2.45487931097129,
13.4792073308366));
#102605=CARTESIAN_POINT('Ctrl Pts',(-1.69898732822169,-2.40363315145129,
13.4741619421795));
#102606=CARTESIAN_POINT('Ctrl Pts',(-1.77425680730785,-2.3486308921786,
13.4691165535223));
#102607=CARTESIAN_POINT('Ctrl Pts',(-1.84682244245705,-2.29011154008641,
13.4640711648652));
#102608=CARTESIAN_POINT('Ctrl Pts',(-1.91931044021938,-2.23165479737632,
13.4590311742286));
#102609=CARTESIAN_POINT('Ctrl Pts',(-1.98910000002059,-2.16968871857654,
13.453991183592));
#102610=CARTESIAN_POINT('Ctrl Pts',(-2.05583649115529,-2.10449526529149,
13.4489511929554));
#102611=CARTESIAN_POINT('Ctrl Pts',(-2.12252489728635,-2.03934878521983,
13.4439148337349));
#102612=CARTESIAN_POINT('Ctrl Pts',(-2.18616429029692,-1.97097986224065,
13.4388784745144));
#102613=CARTESIAN_POINT('Ctrl Pts',(-2.24643433844286,-1.89970965230606,
13.4338421152939));
#102614=CARTESIAN_POINT('Ctrl Pts',(-2.30668248394084,-1.82846534257174,
13.4288075863292));
#102615=CARTESIAN_POINT('Ctrl Pts',(-2.36356343050931,-1.75432217933678,
13.4237730573645));
#102616=CARTESIAN_POINT('Ctrl Pts',(-2.41679555997163,-1.67763620052185,
13.4187385283997));
#102617=CARTESIAN_POINT('Ctrl Pts',(-2.47002323454262,-1.6009566394044,
13.4137044207648));
#102618=CARTESIAN_POINT('Ctrl Pts',(-2.5196024459703,-1.52173505085027,
13.4086703131298));
#102619=CARTESIAN_POINT('Ctrl Pts',(-2.56529421349996,-1.44035745500332,
13.4036362054948));
#102620=CARTESIAN_POINT('Ctrl Pts',(-2.61099493794135,-1.3589639067872,
13.3986011110287));
#102621=CARTESIAN_POINT('Ctrl Pts',(-2.65280648788912,-1.27541389942849,
13.3935660165626));
#102622=CARTESIAN_POINT('Ctrl Pts',(-2.69053580838343,-1.19011808817719,
13.3885309220965));
#102623=CARTESIAN_POINT('Ctrl Pts',(-2.72830657805803,-1.10472857151557,
13.3834902961092));
#102624=CARTESIAN_POINT('Ctrl Pts',(-2.76198598629454,-1.01758982945085,
13.3784496701218));
#102625=CARTESIAN_POINT('Ctrl Pts',(-2.79142925127766,-0.929132248450908,
13.3734090441344));
#102626=CARTESIAN_POINT('Ctrl Pts',(-2.8208906091699,-0.840620310198972,
13.3683653206785));
#102627=CARTESIAN_POINT('Ctrl Pts',(-2.84611052153083,-0.750788346994598,
13.3633215972226));
#102628=CARTESIAN_POINT('Ctrl Pts',(-2.8669947722064,-0.660079522588877,
13.3582778737667));
#102629=CARTESIAN_POINT('Ctrl Pts',(-2.88791282118546,-0.569223898356644,
13.3532259877341));
#102630=CARTESIAN_POINT('Ctrl Pts',(-2.90448112172261,-0.477489016526742,
13.3481741017016));
#102631=CARTESIAN_POINT('Ctrl Pts',(-2.91665702127834,-0.385325602870807,
13.3431222156691));
#102632=CARTESIAN_POINT('Ctrl Pts',(-2.92280275567371,-0.33880650514767,
13.3405722973152));
#102633=CARTESIAN_POINT('Ctrl Pts',(-2.9278302724095,-0.292178274858314,
13.3380223789614));
#102634=CARTESIAN_POINT('Ctrl Pts',(-2.93173912842756,-0.2454988448992,
13.3354724606075));
#102635=CARTESIAN_POINT('Ctrl Pts',(-2.93853326653527,-0.164363471156356,
13.3310403461016));
#102636=CARTESIAN_POINT('Ctrl Pts',(-2.94195988097664,-0.082942196459933,
13.3266082315956));
#102637=CARTESIAN_POINT('Ctrl Pts',(-2.941999649804,-0.00143546270055514,
13.3221761170896));
#102638=CARTESIAN_POINT('',(-2.94199943776035,-0.00181885067937308,12.3221761170896));
#102639=CARTESIAN_POINT('Ctrl Pts',(-2.94597788009644,-0.00141238427974306,
13.3221747584359));
#102640=CARTESIAN_POINT('Ctrl Pts',(-2.94060189892318,0.892291696921148,
13.2736433473318));
#102641=CARTESIAN_POINT('Ctrl Pts',(-2.0297603205157,2.77078909882355,13.172147957733));
#102642=CARTESIAN_POINT('Ctrl Pts',(1.16765677021709,3.2763543727395,13.0176885896398));
#102643=CARTESIAN_POINT('Ctrl Pts',(3.38653851180909,0.793269952057298,
12.8587966541559));
#102644=CARTESIAN_POINT('Ctrl Pts',(2.50126568019329,-2.41693820895166,
12.6999047186721));
#102645=CARTESIAN_POINT('Ctrl Pts',(-0.676706694895887,-3.41174271566395,
12.5410127831881));
#102646=CARTESIAN_POINT('Ctrl Pts',(-2.70347308096043,-1.72194475430307,
12.4151036473877));
#102647=CARTESIAN_POINT('Ctrl Pts',(-2.9404125071609,-0.372252179371909,
12.3421584900819));
#102648=CARTESIAN_POINT('Ctrl Pts',(-2.93832851344324,-0.00183871897317971,
12.3221773112706));
#102649=CARTESIAN_POINT('',(-2.94199908735515,0.00231732635699392,11.3221761170896));
#102650=CARTESIAN_POINT('Ctrl Pts',(-2.94199943776035,-0.00181885067937308,
12.3221761170896));
#102651=CARTESIAN_POINT('Ctrl Pts',(-2.94205766824479,0.0923692288830542,
12.317101658888));
#102652=CARTESIAN_POINT('Ctrl Pts',(-2.93758841679311,0.186573850448379,
12.3120272006865));
#102653=CARTESIAN_POINT('Ctrl Pts',(-2.92861347223371,0.280333962001044,
12.3069527424849));
#102654=CARTESIAN_POINT('Ctrl Pts',(-2.9196373468526,0.374106409448843,
12.3018776166435));
#102655=CARTESIAN_POINT('Ctrl Pts',(-2.90615439122099,0.467433798315638,
12.2968024908021));
#102656=CARTESIAN_POINT('Ctrl Pts',(-2.88823823698857,0.559860595503181,
12.2917273649607));
#102657=CARTESIAN_POINT('Ctrl Pts',(-2.87031501762493,0.65232384066058,
12.286650237773));
#102658=CARTESIAN_POINT('Ctrl Pts',(-2.84795520670616,0.743885361994522,
12.2815731105852));
#102659=CARTESIAN_POINT('Ctrl Pts',(-2.82128325111986,0.834101203062655,
12.2764959833975));
#102660=CARTESIAN_POINT('Ctrl Pts',(-2.79457535859223,0.924438598074477,
12.2714120154507));
#102661=CARTESIAN_POINT('Ctrl Pts',(-2.76354384624255,1.01342627637935,
12.2663280475039));
#102662=CARTESIAN_POINT('Ctrl Pts',(-2.72836260045467,1.10063687038016,
12.2612440795571));
#102663=CARTESIAN_POINT('Ctrl Pts',(-2.69315476612227,1.18791337457571,
12.2561562693556));
#102664=CARTESIAN_POINT('Ctrl Pts',(-2.65379113463881,1.27340972623707,
12.251068459154));
#102665=CARTESIAN_POINT('Ctrl Pts',(-2.61049222133598,1.35672191783886,
12.2459806489525));
#102666=CARTESIAN_POINT('Ctrl Pts',(-2.56711616167106,1.4401825480967,12.2408837737187));
#102667=CARTESIAN_POINT('Ctrl Pts',(-2.51979103835353,1.52145087340081,
12.2357868984848));
#102668=CARTESIAN_POINT('Ctrl Pts',(-2.46878144487779,1.60015067335146,
12.230690023251));
#102669=CARTESIAN_POINT('Ctrl Pts',(-2.44389114620892,1.63855249921357,
12.2282029862408));
#102670=CARTESIAN_POINT('Ctrl Pts',(-2.41812420531121,1.67634324929415,
12.2257159492306));
#102671=CARTESIAN_POINT('Ctrl Pts',(-2.39151476236182,1.71348216839438,
12.2232289122205));
#102672=CARTESIAN_POINT('Ctrl Pts',(-2.33745832739843,1.78892897758803,
12.2181765571355));
#102673=CARTESIAN_POINT('Ctrl Pts',(-2.27973113806503,1.86195061683415,
12.2131242020506));
#102674=CARTESIAN_POINT('Ctrl Pts',(-2.21857840853751,1.9321681720728,12.2080718469657));
#102675=CARTESIAN_POINT('Ctrl Pts',(-2.15750999930541,2.00228890800271,
12.2030264583086));
#102676=CARTESIAN_POINT('Ctrl Pts',(-2.09302572490762,2.06961291087218,
12.1979810696514));
#102677=CARTESIAN_POINT('Ctrl Pts',(-2.02541333578534,2.13379118454053,
12.1929356809943));
#102678=CARTESIAN_POINT('Ctrl Pts',(-1.95787328461187,2.19790079439246,
12.1878956903577));
#102679=CARTESIAN_POINT('Ctrl Pts',(-1.8872120913524,2.25887106047546,12.1828556997211));
#102680=CARTESIAN_POINT('Ctrl Pts',(-1.81375619102398,2.3163878085334,12.1778157090845));
#102681=CARTESIAN_POINT('Ctrl Pts',(-1.74035321717071,2.37386311460067,
12.172779349864));
#102682=CARTESIAN_POINT('Ctrl Pts',(-1.66415988741759,2.42788957546218,
12.1677429906435));
#102683=CARTESIAN_POINT('Ctrl Pts',(-1.58553694457079,2.47819220348244,
12.162706631423));
#102684=CARTESIAN_POINT('Ctrl Pts',(-1.5069425739699,2.52847655109998,12.1576721024583));
#102685=CARTESIAN_POINT('Ctrl Pts',(-1.42592071816484,2.57503951512635,
12.1526375734935));
#102686=CARTESIAN_POINT('Ctrl Pts',(-1.34286156881112,2.61764909928931,
12.1476030445288));
#102687=CARTESIAN_POINT('Ctrl Pts',(-1.25980937051293,2.66025511754065,
12.1425689368938));
#102688=CARTESIAN_POINT('Ctrl Pts',(-1.17472061300241,2.6989082111315,12.1375348292588));
#102689=CARTESIAN_POINT('Ctrl Pts',(-1.08800956062951,2.73342261569242,
12.1325007216238));
#102690=CARTESIAN_POINT('Ctrl Pts',(-1.00128151037501,2.76794378607783,
12.1274656271577));
#102691=CARTESIAN_POINT('Ctrl Pts',(-0.91293094653178,2.7983244922465,12.1224305326916));
#102692=CARTESIAN_POINT('Ctrl Pts',(-0.82339047069958,2.8244277531495,12.1173954382255));
#102693=CARTESIAN_POINT('Ctrl Pts',(-0.73375162629706,2.85055969092105,
12.1123548122381));
#102694=CARTESIAN_POINT('Ctrl Pts',(-0.642920687670014,2.87240467881097,
12.1073141862508));
#102695=CARTESIAN_POINT('Ctrl Pts',(-0.551343422148798,2.88987619645777,
12.1022735602634));
#102696=CARTESIAN_POINT('Ctrl Pts',(-0.459709882327092,2.90735845036569,
12.0972298368075));
#102697=CARTESIAN_POINT('Ctrl Pts',(-0.367329542101543,2.92046182139928,
12.0921861133516));
#102698=CARTESIAN_POINT('Ctrl Pts',(-0.274654138277992,2.92915160145848,
12.0871423898957));
#102699=CARTESIAN_POINT('Ctrl Pts',(-0.18182875198803,2.93785544473825,
12.0820905038631));
#102700=CARTESIAN_POINT('Ctrl Pts',(-0.0887077920051848,2.94213141701459,
12.0770386178306));
#102701=CARTESIAN_POINT('Ctrl Pts',(0.00425633687013605,2.94199692107188,
12.071986731798));
#102702=CARTESIAN_POINT('Ctrl Pts',(0.0511795922524226,2.94192903480711,
12.0694368134442));
#102703=CARTESIAN_POINT('Ctrl Pts',(0.0980629581512809,2.94073832643697,
12.0668868950904));
#102704=CARTESIAN_POINT('Ctrl Pts',(0.14484895308894,2.9384320275938,12.0643369767366));
#102705=CARTESIAN_POINT('Ctrl Pts',(0.237549748419017,2.93386237513018,
12.0592846216516));
#102706=CARTESIAN_POINT('Ctrl Pts',(0.330200420451757,2.92489347562024,
12.0542322665667));
#102707=CARTESIAN_POINT('Ctrl Pts',(0.42234963216692,2.91152619569333,12.0491799114818));
#102708=CARTESIAN_POINT('Ctrl Pts',(0.514371784161062,2.8981773472085,12.0441345228246));
#102709=CARTESIAN_POINT('Ctrl Pts',(0.605893413987775,2.88044223286289,
12.0390891341675));
#102710=CARTESIAN_POINT('Ctrl Pts',(0.69646529138112,2.85837368059206,12.0340437455103));
#102711=CARTESIAN_POINT('Ctrl Pts',(0.78694026665451,2.83632873928704,12.0290037548737));
#102712=CARTESIAN_POINT('Ctrl Pts',(0.876467079918468,2.80995968003446,
12.0239637642371));
#102713=CARTESIAN_POINT('Ctrl Pts',(0.964604816251452,2.77937071087405,
12.0189237736005));
#102714=CARTESIAN_POINT('Ctrl Pts',(1.05267904754699,2.74880378169006,12.0138874143801));
#102715=CARTESIAN_POINT('Ctrl Pts',(1.13936577278185,2.71402313132016,12.0088510551596));
#102716=CARTESIAN_POINT('Ctrl Pts',(1.22423843214642,2.67518303322514,12.0038146959391));
#102717=CARTESIAN_POINT('Ctrl Pts',(1.30908024806488,2.63635704995205,11.9987801669743));
#102718=CARTESIAN_POINT('Ctrl Pts',(1.39210890423529,2.59347473434825,11.9937456380096));
#102719=CARTESIAN_POINT('Ctrl Pts',(1.47291802618841,2.54673840198188,11.9887111090449));
#102720=CARTESIAN_POINT('Ctrl Pts',(1.55372038538624,2.50000598088657,11.9836770014099));
#102721=CARTESIAN_POINT('Ctrl Pts',(1.63230319521567,2.44942040687475,11.9786428937749));
#102722=CARTESIAN_POINT('Ctrl Pts',(1.70828590269151,2.39522927392462,11.9736087861399));
#102723=CARTESIAN_POINT('Ctrl Pts',(1.78428350498215,2.34102751794043,11.9685736916738));
#102724=CARTESIAN_POINT('Ctrl Pts',(1.85767963122038,2.28321905755688,11.9635385972077));
#102725=CARTESIAN_POINT('Ctrl Pts',(1.92812480141315,2.22209332616241,11.9585035027416));
#102726=CARTESIAN_POINT('Ctrl Pts',(1.99864736220074,2.16090044244651,11.9534628767543));
#102727=CARTESIAN_POINT('Ctrl Pts',(2.06621215968135,2.09638330480715,11.9484222507669));
#102728=CARTESIAN_POINT('Ctrl Pts',(2.13050499818133,2.02886974759948,11.9433816247796));
#102729=CARTESIAN_POINT('Ctrl Pts',(2.19483734468032,1.96131470325866,11.9383379013237));
#102730=CARTESIAN_POINT('Ctrl Pts',(2.25589343896197,1.89075990934853,11.9332941778677));
#102731=CARTESIAN_POINT('Ctrl Pts',(2.31339940392865,1.81756628432158,11.9282504544118));
#102732=CARTESIAN_POINT('Ctrl Pts',(2.37099843443491,1.74425420542274,11.9231985683793));
#102733=CARTESIAN_POINT('Ctrl Pts',(2.42503560847699,1.66829513125387,11.9181466823467));
#102734=CARTESIAN_POINT('Ctrl Pts',(2.47528049031936,1.59007876982379,11.9130947963142));
#102735=CARTESIAN_POINT('Ctrl Pts',(2.500641384364,1.55059938840126,11.9105448779604));
#102736=CARTESIAN_POINT('Ctrl Pts',(2.52503685218335,1.51054531327355,11.9079949596065));
#102737=CARTESIAN_POINT('Ctrl Pts',(2.54844183525752,1.4699687793655,11.9054450412527));
#102738=CARTESIAN_POINT('Ctrl Pts',(2.59481598095077,1.38957128071249,11.9003926861678));
#102739=CARTESIAN_POINT('Ctrl Pts',(2.63746506948364,1.30683287709102,11.8953403310828));
#102740=CARTESIAN_POINT('Ctrl Pts',(2.67614534361757,1.22213342145365,11.8902879759979));
#102741=CARTESIAN_POINT('Ctrl Pts',(2.71477228354784,1.1375507534585,11.8852425873407));
#102742=CARTESIAN_POINT('Ctrl Pts',(2.74944110048464,1.05101280721965,11.8801971986836));
#102743=CARTESIAN_POINT('Ctrl Pts',(2.77995285587913,0.962925811830535,
11.8751518100264));
#102744=CARTESIAN_POINT('Ctrl Pts',(2.81043196699289,0.874933060006497,
11.8701118193898));
#102745=CARTESIAN_POINT('Ctrl Pts',(2.83676271224308,0.78539497071694,11.8650718287532));
#102746=CARTESIAN_POINT('Ctrl Pts',(2.85879384636977,0.69473861556585,11.8600318381167));
#102747=CARTESIAN_POINT('Ctrl Pts',(2.88080910661477,0.604147580168466,
11.8549954788962));
#102748=CARTESIAN_POINT('Ctrl Pts',(2.89853080876147,0.512440310854052,
11.8499591196757));
#102749=CARTESIAN_POINT('Ctrl Pts',(2.91185756744108,0.420058932694123,
11.8449227604552));
#102750=CARTESIAN_POINT('Ctrl Pts',(2.92517948306328,0.32771112671245,11.8398882314904));
#102751=CARTESIAN_POINT('Ctrl Pts',(2.93410956478644,0.234690137804377,
11.8348537025257));
#102752=CARTESIAN_POINT('Ctrl Pts',(2.93859774457073,0.141447147740094,
11.829819173561));
#102753=CARTESIAN_POINT('Ctrl Pts',(2.94308554874817,0.0482119609966004,
11.824785065926));
#102754=CARTESIAN_POINT('Ctrl Pts',(2.94313216890858,-0.0452447462288223,
11.819750958291));
#102755=CARTESIAN_POINT('Ctrl Pts',(2.93873958429541,-0.138468970152959,
11.814716850656));
#102756=CARTESIAN_POINT('Ctrl Pts',(2.93434613860826,-0.231711468728897,
11.8096817561899));
#102757=CARTESIAN_POINT('Ctrl Pts',(2.92551178117756,-0.324720949791183,
11.8046466617238));
#102758=CARTESIAN_POINT('Ctrl Pts',(2.91229049248657,-0.417046864719446,
11.7996115672577));
#102759=CARTESIAN_POINT('Ctrl Pts',(2.89905467897586,-0.509474208283074,
11.7945709412703));
#102760=CARTESIAN_POINT('Ctrl Pts',(2.88142237708944,-0.601216046274095,
11.789530315283));
#102761=CARTESIAN_POINT('Ctrl Pts',(2.85949895951669,-0.691830687757469,
11.7844896892956));
#102762=CARTESIAN_POINT('Ctrl Pts',(2.83756206998686,-0.782501012008185,
11.7794459658397));
#102763=CARTESIAN_POINT('Ctrl Pts',(2.81132894003605,-0.872042334790647,
11.7744022423838));
#102764=CARTESIAN_POINT('Ctrl Pts',(2.78095459233893,-0.960028934641571,
11.7693585189279));
#102765=CARTESIAN_POINT('Ctrl Pts',(2.75053108791417,-1.04815792877096,
11.7643066328953));
#102766=CARTESIAN_POINT('Ctrl Pts',(2.71595315063959,-1.13472676485469,
11.7592547468628));
#102767=CARTESIAN_POINT('Ctrl Pts',(2.67742353487152,-1.21933064216237,
11.7542028608302));
#102768=CARTESIAN_POINT('Ctrl Pts',(2.65797587239862,-1.26203409551843,
11.7516529424764));
#102769=CARTESIAN_POINT('Ctrl Pts',(2.63752217185223,-1.30423734087188,
11.7491030241226));
#102770=CARTESIAN_POINT('Ctrl Pts',(2.61609276670458,-1.34589101936076,
11.7465531057688));
#102771=CARTESIAN_POINT('Ctrl Pts',(2.57363298994241,-1.42842274983934,
11.7415007506839));
#102772=CARTESIAN_POINT('Ctrl Pts',(2.52718766825847,-1.50909133282075,
11.7364483955989));
#102773=CARTESIAN_POINT('Ctrl Pts',(2.47694405592248,-1.58748610823222,
11.731396040514));
#102774=CARTESIAN_POINT('Ctrl Pts',(2.42676972187185,-1.6657727891941,11.7263506518569));
#102775=CARTESIAN_POINT('Ctrl Pts',(2.37280774191927,-1.74179152192844,
11.7213052631997));
#102776=CARTESIAN_POINT('Ctrl Pts',(2.31529181944221,-1.81515503217328,
11.7162598745426));
#102777=CARTESIAN_POINT('Ctrl Pts',(2.25783743278584,-1.88844005139133,
11.711219883906));
#102778=CARTESIAN_POINT('Ctrl Pts',(2.19683693394232,-1.95907514691681,
11.7061798932694));
#102779=CARTESIAN_POINT('Ctrl Pts',(2.13256738110225,-2.02670184414449,
11.7011399026328));
#102780=CARTESIAN_POINT('Ctrl Pts',(2.06834413578643,-2.0942798149569,11.6961035434124));
#102781=CARTESIAN_POINT('Ctrl Pts',(2.00085682335587,-2.1588533748168,11.6910671841919));
#102782=CARTESIAN_POINT('Ctrl Pts',(1.93042216430952,-2.22009780585058,
11.6860308249714));
#102783=CARTESIAN_POINT('Ctrl Pts',(1.86001310181708,-2.28131998013744,
11.6809962960067));
#102784=CARTESIAN_POINT('Ctrl Pts',(1.78665915544363,-2.33921513786641,
11.6759617670419));
#102785=CARTESIAN_POINT('Ctrl Pts',(1.71071245673316,-2.39349679138661,
11.6709272380772));
#102786=CARTESIAN_POINT('Ctrl Pts',(1.63477211385139,-2.4477739021828,11.6658931304422));
#102787=CARTESIAN_POINT('Ctrl Pts',(1.55623981156895,-2.49843785186136,
11.6608590228072));
#102788=CARTESIAN_POINT('Ctrl Pts',(1.4754982471522,-2.54524437385702,11.6558249151723));
#102789=CARTESIAN_POINT('Ctrl Pts',(1.3947408550467,-2.59206007128872,11.6507898207062));
#102790=CARTESIAN_POINT('Ctrl Pts',(1.3117737252013,-2.63501661681924,11.6457547262401));
#102791=CARTESIAN_POINT('Ctrl Pts',(1.22700481921386,-2.67391532656252,
11.640719631774));
#102792=CARTESIAN_POINT('Ctrl Pts',(1.14214278667079,-2.7128567701693,11.6356790057866));
#102793=CARTESIAN_POINT('Ctrl Pts',(1.05547543121897,-2.7477312939191,11.6306383797993));
#102794=CARTESIAN_POINT('Ctrl Pts',(0.967431107643021,-2.77838821116931,
11.6255977538119));
#102795=CARTESIAN_POINT('Ctrl Pts',(0.879332680762282,-2.80906396711883,
11.620554030356));
#102796=CARTESIAN_POINT('Ctrl Pts',(0.789856026937357,-2.83551683110188,
11.6155103069001));
#102797=CARTESIAN_POINT('Ctrl Pts',(0.699442972388415,-2.8576465016472,
11.6104665834442));
#102798=CARTESIAN_POINT('Ctrl Pts',(0.608883596675779,-2.87981198603779,
11.6054146974116));
#102799=CARTESIAN_POINT('Ctrl Pts',(0.51738523035346,-2.89764022452043,
11.6003628113791));
#102800=CARTESIAN_POINT('Ctrl Pts',(0.425397970031113,-2.91108237037247,
11.5953109253466));
#102801=CARTESIAN_POINT('Ctrl Pts',(0.378967784966315,-2.91786723729199,
11.5927610069927));
#102802=CARTESIAN_POINT('Ctrl Pts',(0.332413100333541,-2.92353549303978,
11.5902110886388));
#102803=CARTESIAN_POINT('Ctrl Pts',(0.285791837458446,-2.92808589792754,
11.587661170285));
#102804=CARTESIAN_POINT('Ctrl Pts',(0.19341743880498,-2.93710197533974,
11.5826088152));
#102805=CARTESIAN_POINT('Ctrl Pts',(0.100450220757555,-2.94175864314905,
11.5775564601151));
#102806=CARTESIAN_POINT('Ctrl Pts',(0.00733680887932632,-2.94199085165734,
11.5725041050302));
#102807=CARTESIAN_POINT('Ctrl Pts',(-0.085648213792534,-2.94222273998547,
11.567458716373));
#102808=CARTESIAN_POINT('Ctrl Pts',(-0.17877858934624,-2.938042290704,11.5624133277159));
#102809=CARTESIAN_POINT('Ctrl Pts',(-0.271602188677053,-2.9294361660746,
11.5573679390587));
#102810=CARTESIAN_POINT('Ctrl Pts',(-0.364326476789299,-2.92083924906836,
11.5523279484221));
#102811=CARTESIAN_POINT('Ctrl Pts',(-0.456744201093304,-2.90782610903195,
11.5472879577855));
#102812=CARTESIAN_POINT('Ctrl Pts',(-0.548403955851965,-2.89043545183177,
11.5422479671489));
#102813=CARTESIAN_POINT('Ctrl Pts',(-0.63999766788659,-2.87305732495503,
11.5372116079284));
#102814=CARTESIAN_POINT('Ctrl Pts',(-0.730834060691916,-2.85130803268609,
11.5321752487079));
#102815=CARTESIAN_POINT('Ctrl Pts',(-0.820468618902273,-2.8252779058699,
11.5271388894874));
#102816=CARTESIAN_POINT('Ctrl Pts',(-0.910070603152004,-2.79925723862313,
11.5221043605227));
#102817=CARTESIAN_POINT('Ctrl Pts',(-0.998471194286752,-2.76895895114635,
11.517069831558));
#102818=CARTESIAN_POINT('Ctrl Pts',(-1.08523883050169,-2.73452384900394,
11.5120353025932));
#102819=CARTESIAN_POINT('Ctrl Pts',(-1.17199920530529,-2.70009162866692,
11.5070011949583));
#102820=CARTESIAN_POINT('Ctrl Pts',(-1.2571264840562,-2.66152344603806,
11.5019670873233));
#102821=CARTESIAN_POINT('Ctrl Pts',(-1.34020803781096,-2.61900867035352,
11.4969329796883));
#102822=CARTESIAN_POINT('Ctrl Pts',(-1.4233058779603,-2.57648556053966,
11.4918978852222));
#102823=CARTESIAN_POINT('Ctrl Pts',(-1.50435680140709,-2.53001452389156,
11.4868627907561));
#102824=CARTESIAN_POINT('Ctrl Pts',(-1.58297280946911,-2.47983085803881,
11.4818276962899));
#102825=CARTESIAN_POINT('Ctrl Pts',(-1.66167518455394,-2.429592060745,11.4767870703026));
#102826=CARTESIAN_POINT('Ctrl Pts',(-1.73793692964973,-2.37563273214714,
11.4717464443152));
#102827=CARTESIAN_POINT('Ctrl Pts',(-1.81139934462327,-2.31823131164653,
11.4667058183279));
#102828=CARTESIAN_POINT('Ctrl Pts',(-1.88490690230741,-2.2607946179288,
11.461662094872));
#102829=CARTESIAN_POINT('Ctrl Pts',(-1.95561136892047,-2.19991191107742,
11.4566183714161));
#102830=CARTESIAN_POINT('Ctrl Pts',(-2.02318909957356,-2.13590024752251,
11.4515746479602));
#102831=CARTESIAN_POINT('Ctrl Pts',(-2.09087619554172,-2.07178498984443,
11.4465227619276));
#102832=CARTESIAN_POINT('Ctrl Pts',(-2.1554261462877,-2.00453098635218,
11.4414708758951));
#102833=CARTESIAN_POINT('Ctrl Pts',(-2.21655407859464,-1.93449011800667,
11.4364189898625));
#102834=CARTESIAN_POINT('Ctrl Pts',(-2.24740814686075,-1.89913728253861,
11.4338690715087));
#102835=CARTESIAN_POINT('Ctrl Pts',(-2.27739105792315,-1.86307493612799,
11.4313191531549));
#102836=CARTESIAN_POINT('Ctrl Pts',(-2.30647039420271,-1.82635109457803,
11.4287692348011));
#102837=CARTESIAN_POINT('Ctrl Pts',(-2.36400612788006,-1.75369011130406,
11.4237240225619));
#102838=CARTESIAN_POINT('Ctrl Pts',(-2.41821268241222,-1.67817153783343,
11.4186788103228));
#102839=CARTESIAN_POINT('Ctrl Pts',(-2.46879265417749,-1.6001333790279,
11.4136335980836));
#102840=CARTESIAN_POINT('Ctrl Pts',(-2.51930480111526,-1.52219986489644,
11.4085951511833));
#102841=CARTESIAN_POINT('Ctrl Pts',(-2.56619978421412,-1.44175384536167,
11.4035567042831));
#102842=CARTESIAN_POINT('Ctrl Pts',(-2.60922039845594,-1.3591662563062,
11.3985182573828));
#102843=CARTESIAN_POINT('Ctrl Pts',(-2.65219541974529,-1.27666619301227,
11.393485150194));
#102844=CARTESIAN_POINT('Ctrl Pts',(-2.69130402539409,-1.19202946153317,
11.3884520430053));
#102845=CARTESIAN_POINT('Ctrl Pts',(-2.72633294005123,-1.10565487381534,
11.3834189358166));
#102846=CARTESIAN_POINT('Ctrl Pts',(-2.76185224237784,-1.01807108412288,
11.3783153675893));
#102847=CARTESIAN_POINT('Ctrl Pts',(-2.79317649350139,-0.928700795946386,
11.3732117993621));
#102848=CARTESIAN_POINT('Ctrl Pts',(-2.82013231123186,-0.8379843358596,
11.3681082311348));
#102849=CARTESIAN_POINT('Ctrl Pts',(-2.84668412971332,-0.748627485119997,
11.363081152434));
#102850=CARTESIAN_POINT('Ctrl Pts',(-2.86899744628251,-0.657964982397529,
11.3580540737331));
#102851=CARTESIAN_POINT('Ctrl Pts',(-2.88695609225618,-0.56643492246236,
11.3530269950322));
#102852=CARTESIAN_POINT('Ctrl Pts',(-2.90532461295226,-0.47281584880292,
11.3478851820418));
#102853=CARTESIAN_POINT('Ctrl Pts',(-2.91913711330609,-0.378289593421233,
11.3427433690513));
#102854=CARTESIAN_POINT('Ctrl Pts',(-2.92832451093351,-0.283336476059814,
11.3376015560609));
#102855=CARTESIAN_POINT('Ctrl Pts',(-2.93751190856094,-0.188383358698396,
11.3324597430705));
#102856=CARTESIAN_POINT('Ctrl Pts',(-2.94207416906968,-0.0930038764377092,
11.32731793008));
#102857=CARTESIAN_POINT('Ctrl Pts',(-2.94199908735515,0.00231732635699392,
11.3221761170896));
#102858=CARTESIAN_POINT('',(-2.94239657372082,0.000640158651710834,10.3221761814368));
#102859=CARTESIAN_POINT('Ctrl Pts',(-2.93935298557806,0.00233601540201734,
11.3221749955287));
#102860=CARTESIAN_POINT('Ctrl Pts',(-2.94172337671491,0.325219974538946,
11.3047424301248));
#102861=CARTESIAN_POINT('Ctrl Pts',(-2.74371032010323,1.6262663578991,11.2343458862266));
#102862=CARTESIAN_POINT('Ctrl Pts',(-0.839765383495511,3.3753095279522,
11.1109853638332));
#102863=CARTESIAN_POINT('Ctrl Pts',(2.38231317487652,2.53426601713663,10.9520934283495));
#102864=CARTESIAN_POINT('Ctrl Pts',(3.42072593089031,-0.62972566609421,
10.7932014928655));
#102865=CARTESIAN_POINT('Ctrl Pts',(1.32364738655828,-3.21650087903925,
10.6343095573817));
#102866=CARTESIAN_POINT('Ctrl Pts',(-1.94746159165213,-2.85926666405493,
10.4773013514598));
#102867=CARTESIAN_POINT('Ctrl Pts',(-2.94388221610062,-0.939423273160714,
10.3732571240324));
#102868=CARTESIAN_POINT('Ctrl Pts',(-2.94667239079342,0.000628324869612199,
10.3221768750997));
#102869=CARTESIAN_POINT('',(-2.94199877210839,-0.00268791977826042,9.32217614139002));
#102870=CARTESIAN_POINT('Ctrl Pts',(-2.94199993011391,0.000641256405411553,
10.3221761170896));
#102871=CARTESIAN_POINT('Ctrl Pts',(-2.94199238686346,0.0352486959386637,
10.3202926401977));
#102872=CARTESIAN_POINT('Ctrl Pts',(-2.94137422245853,0.0698487503835785,
10.3184091633059));
#102873=CARTESIAN_POINT('Ctrl Pts',(-2.94014608467686,0.104427011636639,
10.3165256864141));
#102874=CARTESIAN_POINT('Ctrl Pts',(-2.93685165181546,0.19718188153905,
10.3114733313293));
#102875=CARTESIAN_POINT('Ctrl Pts',(-2.92915769861534,0.289947129723463,
10.3064209762446));
#102876=CARTESIAN_POINT('Ctrl Pts',(-2.91705888500192,0.382271449929681,
10.3013686211598));
#102877=CARTESIAN_POINT('Ctrl Pts',(-2.90497675380882,0.474468468966993,
10.2963232325027));
#102878=CARTESIAN_POINT('Ctrl Pts',(-2.88850188851419,0.566225331492591,
10.2912778438456));
#102879=CARTESIAN_POINT('Ctrl Pts',(-2.8676809344076,0.65709212324846,10.2862324551885));
#102880=CARTESIAN_POINT('Ctrl Pts',(-2.84688225647159,0.747861697357949,
10.281192464552));
#102881=CARTESIAN_POINT('Ctrl Pts',(-2.82174683069095,0.837742662806323,
10.2761524739154));
#102882=CARTESIAN_POINT('Ctrl Pts',(-2.79237279195056,0.926292713333228,
10.2711124832788));
#102883=CARTESIAN_POINT('Ctrl Pts',(-2.76301991780447,1.01477896174185,
10.2660761240583));
#102884=CARTESIAN_POINT('Ctrl Pts',(-2.7294346404374,1.1019357808457,10.2610397648378));
#102885=CARTESIAN_POINT('Ctrl Pts',(-2.69176535282754,1.18733452965761,
10.2560034056173));
#102886=CARTESIAN_POINT('Ctrl Pts',(-2.65410975455708,1.27270224383808,
10.2509688766525));
#102887=CARTESIAN_POINT('Ctrl Pts',(-2.6123732736043,1.35631275092138,10.2459343476877));
#102888=CARTESIAN_POINT('Ctrl Pts',(-2.56675261809335,1.43775693269445,
10.2408998187229));
#102889=CARTESIAN_POINT('Ctrl Pts',(-2.52113578048464,1.51919429856537,
10.2358657110879));
#102890=CARTESIAN_POINT('Ctrl Pts',(-2.4716356318738,1.59846531209709,10.2308316034528));
#102891=CARTESIAN_POINT('Ctrl Pts',(-2.4184945096012,1.67518605146678,10.2257974958177));
#102892=CARTESIAN_POINT('Ctrl Pts',(-2.36534297012712,1.75192183032689,
10.2207624013516));
#102893=CARTESIAN_POINT('Ctrl Pts',(-2.30854929274796,1.82610597720804,
10.2157273068854));
#102894=CARTESIAN_POINT('Ctrl Pts',(-2.24839807756254,1.89738506498103,
10.2106922124192));
#102895=CARTESIAN_POINT('Ctrl Pts',(-2.1881807806527,1.96874245948516,10.2056515864317));
#102896=CARTESIAN_POINT('Ctrl Pts',(-2.12459887007337,2.03718808428977,
10.2006109604442));
#102897=CARTESIAN_POINT('Ctrl Pts',(-2.05797582847605,2.10240326517258,
10.1955703344568));
#102898=CARTESIAN_POINT('Ctrl Pts',(-1.99131184696814,2.16765852083448,
10.1905266110008));
#102899=CARTESIAN_POINT('Ctrl Pts',(-1.92160334571709,2.22967908553681,
10.1854828875448));
#102900=CARTESIAN_POINT('Ctrl Pts',(-1.84920744278971,2.28818614486041,
10.1804391640887));
#102901=CARTESIAN_POINT('Ctrl Pts',(-1.77669437699459,2.34678788985787,
10.1753872780561));
#102902=CARTESIAN_POINT('Ctrl Pts',(-1.70148558487444,2.40186451570675,
10.1703353920235));
#102903=CARTESIAN_POINT('Ctrl Pts',(-1.62396756871984,2.45318024933884,
10.1652835059909));
#102904=CARTESIAN_POINT('Ctrl Pts',(-1.58484067415706,2.47908165134621,
10.1627335876371));
#102905=CARTESIAN_POINT('Ctrl Pts',(-1.54512586404205,2.50402562139544,
10.1601836692833));
#102906=CARTESIAN_POINT('Ctrl Pts',(-1.50487502376479,2.52798638502048,
10.1576337509296));
#102907=CARTESIAN_POINT('Ctrl Pts',(-1.42512284768101,2.57546174271645,
10.1525813958446));
#102908=CARTESIAN_POINT('Ctrl Pts',(-1.34297876235402,2.61924458675749,
10.1475290407596));
#102909=CARTESIAN_POINT('Ctrl Pts',(-1.25881923275757,2.65908595935514,
10.1424766856747));
#102910=CARTESIAN_POINT('Ctrl Pts',(-1.17477574632801,2.69887239677109,
10.1374312970175));
#102911=CARTESIAN_POINT('Ctrl Pts',(-1.08872273587955,2.7347279737394,10.1323859083604));
#102912=CARTESIAN_POINT('Ctrl Pts',(-1.00106365636304,2.76644818420824,
10.1273405197032));
#102913=CARTESIAN_POINT('Ctrl Pts',(-0.913498362587476,2.79813445748017,
10.1223005290666));
#102914=CARTESIAN_POINT('Ctrl Pts',(-0.824330830657412,2.82569400806737,
10.1172605384301));
#102915=CARTESIAN_POINT('Ctrl Pts',(-0.733986011924087,2.84896973207856,
10.1122205477935));
#102916=CARTESIAN_POINT('Ctrl Pts',(-0.643706288476191,2.87222868545564,
10.107184188573));
#102917=CARTESIAN_POINT('Ctrl Pts',(-0.552251393216398,2.89120983676699,
10.1021478293526));
#102918=CARTESIAN_POINT('Ctrl Pts',(-0.460062015195089,2.90580573028801,
10.0971114701321));
#102919=CARTESIAN_POINT('Ctrl Pts',(-0.367906139577596,2.92039631953723,
10.0920769411674));
#102920=CARTESIAN_POINT('Ctrl Pts',(-0.275016749791795,2.93060474753725,
10.0870424122027));
#102921=CARTESIAN_POINT('Ctrl Pts',(-0.181844296427517,2.93637474649555,
10.082007883238));
#102922=CARTESIAN_POINT('Ctrl Pts',(-0.0886796404811632,2.94214426257407,
10.0769737756031));
#102923=CARTESIAN_POINT('Ctrl Pts',(0.00476758854223665,2.9434760608548,
10.0719396679682));
#102924=CARTESIAN_POINT('Ctrl Pts',(0.0980434025714094,2.94036587709969,
10.0669055603332));
#102925=CARTESIAN_POINT('Ctrl Pts',(0.191337501365793,2.93725508365834,
10.0618704658672));
#102926=CARTESIAN_POINT('Ctrl Pts',(0.284459674477728,2.92970059402629,
10.0568353714011));
#102927=CARTESIAN_POINT('Ctrl Pts',(0.376958673570008,2.9177501878023,10.0518002769351));
#102928=CARTESIAN_POINT('Ctrl Pts',(0.469559291446737,2.9057866529416,10.0467596509478));
#102929=CARTESIAN_POINT('Ctrl Pts',(0.561534927474578,2.88941761860679,
10.0417190249605));
#102930=CARTESIAN_POINT('Ctrl Pts',(0.652442483437231,2.86874237355087,
10.0366783989732));
#102931=CARTESIAN_POINT('Ctrl Pts',(0.743405902163319,2.84805442354087,
10.0316346755173));
#102932=CARTESIAN_POINT('Ctrl Pts',(0.833299506507768,2.82305511373853,
10.0265909520614));
#102933=CARTESIAN_POINT('Ctrl Pts',(0.921695483447506,2.79389359779367,
10.0215472286055));
#102934=CARTESIAN_POINT('Ctrl Pts',(1.01023451718657,2.7646848879235,10.016495342573));
#102935=CARTESIAN_POINT('Ctrl Pts',(1.09727067065002,2.73130068331518,10.0114434565406));
#102936=CARTESIAN_POINT('Ctrl Pts',(1.18239639318077,2.69393815248107,10.006391570508));
#102937=CARTESIAN_POINT('Ctrl Pts',(1.2253632457321,2.67507957124889,10.0038416521542));
#102938=CARTESIAN_POINT('Ctrl Pts',(1.26784377224799,2.65520816839446,10.0012917338004));
#102939=CARTESIAN_POINT('Ctrl Pts',(1.30978820139893,2.63435359575668,9.99874181544654));
#102940=CARTESIAN_POINT('Ctrl Pts',(1.39289601917855,2.59303278015049,9.99368946036164));
#102941=CARTESIAN_POINT('Ctrl Pts',(1.47419567339604,2.54770117516414,9.98863710527674));
#102942=CARTESIAN_POINT('Ctrl Pts',(1.55327396775754,2.49854037011347,9.98358475019183));
#102943=CARTESIAN_POINT('Ctrl Pts',(1.63224322520128,2.44944735032171,9.97853936153469));
#102944=CARTESIAN_POINT('Ctrl Pts',(1.70899683519463,2.3965358547847,9.97349397287754));
#102945=CARTESIAN_POINT('Ctrl Pts',(1.78314434629204,2.34003423912701,9.96844858422039));
#102946=CARTESIAN_POINT('Ctrl Pts',(1.85721252756636,2.28359307409144,9.9634085935838));
#102947=CARTESIAN_POINT('Ctrl Pts',(1.9286798005607,2.22356969139925,9.95836860294721));
#102948=CARTESIAN_POINT('Ctrl Pts',(1.99718391456342,2.16023619343097,9.95332861231061));
#102949=CARTESIAN_POINT('Ctrl Pts',(2.06563866995415,2.09694832854032,9.94829225309011));
#102950=CARTESIAN_POINT('Ctrl Pts',(2.13113418474373,2.03035538961638,9.94325589386961));
#102951=CARTESIAN_POINT('Ctrl Pts',(2.1933414163386,1.96076960180787,9.9382195346491));
#102952=CARTESIAN_POINT('Ctrl Pts',(2.25552604129659,1.89120910206629,9.93318500568435));
#102953=CARTESIAN_POINT('Ctrl Pts',(2.31442446126173,1.81865824498921,9.9281504767196));
#102954=CARTESIAN_POINT('Ctrl Pts',(2.36974537328843,1.74346518915006,9.92311594775485));
#102955=CARTESIAN_POINT('Ctrl Pts',(2.42506165561767,1.6682784260687,9.91808184011985));
#102956=CARTESIAN_POINT('Ctrl Pts',(2.47680076216299,1.5904502618047,9.91304773248484));
#102957=CARTESIAN_POINT('Ctrl Pts',(2.52471318674338,1.51035999837261,9.90801362484984));
#102958=CARTESIAN_POINT('Ctrl Pts',(2.57263500354874,1.43025403492578,9.90297853038372));
#102959=CARTESIAN_POINT('Ctrl Pts',(2.61672842087429,1.34788547303943,9.8979434359176));
#102960=CARTESIAN_POINT('Ctrl Pts',(2.65678916348219,1.26365950350701,9.89290834145147));
#102961=CARTESIAN_POINT('Ctrl Pts',(2.6968939165552,1.17934100388526,9.88786771546409));
#102962=CARTESIAN_POINT('Ctrl Pts',(2.73295696047361,1.09316142526529,9.88282708947671));
#102963=CARTESIAN_POINT('Ctrl Pts',(2.76482173226482,1.00554700973956,9.87778646348933));
#102964=CARTESIAN_POINT('Ctrl Pts',(2.79670608498293,0.917878755087725,
9.87274274003339));
#102965=CARTESIAN_POINT('Ctrl Pts',(2.82438689791758,0.828774332145286,
9.86769901657745));
#102966=CARTESIAN_POINT('Ctrl Pts',(2.84775780324887,0.738674146044887,
9.8626552931215));
#102967=CARTESIAN_POINT('Ctrl Pts',(2.87116653119416,0.648428145115718,
9.85760340708895));
#102968=CARTESIAN_POINT('Ctrl Pts',(2.89025133600985,0.557183598143385,
9.85255152105639));
#102969=CARTESIAN_POINT('Ctrl Pts',(2.90495718602783,0.465389887454911,
9.84749963502384));
#102970=CARTESIAN_POINT('Ctrl Pts',(2.91237990234179,0.419057395758485,
9.84494971666997));
#102971=CARTESIAN_POINT('Ctrl Pts',(2.91868782514139,0.372585061037236,
9.8423997983161));
#102972=CARTESIAN_POINT('Ctrl Pts',(2.92387891834262,0.326030782092145,
9.83984987996223));
#102973=CARTESIAN_POINT('Ctrl Pts',(2.93416444222685,0.233789104001969,
9.83479752487729));
#102974=CARTESIAN_POINT('Ctrl Pts',(2.9400991209621,0.140894713563981,9.82974516979236));
#102975=CARTESIAN_POINT('Ctrl Pts',(2.94161176916946,0.0477932995695164,
9.82469281470743));
#102976=CARTESIAN_POINT('Ctrl Pts',(2.94312233166544,-0.0451797417620558,
9.81964742605027));
#102977=CARTESIAN_POINT('Ctrl Pts',(2.94022297261431,-0.138358799087583,
9.81460203739312));
#102978=CARTESIAN_POINT('Ctrl Pts',(2.93289413802449,-0.231291969470567,
9.80955664873596));
#102979=CARTESIAN_POINT('Ctrl Pts',(2.9255731444956,-0.324125711405322,
9.80451665809938));
#102980=CARTESIAN_POINT('Ctrl Pts',(2.91383212977308,-0.416713648807271,
9.79947666746279));
#102981=CARTESIAN_POINT('Ctrl Pts',(2.89770358849643,-0.508603886354484,
9.79443667682621));
#102982=CARTESIAN_POINT('Ctrl Pts',(2.88158666816288,-0.60042791511054,
9.78940031760572));
#102983=CARTESIAN_POINT('Ctrl Pts',(2.86108858138902,-0.691554806919165,
9.78436395838523));
#102984=CARTESIAN_POINT('Ctrl Pts',(2.83629353766523,-0.781538846250444,
9.77932759916474));
#102985=CARTESIAN_POINT('Ctrl Pts',(2.81150750467114,-0.871490184616759,
9.77429307020002));
#102986=CARTESIAN_POINT('Ctrl Pts',(2.78242773481146,-0.960299067741857,
9.7692585412353));
#102987=CARTESIAN_POINT('Ctrl Pts',(2.74918908565584,-1.04753203832188,
9.76422401227058));
#102988=CARTESIAN_POINT('Ctrl Pts',(2.71595321817689,-1.13475770854751,
9.75918990463561));
#102989=CARTESIAN_POINT('Ctrl Pts',(2.67855932175438,-1.22040731338701,
9.75415579700064));
#102990=CARTESIAN_POINT('Ctrl Pts',(2.63719107339544,-1.30406565877774,
9.74912168936567));
#102991=CARTESIAN_POINT('Ctrl Pts',(2.59581471565988,-1.38774040363078,
9.74408659489958));
#102992=CARTESIAN_POINT('Ctrl Pts',(2.55046265594753,-1.46942271578298,
9.7390515004335));
#102993=CARTESIAN_POINT('Ctrl Pts',(2.50136483402241,-1.54872139751347,
9.73401640596741));
#102994=CARTESIAN_POINT('Ctrl Pts',(2.45221307355703,-1.62810719624769,
9.72897577998007));
#102995=CARTESIAN_POINT('Ctrl Pts',(2.3993075709415,-1.70510375916307,9.72393515399273));
#102996=CARTESIAN_POINT('Ctrl Pts',(2.34292180653509,-1.7793485910474,9.71889452800539));
#102997=CARTESIAN_POINT('Ctrl Pts',(2.28650139303285,-1.85363904643832,
9.71385080454948));
#102998=CARTESIAN_POINT('Ctrl Pts',(2.22659674516041,-1.92517406412833,
9.70880708109357));
#102999=CARTESIAN_POINT('Ctrl Pts',(2.16352043872119,-1.9936256697875,9.70376335763766));
#103000=CARTESIAN_POINT('Ctrl Pts',(2.10034205190652,-2.06218805500877,
9.69871147160514));
#103001=CARTESIAN_POINT('Ctrl Pts',(2.03398207519571,-2.12765675453755,
9.69365958557261));
#103002=CARTESIAN_POINT('Ctrl Pts',(1.96478843880395,-2.18974208315554,
9.68860769954008));
#103003=CARTESIAN_POINT('Ctrl Pts',(1.92986324012209,-2.22107939320721,
9.68605778118624));
#103004=CARTESIAN_POINT('Ctrl Pts',(1.89421661775184,-2.25155538536574,
9.6835078628324));
#103005=CARTESIAN_POINT('Ctrl Pts',(1.85789613716139,-2.28113698482156,
9.68095794447856));
#103006=CARTESIAN_POINT('Ctrl Pts',(1.78593149385365,-2.33974934949027,
9.67590558939365));
#103007=CARTESIAN_POINT('Ctrl Pts',(1.71106137704479,-2.3950580630494,9.67085323430873));
#103008=CARTESIAN_POINT('Ctrl Pts',(1.6336218619111,-2.44676186260251,9.6658008792238));
#103009=CARTESIAN_POINT('Ctrl Pts',(1.55628912406838,-2.49839437049478,
9.66075549056665));
#103010=CARTESIAN_POINT('Ctrl Pts',(1.47639439417413,-2.54643159712274,
9.6557101019095));
#103011=CARTESIAN_POINT('Ctrl Pts',(1.39430693918763,-2.59061231359176,
9.65066471325235));
#103012=CARTESIAN_POINT('Ctrl Pts',(1.31230730890611,-2.63474576146911,
9.64562472261577));
#103013=CARTESIAN_POINT('Ctrl Pts',(1.22812000560482,-2.67503069093299,
9.64058473197918));
#103014=CARTESIAN_POINT('Ctrl Pts',(1.14214248417568,-2.71124962809421,
9.6355447413426));
#103015=CARTESIAN_POINT('Ctrl Pts',(1.05622691130505,-2.74744246877219,
9.6305083821221));
#103016=CARTESIAN_POINT('Ctrl Pts',(0.968524092363189,-2.7795749682352,
9.6254720229016));
#103017=CARTESIAN_POINT('Ctrl Pts',(0.879454301178353,-2.80747647045151,
9.6204356636811));
#103018=CARTESIAN_POINT('Ctrl Pts',(0.790416878712944,-2.8353678330247,
9.61540113471637));
#103019=CARTESIAN_POINT('Ctrl Pts',(0.700013894391332,-2.85903112025962,
9.61036660575163));
#103020=CARTESIAN_POINT('Ctrl Pts',(0.608682753724642,-2.8783448899182,
9.6053320767869));
#103021=CARTESIAN_POINT('Ctrl Pts',(0.517359256380052,-2.89765704324568,
9.60029796915191));
#103022=CARTESIAN_POINT('Ctrl Pts',(0.425108191794256,-2.91262031099064,
9.59526386151691));
#103023=CARTESIAN_POINT('Ctrl Pts',(0.332378058922914,-2.92316418046381,
9.59022975388192));
#103024=CARTESIAN_POINT('Ctrl Pts',(0.239629748255843,-2.93371011684122,
9.58519465941582));
#103025=CARTESIAN_POINT('Ctrl Pts',(0.14640262420569,-2.93983488459261,
9.58015956494972));
#103026=CARTESIAN_POINT('Ctrl Pts',(0.0531500751266599,-2.94151985706608,
9.57512447048362));
#103027=CARTESIAN_POINT('Ctrl Pts',(-0.040204920581921,-2.94320668063908,
9.57008384449625));
#103028=CARTESIAN_POINT('Ctrl Pts',(-0.13358495222081,-2.94044396478311,
9.5650432185089));
#103029=CARTESIAN_POINT('Ctrl Pts',(-0.226537172506329,-2.93326522999078,
9.56000259252154));
#103030=CARTESIAN_POINT('Ctrl Pts',(-0.319546512003089,-2.92608208386036,
9.55495886906561));
#103031=CARTESIAN_POINT('Ctrl Pts',(-0.412127076320044,-2.91447757166104,
9.54991514560968));
#103032=CARTESIAN_POINT('Ctrl Pts',(-0.503833857938221,-2.89853677630543,
9.54487142215376));
#103033=CARTESIAN_POINT('Ctrl Pts',(-0.595689054440318,-2.88257018295266,
9.53981953612121));
#103034=CARTESIAN_POINT('Ctrl Pts',(-0.686667212163074,-2.86225339323529,
9.53476765008867));
#103035=CARTESIAN_POINT('Ctrl Pts',(-0.776336357326798,-2.83772194908038,
9.52971576405613));
#103036=CARTESIAN_POINT('Ctrl Pts',(-0.821596483456769,-2.82533980520498,
9.52716584570228));
#103037=CARTESIAN_POINT('Ctrl Pts',(-0.866523395126456,-2.81188468007406,
9.52461592734843));
#103038=CARTESIAN_POINT('Ctrl Pts',(-0.911063524573254,-2.79737863976119,
9.52206600899458));
#103039=CARTESIAN_POINT('Ctrl Pts',(-0.999314408823774,-2.76863667379735,
9.51701365390965));
#103040=CARTESIAN_POINT('Ctrl Pts',(-1.08636219212492,-2.73566287194053,
9.51196129882473));
#103041=CARTESIAN_POINT('Ctrl Pts',(-1.17177159054851,-2.69857653950808,
9.5069089437398));
#103042=CARTESIAN_POINT('Ctrl Pts',(-1.25706322242659,-2.66154134347674,
9.50186355508265));
#103043=CARTESIAN_POINT('Ctrl Pts',(-1.34072055456809,-2.62040506039286,
9.49681816642549));
#103044=CARTESIAN_POINT('Ctrl Pts',(-1.42232397497759,-2.57533658192555,
9.49177277776833));
#103045=CARTESIAN_POINT('Ctrl Pts',(-1.50384008854676,-2.53031632185929,
9.48673278713175));
#103046=CARTESIAN_POINT('Ctrl Pts',(-1.58330627139328,-2.48137244213095,
9.48169279649516));
#103047=CARTESIAN_POINT('Ctrl Pts',(-1.66032442179078,-2.42872123027842,
9.47665280585858));
#103048=CARTESIAN_POINT('Ctrl Pts',(-1.73728707903936,-2.37610795469838,
9.47161644663809));
#103049=CARTESIAN_POINT('Ctrl Pts',(-1.81180484407345,-2.31979290638618,
9.4665800874176));
#103050=CARTESIAN_POINT('Ctrl Pts',(-1.88350660834158,-2.26003691481657,
9.46154372819711));
#103051=CARTESIAN_POINT('Ctrl Pts',(-1.95518231557898,-2.20030263908234,
9.45650919923238));
#103052=CARTESIAN_POINT('Ctrl Pts',(-2.02404371414397,-2.13713018840411,
9.45147467026765));
#103053=CARTESIAN_POINT('Ctrl Pts',(-2.08975178336914,-2.07082145147898,
9.44644014130293));
#103054=CARTESIAN_POINT('Ctrl Pts',(-2.15545435361622,-2.00451826380062,
9.44140603366795));
#103055=CARTESIAN_POINT('Ctrl Pts',(-2.21800380665003,-1.93507962740859,
9.43637192603297));
#103056=CARTESIAN_POINT('Ctrl Pts',(-2.27709792277764,-1.86284434402924,
9.43133781839799));
#103057=CARTESIAN_POINT('Ctrl Pts',(-2.3362036230661,-1.7905949004391,9.4263027239319));
#103058=CARTESIAN_POINT('Ctrl Pts',(-2.39185236025071,-1.71554806513985,
9.4212676294658));
#103059=CARTESIAN_POINT('Ctrl Pts',(-2.44378288029811,-1.63807485603127,
9.41623253499971));
#103060=CARTESIAN_POINT('Ctrl Pts',(-2.49577045086908,-1.56051653537099,
9.41119190901236));
#103061=CARTESIAN_POINT('Ctrl Pts',(-2.54403140282222,-1.48052688963884,
9.40615128302501));
#103062=CARTESIAN_POINT('Ctrl Pts',(-2.58834860890672,-1.39850472962041,
9.40111065703766));
#103063=CARTESIAN_POINT('Ctrl Pts',(-2.63269304794863,-1.31643216692123,
9.39606693358174));
#103064=CARTESIAN_POINT('Ctrl Pts',(-2.67308872434821,-1.23232500360651,
9.39102321012582));
#103065=CARTESIAN_POINT('Ctrl Pts',(-2.70936609977634,-1.14660339149277,
9.38597948666991));
#103066=CARTESIAN_POINT('Ctrl Pts',(-2.7457021851752,-1.06074305067338,
9.38092760063737));
#103067=CARTESIAN_POINT('Ctrl Pts',(-2.77790651068688,-0.973263461366016,
9.37587571460483));
#103068=CARTESIAN_POINT('Ctrl Pts',(-2.80585901294174,-0.884601152776558,
9.3708238285723));
#103069=CARTESIAN_POINT('Ctrl Pts',(-2.81996792159021,-0.839849223198082,
9.36827391021845));
#103070=CARTESIAN_POINT('Ctrl Pts',(-2.83299440725562,-0.794796160531161,
9.36572399186461));
#103071=CARTESIAN_POINT('Ctrl Pts',(-2.8449280009364,-0.749498945621697,
9.36317407351076));
#103072=CARTESIAN_POINT('Ctrl Pts',(-2.8769063231013,-0.628116487805915,
9.35634108482397));
#103073=CARTESIAN_POINT('Ctrl Pts',(-2.90113079108199,-0.504612143223255,
9.34950809613718));
#103074=CARTESIAN_POINT('Ctrl Pts',(-2.91737508842437,-0.379850751533926,
9.34267510745039));
#103075=CARTESIAN_POINT('Ctrl Pts',(-2.93256699151605,-0.263172083803379,
9.33628479706833));
#103076=CARTESIAN_POINT('Ctrl Pts',(-2.94077959844473,-0.14539389336001,
9.32989448668627));
#103077=CARTESIAN_POINT('Ctrl Pts',(-2.9418738304784,-0.0272463859323058,
9.32350417630422));
#103078=CARTESIAN_POINT('Ctrl Pts',(-2.94194963161366,-0.0190619105047869,
9.32306149799949));
#103079=CARTESIAN_POINT('Ctrl Pts',(-2.94199129147202,-0.010875672699581,
9.32261881969475));
#103080=CARTESIAN_POINT('Ctrl Pts',(-2.94199877210839,-0.00268791977826042,
9.32217614139002));
#103081=CARTESIAN_POINT('',(-2.93737145535825,0.000822519638358221,8.3221761170896));
#103082=CARTESIAN_POINT('Ctrl Pts',(-2.94126103584025,-0.00268679640793773,
9.3221761170896));
#103083=CARTESIAN_POINT('Ctrl Pts',(-2.934746619203,0.723990958988464,9.28287812406869));
#103084=CARTESIAN_POINT('Ctrl Pts',(-2.2959122451109,2.44028323228705,9.19061615255315));
#103085=CARTESIAN_POINT('Ctrl Pts',(0.582625545836898,3.42906223071866,
9.04539020254303));
#103086=CARTESIAN_POINT('Ctrl Pts',(3.19799441672963,1.36775437099239,8.88649826705913));
#103087=CARTESIAN_POINT('Ctrl Pts',(2.88203120349949,-1.94725870157488,
8.72760633157527));
#103088=CARTESIAN_POINT('Ctrl Pts',(-0.0756472328928887,-3.47738375865513,
8.56871439609139));
#103089=CARTESIAN_POINT('Ctrl Pts',(-2.53228522578548,-2.06778972386557,
8.43357099126284));
#103090=CARTESIAN_POINT('Ctrl Pts',(-2.93601614403195,-0.541218415403109,
8.35139156492891));
#103091=CARTESIAN_POINT('Ctrl Pts',(-2.93737145535825,0.000822519638358221,
8.3221761170896));
#103092=CARTESIAN_POINT('',(-2.94199909588776,0.00230646821441294,7.3221761170896));
#103093=CARTESIAN_POINT('Ctrl Pts',(-2.93737145535825,0.000822519638358221,
8.3221761170896));
#103094=CARTESIAN_POINT('Ctrl Pts',(-2.93847315514246,0.441434480580057,
8.29842758643428));
#103095=CARTESIAN_POINT('Ctrl Pts',(-2.63857366541807,1.86327470776546,
8.22171507728432));
#103096=CARTESIAN_POINT('Ctrl Pts',(-0.432952847726418,3.45115518927333,
8.09203858963981));
#103097=CARTESIAN_POINT('Ctrl Pts',(2.66643443613374,2.2333937643423,7.9331466541559));
#103098=CARTESIAN_POINT('Ctrl Pts',(3.32172589169603,-1.03153158421828,
7.77425471867204));
#103099=CARTESIAN_POINT('Ctrl Pts',(0.932271043120299,-3.35093882530888,
7.61536278318816));
#103100=CARTESIAN_POINT('Ctrl Pts',(-2.1443156395293,-2.63763485171723,
7.46467029144031));
#103101=CARTESIAN_POINT('Ctrl Pts',(-2.93716327839541,-0.823293308472798,
7.36694177818707));
#103102=CARTESIAN_POINT('Ctrl Pts',(-2.94428241720801,0.00228748565644199,
7.32217724342845));
#103103=CARTESIAN_POINT('',(-2.9419992148765,-0.00214934084322361,6.3221761170896));
#103104=CARTESIAN_POINT('Ctrl Pts',(-2.94199909588776,0.00230646821441294,
7.3221761170896));
#103105=CARTESIAN_POINT('Ctrl Pts',(-2.94188064052067,0.1534013676358,7.31397704879987));
#103106=CARTESIAN_POINT('Ctrl Pts',(-2.93012005936685,0.304050427900592,
7.30577798051015));
#103107=CARTESIAN_POINT('Ctrl Pts',(-2.90693455819628,0.452874678431272,
7.29757891222043));
#103108=CARTESIAN_POINT('Ctrl Pts',(-2.89264740011975,0.544581800796651,
7.29252655713551));
#103109=CARTESIAN_POINT('Ctrl Pts',(-2.87399062726682,0.635776718490721,
7.2874742020506));
#103110=CARTESIAN_POINT('Ctrl Pts',(-2.85101253679382,0.72601068521369,
7.28242184696568));
#103111=CARTESIAN_POINT('Ctrl Pts',(-2.82806612960614,0.816120233046577,
7.27737645830853));
#103112=CARTESIAN_POINT('Ctrl Pts',(-2.80081035366142,0.9052710360974,7.27233106965139));
#103113=CARTESIAN_POINT('Ctrl Pts',(-2.76934495822611,0.993021904263771,
7.26728568099424));
#103114=CARTESIAN_POINT('Ctrl Pts',(-2.73791322736321,1.08067888848511,
7.26224569035767));
#103115=CARTESIAN_POINT('Ctrl Pts',(-2.70228097821773,1.16693849896334,
7.2572056997211));
#103116=CARTESIAN_POINT('Ctrl Pts',(-2.66259818166292,1.25137321491445,
7.25216570908452));
#103117=CARTESIAN_POINT('Ctrl Pts',(-2.62294397737271,1.33574709392993,
7.24712934986403));
#103118=CARTESIAN_POINT('Ctrl Pts',(-2.57924521502232,1.41829829102065,
7.24209299064354));
#103119=CARTESIAN_POINT('Ctrl Pts',(-2.5317001449129,1.49861882286591,7.23705663142306));
#103120=CARTESIAN_POINT('Ctrl Pts',(-2.48417235308614,1.57891016554709,
7.23202210245833));
#103121=CARTESIAN_POINT('Ctrl Pts',(-2.43280125640771,1.65697207151327,
7.2269875734936));
#103122=CARTESIAN_POINT('Ctrl Pts',(-2.37783075974406,1.73242168019653,
7.22195304452886));
#103123=CARTESIAN_POINT('Ctrl Pts',(-2.32286486345237,1.80786497465153,
7.21691893689389));
#103124=CARTESIAN_POINT('Ctrl Pts',(-2.26430042782968,1.88069604754626,
7.21188482925891));
#103125=CARTESIAN_POINT('Ctrl Pts',(-2.20242367156039,1.95056247553121,
7.20685072162393));
#103126=CARTESIAN_POINT('Ctrl Pts',(-2.14053478565207,2.0204425993626,7.20181562715784));
#103127=CARTESIAN_POINT('Ctrl Pts',(-2.07533258435519,2.08735659180591,
7.19678053269174));
#103128=CARTESIAN_POINT('Ctrl Pts',(-2.00714162828726,2.15098732771636,
7.19174543822565));
#103129=CARTESIAN_POINT('Ctrl Pts',(-1.93887575808903,2.21468796792961,
7.1867048122383));
#103130=CARTESIAN_POINT('Ctrl Pts',(-1.86761490432089,2.27509784814801,
7.18166418625095));
#103131=CARTESIAN_POINT('Ctrl Pts',(-1.79371810752436,2.33193896805625,
7.1766235602636));
#103132=CARTESIAN_POINT('Ctrl Pts',(-1.71977590108904,2.38881501687664,
7.17157983680768));
#103133=CARTESIAN_POINT('Ctrl Pts',(-1.64319489128419,2.44211768594572,
7.16653611335176));
#103134=CARTESIAN_POINT('Ctrl Pts',(-1.56436278205414,2.49161254735238,
7.16149238989584));
#103135=CARTESIAN_POINT('Ctrl Pts',(-1.48540309383668,2.54118750942313,
7.15644050386331));
#103136=CARTESIAN_POINT('Ctrl Pts',(-1.40418541977465,2.58694214358168,
7.15138861783078));
#103137=CARTESIAN_POINT('Ctrl Pts',(-1.32112152825515,2.62868824845792,
7.14633673179825));
#103138=CARTESIAN_POINT('Ctrl Pts',(-1.2791953762858,2.64975942036129,7.14378681344435));
#103139=CARTESIAN_POINT('Ctrl Pts',(-1.23679917931604,2.66981011279453,
7.14123689509045));
#103140=CARTESIAN_POINT('Ctrl Pts',(-1.1939875166179,2.68882089588738,7.13868697673655));
#103141=CARTESIAN_POINT('Ctrl Pts',(-1.10916138036285,2.72648846531395,
7.13363462165162));
#103142=CARTESIAN_POINT('Ctrl Pts',(-1.02239880566903,2.76020557994489,
7.1285822665667));
#103143=CARTESIAN_POINT('Ctrl Pts',(-0.934103160531709,2.78976975492328,
7.12352991148177));
#103144=CARTESIAN_POINT('Ctrl Pts',(-0.845929261634393,2.8192931654094,
7.11848452282463));
#103145=CARTESIAN_POINT('Ctrl Pts',(-0.756226910426811,2.84467487525731,
7.11343913416748));
#103146=CARTESIAN_POINT('Ctrl Pts',(-0.665420994541296,2.86575974220165,
7.10839374551033));
#103147=CARTESIAN_POINT('Ctrl Pts',(-0.574712231171534,2.8868220506172,
7.10335375487374));
#103148=CARTESIAN_POINT('Ctrl Pts',(-0.482902680340056,2.90359655374513,
7.09831376423715));
#103149=CARTESIAN_POINT('Ctrl Pts',(-0.390432944213572,2.91597772900835,
7.09327377360056));
#103150=CARTESIAN_POINT('Ctrl Pts',(-0.298029834418809,2.92834998338217,
7.08823741438007));
#103151=CARTESIAN_POINT('Ctrl Pts',(-0.204967923849687,2.93633514294952,
7.08320105515958));
#103152=CARTESIAN_POINT('Ctrl Pts',(-0.111697544516788,2.93987885099861,
7.07816469593908));
#103153=CARTESIAN_POINT('Ctrl Pts',(-0.0184610604327648,2.94342127123407,
7.07313016697435));
#103154=CARTESIAN_POINT('Ctrl Pts',(0.0749832984381998,2.94252542961131,
7.06809563800962));
#103155=CARTESIAN_POINT('Ctrl Pts',(0.168181586974739,2.93718895439205,
7.06306110904489));
#103156=CARTESIAN_POINT('Ctrl Pts',(0.261372075931218,2.93185292577182,
7.05802700140991));
#103157=CARTESIAN_POINT('Ctrl Pts',(0.354316091994384,2.92207702801956,
7.05299289377493));
#103158=CARTESIAN_POINT('Ctrl Pts',(0.446562353806051,2.90791094501933,
7.04795878613995));
#103159=CARTESIAN_POINT('Ctrl Pts',(0.538826698560719,2.89374208505593,
7.04292369167385));
#103160=CARTESIAN_POINT('Ctrl Pts',(0.630392578408343,2.87518139847378,
7.03788859720775));
#103161=CARTESIAN_POINT('Ctrl Pts',(0.720817613325796,2.85232991926237,
7.03285350274166));
#103162=CARTESIAN_POINT('Ctrl Pts',(0.811341988584582,2.82945333556804,
7.02781287675431));
#103163=CARTESIAN_POINT('Ctrl Pts',(0.900722585767078,2.80227665889332,
7.02277225076695));
#103164=CARTESIAN_POINT('Ctrl Pts',(0.988531234777763,2.77095109986964,
7.0177316247796));
#103165=CARTESIAN_POINT('Ctrl Pts',(1.07639384227117,2.73960629126571,7.01268790132368));
#103166=CARTESIAN_POINT('Ctrl Pts',(1.16268216802116,2.70410769366106,7.00764417786776));
#103167=CARTESIAN_POINT('Ctrl Pts',(1.24698914115239,2.6646542143115,7.00260045441184));
#103168=CARTESIAN_POINT('Ctrl Pts',(1.33143255358951,2.6251368849014,6.9975485683793));
#103169=CARTESIAN_POINT('Ctrl Pts',(1.41388781949333,2.58165210306019,6.99249668234676));
#103170=CARTESIAN_POINT('Ctrl Pts',(1.49397368943538,2.5344440446131,6.98744479631423));
#103171=CARTESIAN_POINT('Ctrl Pts',(1.53439669746323,2.5106159744808,6.98489487796038));
#103172=CARTESIAN_POINT('Ctrl Pts',(1.57421653361987,2.48584000965761,6.98234495960653));
#103173=CARTESIAN_POINT('Ctrl Pts',(1.61338730044221,2.46015150321516,6.97979504125269));
#103174=CARTESIAN_POINT('Ctrl Pts',(1.69099944148848,2.40925283190953,6.97474268616776));
#103175=CARTESIAN_POINT('Ctrl Pts',(1.76633987464382,2.35458650481048,6.96969033108284));
#103176=CARTESIAN_POINT('Ctrl Pts',(1.83901989453574,2.29638189931504,6.96463797599791));
#103177=CARTESIAN_POINT('Ctrl Pts',(1.91159969975537,2.23825754910124,6.95959258734076));
#103178=CARTESIAN_POINT('Ctrl Pts',(1.98152603736183,2.176604890473,6.95454719868361));
#103179=CARTESIAN_POINT('Ctrl Pts',(2.04843834005712,2.11169703484757,6.94950181002646));
#103180=CARTESIAN_POINT('Ctrl Pts',(2.11527905382032,2.0468586236125,6.94446181938987));
#103181=CARTESIAN_POINT('Ctrl Pts',(2.17911182508806,1.97877224544958,6.93942182875328));
#103182=CARTESIAN_POINT('Ctrl Pts',(2.23960928329026,1.90775109964588,6.93438183811669));
#103183=CARTESIAN_POINT('Ctrl Pts',(2.30006315183939,1.83678112602691,6.9293454788962));
#103184=CARTESIAN_POINT('Ctrl Pts',(2.35718619670429,1.76288092496186,6.9243091196757));
#103185=CARTESIAN_POINT('Ctrl Pts',(2.41068878558327,1.68639959056655,6.91927276045521));
#103186=CARTESIAN_POINT('Ctrl Pts',(2.46417193116656,1.60994605013843,6.91423823149048));
#103187=CARTESIAN_POINT('Ctrl Pts',(2.51403698016615,1.53091360347701,6.90920370252574));
#103188=CARTESIAN_POINT('Ctrl Pts',(2.56003604045838,1.44968254164633,6.90416917356101));
#103189=CARTESIAN_POINT('Ctrl Pts',(2.60603125118043,1.3684582778822,6.89913506592603));
#103190=CARTESIAN_POINT('Ctrl Pts',(2.64816089772338,1.28503615143493,6.89410095829104));
#103191=CARTESIAN_POINT('Ctrl Pts',(2.68622228766056,1.19982241239096,6.88906685065606));
#103192=CARTESIAN_POINT('Ctrl Pts',(2.72429113873418,1.11459196898242,6.88403175618996));
#103193=CARTESIAN_POINT('Ctrl Pts',(2.75828996854704,1.02756962122026,6.87899666172386));
#103194=CARTESIAN_POINT('Ctrl Pts',(2.7880640701717,0.939181952881126,6.87396156725776));
#103195=CARTESIAN_POINT('Ctrl Pts',(2.81787088142616,0.850697182438061,
6.8689209412704));
#103196=CARTESIAN_POINT('Ctrl Pts',(2.84344355796929,0.76084451902619,6.86388031528305));
#103197=CARTESIAN_POINT('Ctrl Pts',(2.86467726760925,0.67006578217577,6.8588396892957));
#103198=CARTESIAN_POINT('Ctrl Pts',(2.8859240253802,0.579231261721361,6.85379596583977));
#103199=CARTESIAN_POINT('Ctrl Pts',(2.90282642775214,0.487469971480362,
6.84875224238385));
#103200=CARTESIAN_POINT('Ctrl Pts',(2.91533116449869,0.395231832349964,
6.84370851892793));
#103201=CARTESIAN_POINT('Ctrl Pts',(2.92785613845147,0.302844418406204,
6.83865663289539));
#103202=CARTESIAN_POINT('Ctrl Pts',(2.93596919993952,0.20997905693951,6.83360474686285));
#103203=CARTESIAN_POINT('Ctrl Pts',(2.93966907772781,0.117088485560753,
6.82855286083031));
#103204=CARTESIAN_POINT('Ctrl Pts',(2.94153657557289,0.0702023580171901,
6.82600294247648));
#103205=CARTESIAN_POINT('Ctrl Pts',(2.94228056151857,0.0233097757748152,
6.82345302412264));
#103206=CARTESIAN_POINT('Ctrl Pts',(2.94190589024871,-0.0235315303354603,
6.8209031057688));
#103207=CARTESIAN_POINT('Ctrl Pts',(2.94116352440293,-0.116341918069838,
6.81585075068388));
#103208=CARTESIAN_POINT('Ctrl Pts',(2.93602358759243,-0.209283669915334,
6.81079839559896));
#103209=CARTESIAN_POINT('Ctrl Pts',(2.92646833053807,-0.301905797158144,
6.80574604051404));
#103210=CARTESIAN_POINT('Ctrl Pts',(2.91692624872714,-0.39440021260147,
6.80070065185689));
#103211=CARTESIAN_POINT('Ctrl Pts',(2.90298098961361,-0.48657544113512,
6.79565526319974));
#103212=CARTESIAN_POINT('Ctrl Pts',(2.88466680790186,-0.577980455888684,
6.79060987454259));
#103213=CARTESIAN_POINT('Ctrl Pts',(2.86637222038517,-0.669287677155403,
6.785569883906));
#103214=CARTESIAN_POINT('Ctrl Pts',(2.84371808791363,-0.759825889314803,
6.78052989326942));
#103215=CARTESIAN_POINT('Ctrl Pts',(2.81679034453784,-0.849150254618343,
6.77548990263283));
#103216=CARTESIAN_POINT('Ctrl Pts',(2.78988200315061,-0.938410259894014,
6.77045354341234));
#103217=CARTESIAN_POINT('Ctrl Pts',(2.75870629910473,-1.02645773259668,
6.76541718419185));
#103218=CARTESIAN_POINT('Ctrl Pts',(2.72339978133985,-1.11286011295133,
6.76038082497136));
#103219=CARTESIAN_POINT('Ctrl Pts',(2.68810609426371,-1.19923109394634,
6.75534629600663));
#103220=CARTESIAN_POINT('Ctrl Pts',(2.6486847435846,-1.28395775945165,6.7503117670419));
#103221=CARTESIAN_POINT('Ctrl Pts',(2.60532111200398,-1.36662573638372,
6.74527723807717));
#103222=CARTESIAN_POINT('Ctrl Pts',(2.56196110943974,-1.44928679499666,
6.74024313044219));
#103223=CARTESIAN_POINT('Ctrl Pts',(2.5146596884601,-1.52988911426925,6.73520902280721));
#103224=CARTESIAN_POINT('Ctrl Pts',(2.46364853664272,-1.60804225314454,
6.73017491517223));
#103225=CARTESIAN_POINT('Ctrl Pts',(2.41262738515996,-1.68621071230196,
6.72513982070614));
#103226=CARTESIAN_POINT('Ctrl Pts',(2.35789530169561,-1.76192866577616,
6.72010472624004));
#103227=CARTESIAN_POINT('Ctrl Pts',(2.29972705922584,-1.83483499341615,
6.71506963177394));
#103228=CARTESIAN_POINT('Ctrl Pts',(2.24149491351219,-1.90782141546228,
6.71002900578659));
#103229=CARTESIAN_POINT('Ctrl Pts',(2.17981935106033,-1.97798969821184,
6.70498837979924));
#103230=CARTESIAN_POINT('Ctrl Pts',(2.11501496842135,-2.04501239198046,
6.69994775381189));
#103231=CARTESIAN_POINT('Ctrl Pts',(2.05017076343912,-2.11207627124624,
6.69490403035597));
#103232=CARTESIAN_POINT('Ctrl Pts',(1.98219423402991,-2.1759904092918,6.68986030690005));
#103233=CARTESIAN_POINT('Ctrl Pts',(1.91143469560998,-2.23646627616389,
6.68481658344413));
#103234=CARTESIAN_POINT('Ctrl Pts',(1.84056064255445,-2.29704001495561,
6.6797646974116));
#103235=CARTESIAN_POINT('Ctrl Pts',(1.76689493960156,-2.3541641021299,6.67471281137906));
#103236=CARTESIAN_POINT('Ctrl Pts',(1.69081745894377,-2.40759222471974,
6.66966092534653));
#103237=CARTESIAN_POINT('Ctrl Pts',(1.65241766864856,-2.4345598462232,6.66711100699267));
#103238=CARTESIAN_POINT('Ctrl Pts',(1.61340385513976,-2.46058656595473,
6.66456108863881));
#103239=CARTESIAN_POINT('Ctrl Pts',(1.57382717536845,-2.48564519231361,
6.66201117028495));
#103240=CARTESIAN_POINT('Ctrl Pts',(1.49541076686486,-2.53529583234839,
6.65695881520003));
#103241=CARTESIAN_POINT('Ctrl Pts',(1.4145018071766,-2.58132113439736,6.6519064601151));
#103242=CARTESIAN_POINT('Ctrl Pts',(1.3314697723869,-2.62346188179283,6.64685410503018));
#103243=CARTESIAN_POINT('Ctrl Pts',(1.24855222612056,-2.66554452351914,
6.64180871637303));
#103244=CARTESIAN_POINT('Ctrl Pts',(1.1635178145737,-2.7037530547636,6.63676332771588));
#103245=CARTESIAN_POINT('Ctrl Pts',(1.07676421605117,-2.73787195154042,
6.63171793905872));
#103246=CARTESIAN_POINT('Ctrl Pts',(0.990103434502904,-2.77195434478517,
6.62667794842214));
#103247=CARTESIAN_POINT('Ctrl Pts',(0.901727533154306,-2.80195563875512,
6.62163795778556));
#103248=CARTESIAN_POINT('Ctrl Pts',(0.81205698217149,-2.8277071025314,6.61659796714897));
#103249=CARTESIAN_POINT('Ctrl Pts',(0.722451040650323,-2.85344001185259,
6.61156160792848));
#103250=CARTESIAN_POINT('Ctrl Pts',(0.631552729364438,-2.87492905504814,
6.60652524870799));
#103251=CARTESIAN_POINT('Ctrl Pts',(0.539799615584686,-2.89205469779094,
6.6014888894875));
#103252=CARTESIAN_POINT('Ctrl Pts',(0.448079845666546,-2.90917411692957,
6.59645436052277));
#103253=CARTESIAN_POINT('Ctrl Pts',(0.355506326638361,-2.92193320434845,
6.59141983155803));
#103254=CARTESIAN_POINT('Ctrl Pts',(0.262527791320864,-2.93026332584363,
6.5863853025933));
#103255=CARTESIAN_POINT('Ctrl Pts',(0.169557037192701,-2.93859275020746,
6.58135119495831));
#103256=CARTESIAN_POINT('Ctrl Pts',(0.0761817766508294,-2.94249390613339,
6.57631708732333));
#103257=CARTESIAN_POINT('Ctrl Pts',(-0.0171442912079515,-2.94195004602032,
6.57128297968835));
#103258=CARTESIAN_POINT('Ctrl Pts',(-0.110488653683019,-2.9414060792949,
6.56624788522225));
#103259=CARTESIAN_POINT('Ctrl Pts',(-0.203783360120329,-2.93641536897968,
6.56121279075615));
#103260=CARTESIAN_POINT('Ctrl Pts',(-0.296576018880584,-2.92701326697112,
6.55617769629006));
#103261=CARTESIAN_POINT('Ctrl Pts',(-0.389470619037941,-2.91760083587589,
6.5511370703027));
#103262=CARTESIAN_POINT('Ctrl Pts',(-0.481861627908431,-2.90376738411304,
6.54609644431535));
#103263=CARTESIAN_POINT('Ctrl Pts',(-0.573303384354947,-2.88559997738549,
6.54105581832799));
#103264=CARTESIAN_POINT('Ctrl Pts',(-0.664801331831481,-2.86742140677248,
6.53601209487207));
#103265=CARTESIAN_POINT('Ctrl Pts',(-0.755348434826439,-2.84490368637615,
6.53096837141616));
#103266=CARTESIAN_POINT('Ctrl Pts',(-0.844512940296811,-2.81818414828968,
6.52592464796024));
#103267=CARTESIAN_POINT('Ctrl Pts',(-0.933821746324855,-2.79142136828508,
6.5208727619277));
#103268=CARTESIAN_POINT('Ctrl Pts',(-1.02174306938939,-2.76044334256319,
6.51582087589516));
#103269=CARTESIAN_POINT('Ctrl Pts',(-1.10786409070903,-2.72543595714841,
6.51076898986263));
#103270=CARTESIAN_POINT('Ctrl Pts',(-1.15133331616283,-2.70776612572019,
6.50821907150878));
#103271=CARTESIAN_POINT('Ctrl Pts',(-1.19434425278957,-2.68907048144247,
6.50566915315492));
#103272=CARTESIAN_POINT('Ctrl Pts',(-1.23684633263854,-2.66937729619449,
6.50311923480107));
#103273=CARTESIAN_POINT('Ctrl Pts',(-1.32105906788969,-2.63035762935858,
6.49806687971615));
#103274=CARTESIAN_POINT('Ctrl Pts',(-1.40357462284592,-2.5872789643746,
6.49301452463123));
#103275=CARTESIAN_POINT('Ctrl Pts',(-1.48397496366263,-2.54031145870393,
6.4879621695463));
#103276=CARTESIAN_POINT('Ctrl Pts',(-1.56426444466102,-2.49340871406652,
6.48291678088914));
#103277=CARTESIAN_POINT('Ctrl Pts',(-1.64244412683902,-2.44262800610038,
6.47787139223199));
#103278=CARTESIAN_POINT('Ctrl Pts',(-1.71811742649312,-2.38818686638643,
6.47282600357483));
#103279=CARTESIAN_POINT('Ctrl Pts',(-1.79370976389519,-2.33380397280811,
6.46778601293824));
#103280=CARTESIAN_POINT('Ctrl Pts',(-1.86680069010308,-2.27576868970264,
6.46274602230166));
#103281=CARTESIAN_POINT('Ctrl Pts',(-1.9370206084162,-2.21434305440032,
6.45770603166507));
#103282=CARTESIAN_POINT('Ctrl Pts',(-2.00718993184539,-2.15296167752158,
6.45266967244457));
#103283=CARTESIAN_POINT('Ctrl Pts',(-2.07449202565071,-2.08819509554047,
6.44763331322408));
#103284=CARTESIAN_POINT('Ctrl Pts',(-2.13858938528684,-2.0203463666259,
6.44259695400358));
#103285=CARTESIAN_POINT('Ctrl Pts',(-2.20266345139744,-1.95252229451635,
6.43756242503885));
#103286=CARTESIAN_POINT('Ctrl Pts',(-2.26353479223544,-1.88161862323202,
6.43252789607412));
#103287=CARTESIAN_POINT('Ctrl Pts',(-2.32090264043655,-1.80797536864158,
6.42749336710939));
#103288=CARTESIAN_POINT('Ctrl Pts',(-2.37826568763615,-1.73433827710915,
6.42245925947441));
#103289=CARTESIAN_POINT('Ctrl Pts',(-2.43212555229379,-1.65796240868285,
6.41742515183943));
#103290=CARTESIAN_POINT('Ctrl Pts',(-2.48222239153612,-1.57922006033254,
6.41239104420445));
#103291=CARTESIAN_POINT('Ctrl Pts',(-2.53232905121202,-1.500462276198,6.40735594973836));
#103292=CARTESIAN_POINT('Ctrl Pts',(-2.57867098233763,-1.41933746582406,
6.40232085527227));
#103293=CARTESIAN_POINT('Ctrl Pts',(-2.62103284391699,-1.33624504904917,
6.39728576080618));
#103294=CARTESIAN_POINT('Ctrl Pts',(-2.6634412439555,-1.25306134749833,
6.39224513481882));
#103295=CARTESIAN_POINT('Ctrl Pts',(-2.70186064439241,-1.1679061211299,
6.38720450883146));
#103296=CARTESIAN_POINT('Ctrl Pts',(-2.73612281952669,-1.08120114523864,
6.38216388284411));
#103297=CARTESIAN_POINT('Ctrl Pts',(-2.77040604879409,-0.994442889072623,
6.37712015938818));
#103298=CARTESIAN_POINT('Ctrl Pts',(-2.80052682370888,-0.906133407638423,
6.37207643593226));
#103299=CARTESIAN_POINT('Ctrl Pts',(-2.82636670524513,-0.816710014314636,
6.36703271247633));
#103300=CARTESIAN_POINT('Ctrl Pts',(-2.85224840509566,-0.727141901458713,
6.3619808264438));
#103301=CARTESIAN_POINT('Ctrl Pts',(-2.87383527787349,-0.636456709444174,
6.35692894041126));
#103302=CARTESIAN_POINT('Ctrl Pts',(-2.89105995440951,-0.545102137227228,
6.35187705437872));
#103303=CARTESIAN_POINT('Ctrl Pts',(-2.89975403787761,-0.49899129883871,
6.34932713602488));
#103304=CARTESIAN_POINT('Ctrl Pts',(-2.90733759523971,-0.452710012748207,
6.34677721767104));
#103305=CARTESIAN_POINT('Ctrl Pts',(-2.91380699892608,-0.40631609986484,
6.3442272993172));
#103306=CARTESIAN_POINT('Ctrl Pts',(-2.93245570054395,-0.27258101697472,
6.33687690524133));
#103307=CARTESIAN_POINT('Ctrl Pts',(-2.9419003072094,-0.137533302805858,
6.32952651116546));
#103308=CARTESIAN_POINT('Ctrl Pts',(-2.9419992148765,-0.00214934084322361,
6.3221761170896));
#103309=CARTESIAN_POINT('',(-2.94170074019424,-0.00106841483045282,5.32217617144154));
#103310=CARTESIAN_POINT('Ctrl Pts',(-2.94471353758293,-0.00212782599804863,
6.32217484249879));
#103311=CARTESIAN_POINT('Ctrl Pts',(-2.93780032435234,0.838783439956008,
6.27656168294363));
#103312=CARTESIAN_POINT('Ctrl Pts',(-2.11923631689247,2.66785949385505,
6.17798454489385));
#103313=CARTESIAN_POINT('Ctrl Pts',(0.985754882321845,3.33559704112804,
6.02644342834946));
#103314=CARTESIAN_POINT('Ctrl Pts',(3.33780171542183,0.978263776969118,
5.86755149286558));
#103315=CARTESIAN_POINT('Ctrl Pts',(2.63036689099525,-2.27576148301134,
5.70865955738172));
#103316=CARTESIAN_POINT('Ctrl Pts',(-0.488103681415864,-3.44378790069809,
5.54976762189784));
#103317=CARTESIAN_POINT('Ctrl Pts',(-2.65377056339368,-1.83145342118466,
5.42094007970052));
#103318=CARTESIAN_POINT('Ctrl Pts',(-2.93890109085433,-0.425887727767073,
5.34507651599781));
#103319=CARTESIAN_POINT('Ctrl Pts',(-2.93752250330966,-0.0010809852794131,
5.32217693078973));
#103320=CARTESIAN_POINT('',(-2.94199880936505,0.00264682727074493,4.32217611708959));
#103321=CARTESIAN_POINT('Ctrl Pts',(-2.94199980632419,-0.00106751507401821,
5.32217611708959));
#103322=CARTESIAN_POINT('Ctrl Pts',(-2.9420345110113,0.0945762704193298,
5.31702819360726));
#103323=CARTESIAN_POINT('Ctrl Pts',(-2.93740083055662,0.190188226245283,
5.31188027012492));
#103324=CARTESIAN_POINT('Ctrl Pts',(-2.92813433093512,0.285295180469558,
5.30673234664258));
#103325=CARTESIAN_POINT('Ctrl Pts',(-2.91886212799877,0.380460670810617,
5.30158125473316));
#103326=CARTESIAN_POINT('Ctrl Pts',(-2.90495147051173,0.475120127456848,
5.29643016282373));
#103327=CARTESIAN_POINT('Ctrl Pts',(-2.88648955217386,0.568807581868541,
5.2912790709143));
#103328=CARTESIAN_POINT('Ctrl Pts',(-2.86799656128149,0.662652718081264,
5.28611930939746));
#103329=CARTESIAN_POINT('Ctrl Pts',(-2.84493708928312,0.755522175674526,
5.28095954788062));
#103330=CARTESIAN_POINT('Ctrl Pts',(-2.81744913705144,0.84696184101061,
5.27579978636378));
#103331=CARTESIAN_POINT('Ctrl Pts',(-2.78993722170672,0.938481220507241,
5.27063552673272));
#103332=CARTESIAN_POINT('Ctrl Pts',(-2.7579892716372,1.02856793235365,5.26547126710167));
#103333=CARTESIAN_POINT('Ctrl Pts',(-2.72179192390167,1.11678678492525,
5.26030700747062));
#103334=CARTESIAN_POINT('Ctrl Pts',(-2.68551790829933,1.20519248961893,
5.25513180966884));
#103335=CARTESIAN_POINT('Ctrl Pts',(-2.64497668398172,1.29172205155361,
5.24995661186705));
#103336=CARTESIAN_POINT('Ctrl Pts',(-2.60040169900902,1.37596330030674,
5.24478141406527));
#103337=CARTESIAN_POINT('Ctrl Pts',(-2.56365877865534,1.44540290853826,
5.24051552635355));
#103338=CARTESIAN_POINT('Ctrl Pts',(-2.52417597520646,1.51328808545775,
5.23624963864182));
#103339=CARTESIAN_POINT('Ctrl Pts',(-2.48210558902173,1.57940363585344,
5.23198375093009));
#103340=CARTESIAN_POINT('Ctrl Pts',(-2.43227902444048,1.6577083779861,5.22693139584518));
#103341=CARTESIAN_POINT('Ctrl Pts',(-2.37865392063076,1.73379343846384,
5.22187904076027));
#103342=CARTESIAN_POINT('Ctrl Pts',(-2.32145428796571,1.80726699435518,
5.21682668567535));
#103343=CARTESIAN_POINT('Ctrl Pts',(-2.26433352487776,1.8806392414092,5.2117812970182));
#103344=CARTESIAN_POINT('Ctrl Pts',(-2.20364829748771,1.95140679176675,
5.20673590836105));
#103345=CARTESIAN_POINT('Ctrl Pts',(-2.13966673299798,2.0192053564959,5.2016905197039));
#103346=CARTESIAN_POINT('Ctrl Pts',(-2.07575362186734,2.08693138408824,
5.19665052906732));
#103347=CARTESIAN_POINT('Ctrl Pts',(-2.00855148680339,2.15169441846654,
5.19161053843074));
#103348=CARTESIAN_POINT('Ctrl Pts',(-1.93836899559704,2.21316281301402,
5.18657054779416));
#103349=CARTESIAN_POINT('Ctrl Pts',(-1.86823707230764,2.27458691832899,
5.18153418857367));
#103350=CARTESIAN_POINT('Ctrl Pts',(-1.79512939437758,2.33272081033483,
5.17649782935319));
#103351=CARTESIAN_POINT('Ctrl Pts',(-1.71939103999525,2.38727008350209,
5.1714614701327));
#103352=CARTESIAN_POINT('Ctrl Pts',(-1.64368020957482,2.4417995329997,5.16642694116798));
#103353=CARTESIAN_POINT('Ctrl Pts',(-1.56534096203413,2.49274669221162,
5.16139241220325));
#103354=CARTESIAN_POINT('Ctrl Pts',(-1.48475014355556,2.53985846283051,
5.15635788323852));
#103355=CARTESIAN_POINT('Ctrl Pts',(-1.40416606956303,2.58696629075859,
5.15132377560356));
#103356=CARTESIAN_POINT('Ctrl Pts',(-1.32133118288554,2.63023914423385,
5.14628966796859));
#103357=CARTESIAN_POINT('Ctrl Pts',(-1.23664890784301,2.66946876339295,
5.14125556033363));
#103358=CARTESIAN_POINT('Ctrl Pts',(-1.15195003261822,2.70870607269532,
5.13622046586754));
#103359=CARTESIAN_POINT('Ctrl Pts',(-1.06540345303215,2.74389838720553,
5.13118537140146));
#103360=CARTESIAN_POINT('Ctrl Pts',(-0.977433585051243,2.77488514840054,
5.12615027693538));
#103361=CARTESIAN_POINT('Ctrl Pts',(-0.889367073959015,2.80590595144511,
5.12110965094803));
#103362=CARTESIAN_POINT('Ctrl Pts',(-0.799874572968278,2.83271183091539,
5.11606902496069));
#103363=CARTESIAN_POINT('Ctrl Pts',(-0.709396418217592,2.85519188879137,
5.11102839897334));
#103364=CARTESIAN_POINT('Ctrl Pts',(-0.61886266457064,2.87768576068036,
5.10598467551742));
#103365=CARTESIAN_POINT('Ctrl Pts',(-0.527342486780911,2.89584843256464,
5.1009409520615));
#103366=CARTESIAN_POINT('Ctrl Pts',(-0.435285030099101,2.90962041211077,
5.09589722860558));
#103367=CARTESIAN_POINT('Ctrl Pts',(-0.343078591013989,2.92341467972225,
5.09084534257305));
#103368=CARTESIAN_POINT('Ctrl Pts',(-0.250333578589815,2.93280402461145,
5.08579345654052));
#103369=CARTESIAN_POINT('Ctrl Pts',(-0.157502670145837,2.93778094978113,
5.080741570508));
#103370=CARTESIAN_POINT('Ctrl Pts',(-0.110646657217539,2.94029303195293,
5.07819165215408));
#103371=CARTESIAN_POINT('Ctrl Pts',(-0.0637687400751823,2.94168179722519,
5.07564173380016));
#103372=CARTESIAN_POINT('Ctrl Pts',(-0.016926710850602,2.94195130592941,
5.07309181544624));
#103373=CARTESIAN_POINT('Ctrl Pts',(0.075885109643817,2.94248530485926,
5.06803946036135));
#103374=CARTESIAN_POINT('Ctrl Pts',(0.168888755618728,2.93862395512216,
5.06298710527645));
#103375=CARTESIAN_POINT('Ctrl Pts',(0.261633525086621,2.93034330728513,
5.05793475019156));
#103376=CARTESIAN_POINT('Ctrl Pts',(0.354250413650165,2.92207407719963,
5.05288936153444));
#103377=CARTESIAN_POINT('Ctrl Pts',(0.446608696373017,2.90939769682623,
5.04784397287732));
#103378=CARTESIAN_POINT('Ctrl Pts',(0.538256917974871,2.89234221527332,
5.04279858422019));
#103379=CARTESIAN_POINT('Ctrl Pts',(0.629807085884844,2.87530498124234,
5.03775859358363));
#103380=CARTESIAN_POINT('Ctrl Pts',(0.720648268274743,2.85389803935472,
5.03271860294707));
#103381=CARTESIAN_POINT('Ctrl Pts',(0.810334487725388,2.82820119828891,
5.02767861231051));
#103382=CARTESIAN_POINT('Ctrl Pts',(0.899956086424732,2.80252287232147,
5.02264225309005));
#103383=CARTESIAN_POINT('Ctrl Pts',(0.988423950419802,2.77256091290418,
5.01760589386959));
#103384=CARTESIAN_POINT('Ctrl Pts',(1.0753036830665,2.7384459076607,5.01256953464914));
#103385=CARTESIAN_POINT('Ctrl Pts',(1.16215184287962,2.7043433001002,5.00753500568444));
#103386=CARTESIAN_POINT('Ctrl Pts',(1.24741260480997,2.66609080721475,5.00250047671975));
#103387=CARTESIAN_POINT('Ctrl Pts',(1.33066908564115,2.62386809586895,4.99746594775506));
#103388=CARTESIAN_POINT('Ctrl Pts',(1.41391859890251,2.58164891805815,4.99243184012011));
#103389=CARTESIAN_POINT('Ctrl Pts',(1.49516376844178,2.53546038349343,4.98739773248516));
#103390=CARTESIAN_POINT('Ctrl Pts',(1.57401100403843,2.48552878864155,4.98236362485022));
#103391=CARTESIAN_POINT('Ctrl Pts',(1.65287369598042,2.43558740574869,4.97732853038415));
#103392=CARTESIAN_POINT('Ctrl Pts',(1.72933714533686,2.38190174331353,4.97229343591808));
#103393=CARTESIAN_POINT('Ctrl Pts',(1.80303648752597,2.32474158233771,4.96725834145201));
#103394=CARTESIAN_POINT('Ctrl Pts',(1.87681679532157,2.26751862558971,4.96221771546469));
#103395=CARTESIAN_POINT('Ctrl Pts',(1.94782658290908,2.20681382368379,4.95717708947737));
#103396=CARTESIAN_POINT('Ctrl Pts',(2.01573410535022,2.14293724045478,4.95213646349006));
#103397=CARTESIAN_POINT('Ctrl Pts',(2.08368335701646,2.07902140501595,4.94709274003417));
#103398=CARTESIAN_POINT('Ctrl Pts',(2.14852623987871,2.01193022724544,4.94204901657828));
#103399=CARTESIAN_POINT('Ctrl Pts',(2.20996944760846,1.94200902177028,4.93700529312239));
#103400=CARTESIAN_POINT('Ctrl Pts',(2.27151209276674,1.87197465838672,4.93195340708989));
#103401=CARTESIAN_POINT('Ctrl Pts',(2.32964380225102,1.79910147072921,4.92690152105739));
#103402=CARTESIAN_POINT('Ctrl Pts',(2.38411306252143,1.72376590786415,4.92184963502488));
#103403=CARTESIAN_POINT('Ctrl Pts',(2.41160619391993,1.68574059746802,4.91929971667071));
#103404=CARTESIAN_POINT('Ctrl Pts',(2.43816695633939,1.64708838298131,4.91674979831653));
#103405=CARTESIAN_POINT('Ctrl Pts',(2.46376745725854,1.60786004258885,4.91419987996235));
#103406=CARTESIAN_POINT('Ctrl Pts',(2.51449175624882,1.53013382647908,4.90914752487733));
#103407=CARTESIAN_POINT('Ctrl Pts',(2.56162533671277,1.44986544055092,4.9040951697923));
#103408=CARTESIAN_POINT('Ctrl Pts',(2.60490392559348,1.36742076129759,4.89904281470728));
#103409=CARTESIAN_POINT('Ctrl Pts',(2.64812283989505,1.28508976069378,4.89399742605002));
#103410=CARTESIAN_POINT('Ctrl Pts',(2.68749712040228,1.20058881962297,4.88895203739277));
#103411=CARTESIAN_POINT('Ctrl Pts',(2.722805794782,1.1143126149791,4.88390664873551));
#103412=CARTESIAN_POINT('Ctrl Pts',(2.75807669269622,1.02812871654966,4.87886665809883));
#103413=CARTESIAN_POINT('Ctrl Pts',(2.7892904629384,0.940173738710766,4.87382666746214));
#103414=CARTESIAN_POINT('Ctrl Pts',(2.81627260839231,0.850865791543631,
4.86878667682545));
#103415=CARTESIAN_POINT('Ctrl Pts',(2.84323531265985,0.761622192574762,
4.86375031760486));
#103416=CARTESIAN_POINT('Ctrl Pts',(2.86597232429127,0.671027985947263,
4.85871395838427));
#103417=CARTESIAN_POINT('Ctrl Pts',(2.88435810299701,0.579519053763985,
4.85367759916368));
#103418=CARTESIAN_POINT('Ctrl Pts',(2.90273720015446,0.488043376704628,
4.84864307019884));
#103419=CARTESIAN_POINT('Ctrl Pts',(2.9167681183433,0.395654069573802,4.84360854123401));
#103420=CARTESIAN_POINT('Ctrl Pts',(2.92637605903953,0.302798878928364,
4.83857401226918));
#103421=CARTESIAN_POINT('Ctrl Pts',(2.93598319566624,0.209951459149804,
4.8335399046341));
#103422=CARTESIAN_POINT('Ctrl Pts',(2.94116804520858,0.116638675275587,
4.82850579699901));
#103423=CARTESIAN_POINT('Ctrl Pts',(2.94190762254467,0.023313953194666,
4.82347168936393));
#103424=CARTESIAN_POINT('Ctrl Pts',(2.94264734485937,-0.0700290632391486,
4.81843659489771));
#103425=CARTESIAN_POINT('Ctrl Pts',(2.93894006120845,-0.16338357832546,
4.81340150043149));
#103426=CARTESIAN_POINT('Ctrl Pts',(2.93081489902085,-0.256296757055925,
4.80836640596527));
#103427=CARTESIAN_POINT('Ctrl Pts',(2.92268081058422,-0.349312009585432,
4.80332577997782));
#103428=CARTESIAN_POINT('Ctrl Pts',(2.91011919431999,-0.441884514709381,
4.79828515399038));
#103429=CARTESIAN_POINT('Ctrl Pts',(2.89321097912903,-0.533567456135797,
4.79324452800293));
#103430=CARTESIAN_POINT('Ctrl Pts',(2.87629237382679,-0.625306736800511,
4.78820080454692));
#103431=CARTESIAN_POINT('Ctrl Pts',(2.85502195337702,-0.71615493329788,
4.7831570810909));
#103432=CARTESIAN_POINT('Ctrl Pts',(2.82953109957676,-0.805678444869855,
4.77811335763489));
#103433=CARTESIAN_POINT('Ctrl Pts',(2.80399899231585,-0.895346838001744,
4.77306147160227));
#103434=CARTESIAN_POINT('Ctrl Pts',(2.77423295776426,-0.983685845888612,
4.76800958556964));
#103435=CARTESIAN_POINT('Ctrl Pts',(2.74041318743611,-1.07028013254767,
4.76295769953702));
#103436=CARTESIAN_POINT('Ctrl Pts',(2.72334279976471,-1.11398823668486,
4.76040778118417));
#103437=CARTESIAN_POINT('Ctrl Pts',(2.70524039402295,-1.15725220193419,
4.75785786283133));
#103438=CARTESIAN_POINT('Ctrl Pts',(2.68613354402471,-1.2000210763421,4.75530794447849));
#103439=CARTESIAN_POINT('Ctrl Pts',(2.64827562961882,-1.28476243280432,
4.75025558939365));
#103440=CARTESIAN_POINT('Ctrl Pts',(2.60633576187254,-1.36786258731512,
4.74520323430881));
#103441=CARTESIAN_POINT('Ctrl Pts',(2.56047833350861,-1.44890120561512,
4.74015087922396));
#103442=CARTESIAN_POINT('Ctrl Pts',(2.51468413555046,-1.52982808400947,
4.73510549056689));
#103443=CARTESIAN_POINT('Ctrl Pts',(2.46498332777356,-1.60869869141865,
4.73006010190981));
#103444=CARTESIAN_POINT('Ctrl Pts',(2.41158796751508,-1.68511349022447,
4.72501471325273));
#103445=CARTESIAN_POINT('Ctrl Pts',(2.35824973452142,-1.76144653345404,
4.71997472261624));
#103446=CARTESIAN_POINT('Ctrl Pts',(2.3012250588703,-1.83532862834624,4.71493473197975));
#103447=CARTESIAN_POINT('Ctrl Pts',(2.24077087055533,-1.90638660970714,
4.70989474134326));
#103448=CARTESIAN_POINT('Ctrl Pts',(2.18036024071641,-1.97739339234278,
4.70485838212285));
#103449=CARTESIAN_POINT('Ctrl Pts',(2.11652529677877,-2.04557976857979,
4.69982202290243));
#103450=CARTESIAN_POINT('Ctrl Pts',(2.04956442701537,-2.11060409824134,
4.69478566368202));
#103451=CARTESIAN_POINT('Ctrl Pts',(1.98262789140132,-2.17560479750869,
4.68975113471736));
#103452=CARTESIAN_POINT('Ctrl Pts',(1.91256800510489,-2.23744542387134,
4.68471660575271));
#103453=CARTESIAN_POINT('Ctrl Pts',(1.8397206158004,-2.29582056263093,4.67968207678805));
#103454=CARTESIAN_POINT('Ctrl Pts',(1.76687932294954,-2.35419081609086,
4.67464796915315));
#103455=CARTESIAN_POINT('Ctrl Pts',(1.69125133769096,-2.40909588092382,
4.66961386151824));
#103456=CARTESIAN_POINT('Ctrl Pts',(1.61320534852639,-2.46027081913472,
4.66457975388334));
#103457=CARTESIAN_POINT('Ctrl Pts',(1.53514406008434,-2.51145578911777,
4.65954465941733));
#103458=CARTESIAN_POINT('Ctrl Pts',(1.4546641980517,-2.55890893701755,4.65450956495132));
#103459=CARTESIAN_POINT('Ctrl Pts',(1.37216218320771,-2.60240944952455,
4.64947447048531));
#103460=CARTESIAN_POINT('Ctrl Pts',(1.28956953219932,-2.64595775140506,
4.64443384449803));
#103461=CARTESIAN_POINT('Ctrl Pts',(1.20495068753058,-2.68554454256647,
4.63939321851076));
#103462=CARTESIAN_POINT('Ctrl Pts',(1.1187250712355,-2.72099581311496,4.63435259252348));
#103463=CARTESIAN_POINT('Ctrl Pts',(1.03244646923242,-2.75646886849666,
4.62930886906763));
#103464=CARTESIAN_POINT('Ctrl Pts',(0.944559548089188,-2.7878011950038,
4.62426514561178));
#103465=CARTESIAN_POINT('Ctrl Pts',(0.855499951102573,-2.81486835103589,
4.61922142215593));
#103466=CARTESIAN_POINT('Ctrl Pts',(0.766296223338374,-2.8419793115582,
4.61416953612346));
#103467=CARTESIAN_POINT('Ctrl Pts',(0.675916461150174,-2.86481121278395,
4.609117650091));
#103468=CARTESIAN_POINT('Ctrl Pts',(0.584807394724338,-2.88329053532171,
4.60406576405853));
#103469=CARTESIAN_POINT('Ctrl Pts',(0.538820474342438,-2.89261789611677,
4.60151584570389));
#103470=CARTESIAN_POINT('Ctrl Pts',(0.492647850825972,-2.90083717974908,
4.59896592734925));
#103471=CARTESIAN_POINT('Ctrl Pts',(0.446347289731649,-2.9079439638599,
4.59641600899461));
#103472=CARTESIAN_POINT('Ctrl Pts',(0.35460832293488,-2.92202519778373,
4.59136365390988));
#103473=CARTESIAN_POINT('Ctrl Pts',(0.26203775074848,-2.93178620956139,
4.58631129882515));
#103474=CARTESIAN_POINT('Ctrl Pts',(0.16907794671422,-2.93713749217412,
4.58125894374042));
#103475=CARTESIAN_POINT('Ctrl Pts',(0.0762463200841915,-2.94248139618358,
4.57621355508346));
#103476=CARTESIAN_POINT('Ctrl Pts',(-0.0169730322596317,-2.94342762814871,
4.57116816642649));
#103477=CARTESIAN_POINT('Ctrl Pts',(-0.11012939840714,-2.93993801220476,
4.56612277776953));
#103478=CARTESIAN_POINT('Ctrl Pts',(-0.203186097311192,-2.93645212977271,
4.56108278713312));
#103479=CARTESIAN_POINT('Ctrl Pts',(-0.296179502418778,-2.92853984913072,
4.55604279649672));
#103480=CARTESIAN_POINT('Ctrl Pts',(-0.388656762707934,-2.91621499907009,
4.55100280586031));
#103481=CARTESIAN_POINT('Ctrl Pts',(-0.481067391243812,-2.90389902931546,
4.54596644664001));
#103482=CARTESIAN_POINT('Ctrl Pts',(-0.57296217506985,-2.88717686806095,
4.54093008741971));
#103483=CARTESIAN_POINT('Ctrl Pts',(-0.663892304744306,-2.86611426982619,
4.53589372819941));
#103484=CARTESIAN_POINT('Ctrl Pts',(-0.754789389636509,-2.8450593259187,
4.53085919923488));
#103485=CARTESIAN_POINT('Ctrl Pts',(-0.844722084464464,-2.8196671787591,
4.52582467027034));
#103486=CARTESIAN_POINT('Ctrl Pts',(-0.933251738626908,-2.79005469343342,
4.5207901413058));
#103487=CARTESIAN_POINT('Ctrl Pts',(-1.02177398391817,-2.76044468631791,
4.51575603367101));
#103488=CARTESIAN_POINT('Ctrl Pts',(-1.10889300076054,-2.72661518436128,
4.51072192603622));
#103489=CARTESIAN_POINT('Ctrl Pts',(-1.19418637272005,-2.68873258380407,
4.50568781840143));
#103490=CARTESIAN_POINT('Ctrl Pts',(-1.27949646465428,-2.65084255715843,
4.50065272393553));
#103491=CARTESIAN_POINT('Ctrl Pts',(-1.36297979513366,-2.60889803463047,
4.49561762946964));
#103492=CARTESIAN_POINT('Ctrl Pts',(-1.44423601556269,-2.56311262556907,
4.49058253500374));
#103493=CARTESIAN_POINT('Ctrl Pts',(-1.52558150353447,-2.51727691696213,
4.48554190901659));
#103494=CARTESIAN_POINT('Ctrl Pts',(-1.60469460995704,-2.46759211748283,
4.48050128302944));
#103495=CARTESIAN_POINT('Ctrl Pts',(-1.68120186850992,-2.41431652384661,
4.47546065704229));
#103496=CARTESIAN_POINT('Ctrl Pts',(-1.75775614083244,-2.36100819231683,
4.47041693358656));
#103497=CARTESIAN_POINT('Ctrl Pts',(-1.83170102561651,-2.30410494455138,
4.46537321013084));
#103498=CARTESIAN_POINT('Ctrl Pts',(-1.90269593557739,-2.24390556323952,
4.46032948667512));
#103499=CARTESIAN_POINT('Ctrl Pts',(-1.97380574109052,-2.1836087574621,
4.45527760064277));
#103500=CARTESIAN_POINT('Ctrl Pts',(-2.04195571647358,-2.12000547152758,
4.45022571461044));
#103501=CARTESIAN_POINT('Ctrl Pts',(-2.10684207279745,-2.05343139166872,
4.44517382857809));
#103502=CARTESIAN_POINT('Ctrl Pts',(-2.13959318989923,-2.01982840316806,
4.44262391022231));
#103503=CARTESIAN_POINT('Ctrl Pts',(-2.17151347677769,-1.98546908022081,
4.44007399186653));
#103504=CARTESIAN_POINT('Ctrl Pts',(-2.202567924953,-1.95039958366696,4.43752407351075));
#103505=CARTESIAN_POINT('Ctrl Pts',(-2.26351815036058,-1.88156906676898,
4.43251937667381));
#103506=CARTESIAN_POINT('Ctrl Pts',(-2.32135890021934,-1.80974292607652,
4.42751467983687));
#103507=CARTESIAN_POINT('Ctrl Pts',(-2.37577747337919,-1.73523640953732,
4.42250998299993));
#103508=CARTESIAN_POINT('Ctrl Pts',(-2.43012647817473,-1.66082514166389,
4.41751168413619));
#103509=CARTESIAN_POINT('Ctrl Pts',(-2.48106172605355,-1.58374066173396,
4.41251338527245));
#103510=CARTESIAN_POINT('Ctrl Pts',(-2.52830867149839,-1.50433349415149,
4.40751508640872));
#103511=CARTESIAN_POINT('Ctrl Pts',(-2.57550903848734,-1.42500461021716,
4.4025217151237));
#103512=CARTESIAN_POINT('Ctrl Pts',(-2.6190280927908,-1.34335797234546,
4.39752834383869));
#103513=CARTESIAN_POINT('Ctrl Pts',(-2.65863353621515,-1.2597744719243,
4.39253497255368));
#103514=CARTESIAN_POINT('Ctrl Pts',(-2.69821151611528,-1.17624893064434,
4.38754506381223));
#103515=CARTESIAN_POINT('Ctrl Pts',(-2.73388108272753,-1.09078960304317,
4.38255515507078));
#103516=CARTESIAN_POINT('Ctrl Pts',(-2.76545562710603,-1.00380235828952,
4.37756524632933));
#103517=CARTESIAN_POINT('Ctrl Pts',(-2.79702472347893,-0.916830122683444,
4.37257619856787));
#103518=CARTESIAN_POINT('Ctrl Pts',(-2.82450003557403,-0.828330915147752,
4.3675871508064));
#103519=CARTESIAN_POINT('Ctrl Pts',(-2.8477432903,-0.738730094521212,4.36259810304494));
#103520=CARTESIAN_POINT('Ctrl Pts',(-2.87098353801618,-0.649140865668232,
4.35760970072301));
#103521=CARTESIAN_POINT('Ctrl Pts',(-2.88999270855973,-0.558450747278933,
4.35262129840107));
#103522=CARTESIAN_POINT('Ctrl Pts',(-2.90468299020389,-0.467098197834468,
4.34763289607914));
#103523=CARTESIAN_POINT('Ctrl Pts',(-2.91938238808987,-0.375688958399173,
4.34264139814047));
#103524=CARTESIAN_POINT('Ctrl Pts',(-2.92975747686044,-0.283616915626116,
4.33764990020179));
#103525=CARTESIAN_POINT('Ctrl Pts',(-2.9357720645064,-0.191327952123688,
4.33265840226312));
#103526=CARTESIAN_POINT('Ctrl Pts',(-2.93998233189044,-0.126724817908505,
4.32916430720527));
#103527=CARTESIAN_POINT('Ctrl Pts',(-2.9420569841351,-0.0620155351335664,
4.32567021214743));
#103528=CARTESIAN_POINT('Ctrl Pts',(-2.94199880936505,0.00264682727074493,
4.32217611708959));
#103529=CARTESIAN_POINT('',(-2.94245552567036,-0.000355218061749572,3.3221761170896));
#103530=CARTESIAN_POINT('Ctrl Pts',(-2.94080193791859,0.00265685637863251,
4.32217551672762));
#103531=CARTESIAN_POINT('Ctrl Pts',(-2.9431405362452,0.271157122569686,
4.3076610571607));
#103532=CARTESIAN_POINT('Ctrl Pts',(-2.78627811663743,1.51674327414858,
4.24018261909918));
#103533=CARTESIAN_POINT('Ctrl Pts',(-1.02407150506552,3.32403337258514,
4.119740202543));
#103534=CARTESIAN_POINT('Ctrl Pts',(2.23937444558007,2.66141360932405,3.96084826705914));
#103535=CARTESIAN_POINT('Ctrl Pts',(3.45017448606169,-0.440699812455072,
3.80195633157526));
#103536=CARTESIAN_POINT('Ctrl Pts',(1.49849021612704,-3.13886084204111,
3.6430643960914));
#103537=CARTESIAN_POINT('Ctrl Pts',(-1.82673380221927,-2.95989255113387,
3.48417246060752));
#103538=CARTESIAN_POINT('Ctrl Pts',(-2.93802558998807,-1.01302275008816,
3.37720970094026));
#103539=CARTESIAN_POINT('Ctrl Pts',(-2.94682272625454,-0.0193976123279483,
3.32321091976762));
#103540=CARTESIAN_POINT('Ctrl Pts',(-2.9467902630953,-0.000355741358367689,
3.3221761170896));
#103541=CARTESIAN_POINT('',(-2.94199898604255,-0.00244256517021028,2.32217614961572));
#103542=CARTESIAN_POINT('Ctrl Pts',(-2.94199997856207,-0.000355163067354804,
3.3221761170896));
#103543=CARTESIAN_POINT('Ctrl Pts',(-2.94201114633791,0.0921533191625664,
3.3171406920142));
#103544=CARTESIAN_POINT('Ctrl Pts',(-2.93765476336845,0.184833200119386,
3.3121052669388));
#103545=CARTESIAN_POINT('Ctrl Pts',(-2.928908341081,0.277236234186919,3.30706984186339));
#103546=CARTESIAN_POINT('Ctrl Pts',(-2.92017394505773,0.369512214784784,
3.30204134045921));
#103547=CARTESIAN_POINT('Ctrl Pts',(-2.90706154442541,0.461511663166572,
3.29701283905502));
#103548=CARTESIAN_POINT('Ctrl Pts',(-2.88960065316893,0.552785731731266,
3.29198433765083));
#103549=CARTESIAN_POINT('Ctrl Pts',(-2.87142912184824,0.647774559697056,
3.2867511814837));
#103550=CARTESIAN_POINT('Ctrl Pts',(-2.84854757434183,0.741977213308869,
3.28151802531657));
#103551=CARTESIAN_POINT('Ctrl Pts',(-2.82104910386007,0.83489277970905,
3.27628486914945));
#103552=CARTESIAN_POINT('Ctrl Pts',(-2.79467306622296,0.924015717585553,
3.27126532000337));
#103553=CARTESIAN_POINT('Ctrl Pts',(-2.76404977901021,1.01195410927705,
3.2662457708573));
#103554=CARTESIAN_POINT('Ctrl Pts',(-2.72931331381235,1.09827721229507,
3.26122622171123));
#103555=CARTESIAN_POINT('Ctrl Pts',(-2.69458840529123,1.18457159597764,
3.25620834254817));
#103556=CARTESIAN_POINT('Ctrl Pts',(-2.65575320396844,1.26925134360697,
3.25119046338511));
#103557=CARTESIAN_POINT('Ctrl Pts',(-2.6129906737564,1.35190374615284,3.24617258422205));
#103558=CARTESIAN_POINT('Ctrl Pts',(-2.57023019747324,1.4345521788177,3.24115494607295));
#103559=CARTESIAN_POINT('Ctrl Pts',(-2.5235429735275,1.51517306272391,3.23613730792386));
#103560=CARTESIAN_POINT('Ctrl Pts',(-2.47315832393181,1.59337751483031,
3.23111966977476));
#103561=CARTESIAN_POINT('Ctrl Pts',(-2.42276175155821,1.67160047285709,
3.22610084427623));
#103562=CARTESIAN_POINT('Ctrl Pts',(-2.36866625893787,1.7474054877297,3.2210820187777));
#103563=CARTESIAN_POINT('Ctrl Pts',(-2.31114429061703,1.82043293420777,
3.21606319327917));
#103564=CARTESIAN_POINT('Ctrl Pts',(-2.25355816621311,1.89354183052248,
3.21103877012474));
#103565=CARTESIAN_POINT('Ctrl Pts',(-2.19253821770682,1.96386662495742,
3.2060143469703));
#103566=CARTESIAN_POINT('Ctrl Pts',(-2.12839669278391,2.03108136669768,
3.20098992381587));
#103567=CARTESIAN_POINT('Ctrl Pts',(-2.06421283811086,2.09834046633599,
3.19596218482856));
#103568=CARTESIAN_POINT('Ctrl Pts',(-1.99690363100382,2.16248512071508,
3.19093444584125));
#103569=CARTESIAN_POINT('Ctrl Pts',(-1.92681600729287,2.22322830002678,
3.18590670685395));
#103570=CARTESIAN_POINT('Ctrl Pts',(-1.85661932603274,2.28406599677129,
3.18087114461821));
#103571=CARTESIAN_POINT('Ctrl Pts',(-1.78363595308645,2.3414913825842,3.17583558238248));
#103572=CARTESIAN_POINT('Ctrl Pts',(-1.70824317556668,2.39525974648468,
3.17080002014675));
#103573=CARTESIAN_POINT('Ctrl Pts',(-1.68622709717687,2.41096109817205,
3.16932954331109));
#103574=CARTESIAN_POINT('Ctrl Pts',(-1.66400572326432,2.42635089419769,
3.16785906647543));
#103575=CARTESIAN_POINT('Ctrl Pts',(-1.64158883621474,2.44142378394558,
3.16638858963977));
#103576=CARTESIAN_POINT('Ctrl Pts',(-1.56456751209218,2.4932121488585,3.1613362345682));
#103577=CARTESIAN_POINT('Ctrl Pts',(-1.48495488029135,2.54144509380551,
3.15628387949662));
#103578=CARTESIAN_POINT('Ctrl Pts',(-1.40311314851733,2.58585333931717,
3.15123152442505));
#103579=CARTESIAN_POINT('Ctrl Pts',(-1.32138426402925,2.6302003526204,3.14618613578179));
#103580=CARTESIAN_POINT('Ctrl Pts',(-1.23743277426245,2.6707329359363,3.14114074713852));
#103581=CARTESIAN_POINT('Ctrl Pts',(-1.1516502800556,2.70722471037183,3.13609535849526));
#103582=CARTESIAN_POINT('Ctrl Pts',(-1.06595956385464,2.74367744254915,
3.13105536787304));
#103583=CARTESIAN_POINT('Ctrl Pts',(-0.978442143574573,2.77609778596146,
3.12601537725082));
#103584=CARTESIAN_POINT('Ctrl Pts',(-0.889513690136257,2.80430551029309,
3.1209753866286));
#103585=CARTESIAN_POINT('Ctrl Pts',(-0.800649311475535,2.83249291037986,
3.11593902742316));
#103586=CARTESIAN_POINT('Ctrl Pts',(-0.710376342680051,2.85647359050147,
3.11090266821772));
#103587=CARTESIAN_POINT('Ctrl Pts',(-0.619128898248618,2.87611602814515,
3.10586630901228));
#103588=CARTESIAN_POINT('Ctrl Pts',(-0.527914613921933,2.89575132755835,
3.10083178006301));
#103589=CARTESIAN_POINT('Ctrl Pts',(-0.435726991337099,2.91105142309791,
3.09579725111375));
#103590=CARTESIAN_POINT('Ctrl Pts',(-0.343012706107742,2.92193536606282,
3.09076272216449));
#103591=CARTESIAN_POINT('Ctrl Pts',(-0.250306179960344,2.93281839817126,
3.08572861454536));
#103592=CARTESIAN_POINT('Ctrl Pts',(-0.157073520032592,2.93928596090582,
3.08069450692624));
#103593=CARTESIAN_POINT('Ctrl Pts',(-0.0637677932525789,2.94130883596805,
3.07566039930712));
#103594=CARTESIAN_POINT('Ctrl Pts',(0.0295562241494228,2.94333210757231,
3.07062530485725));
#103595=CARTESIAN_POINT('Ctrl Pts',(0.122952892733062,2.94090895186493,
3.06559021040739));
#103596=CARTESIAN_POINT('Ctrl Pts',(0.215969019761832,2.93406226629619,
3.06055511595753));
#103597=CARTESIAN_POINT('Ctrl Pts',(0.309087333680491,2.92720805900485,
3.05551448998685));
#103598=CARTESIAN_POINT('Ctrl Pts',(0.401823827821623,2.91592065407017,
3.05047386401618));
#103599=CARTESIAN_POINT('Ctrl Pts',(0.493730615240738,2.90027482828335,
3.04543323804551));
#103600=CARTESIAN_POINT('Ctrl Pts',(0.585693879446819,2.88461938812532,
3.04038951460655));
#103601=CARTESIAN_POINT('Ctrl Pts',(0.67682598833652,2.86460029047912,3.0353457911676));
#103602=CARTESIAN_POINT('Ctrl Pts',(0.766691575439549,2.84034294199662,
3.03030206772864));
#103603=CARTESIAN_POINT('Ctrl Pts',(0.856702597700644,2.81604633631429,
3.02525018171334));
#103604=CARTESIAN_POINT('Ctrl Pts',(0.94544258386381,2.78749792249483,3.02019829569804));
#103605=CARTESIAN_POINT('Ctrl Pts',(1.03249375929331,2.75487216346247,3.01514640968273));
#103606=CARTESIAN_POINT('Ctrl Pts',(1.07643247896761,2.73840444693582,3.01259649117379));
#103607=CARTESIAN_POINT('Ctrl Pts',(1.11994129363676,2.72089870215936,3.01004657266485));
#103608=CARTESIAN_POINT('Ctrl Pts',(1.16296887697036,2.70238179967197,3.00749665415591));
#103609=CARTESIAN_POINT('Ctrl Pts',(1.24822283225128,2.66569279568209,3.00244429885987));
#103610=CARTESIAN_POINT('Ctrl Pts',(1.33189187407922,2.62489965481643,2.99739194356383));
#103611=CARTESIAN_POINT('Ctrl Pts',(1.41355344725012,2.58016097400285,2.99233958826779));
#103612=CARTESIAN_POINT('Ctrl Pts',(1.49510242157254,2.53548398100332,2.98729419939875));
#103613=CARTESIAN_POINT('Ctrl Pts',(1.57464904137417,2.48687247022385,2.98224881052971));
#103614=CARTESIAN_POINT('Ctrl Pts',(1.65179089066202,2.43453298468638,2.97720342166067));
#103615=CARTESIAN_POINT('Ctrl Pts',(1.72885020651887,2.38224949673463,2.97216343081175));
#103616=CARTESIAN_POINT('Ctrl Pts',(1.80350950014496,2.32624620991823,2.96712343996282));
#103617=CARTESIAN_POINT('Ctrl Pts',(1.87539210840759,2.2667748983352,2.9620834491139));
#103618=CARTESIAN_POINT('Ctrl Pts',(1.94722292378378,2.20734643704602,2.95704708968125));
#103619=CARTESIAN_POINT('Ctrl Pts',(2.01628068909037,2.14445520004328,2.9520107302486));
#103620=CARTESIAN_POINT('Ctrl Pts',(2.08221969311326,2.0783948493035,2.94697437081595));
#103621=CARTESIAN_POINT('Ctrl Pts',(2.14813473434,2.01235850545831,2.94193984163925));
#103622=CARTESIAN_POINT('Ctrl Pts',(2.21093295235516,1.94315564991739,2.93690531246256));
#103623=CARTESIAN_POINT('Ctrl Pts',(2.27030434287066,1.87111789867517,2.93187078328586));
#103624=CARTESIAN_POINT('Ctrl Pts',(2.32967076470694,1.79908617613592,2.92683667543937));
#103625=CARTESIAN_POINT('Ctrl Pts',(2.38561064684502,1.72422037253094,2.92180256759289));
#103626=CARTESIAN_POINT('Ctrl Pts',(2.43785400625811,1.6468854981969,2.9167684597464));
#103627=CARTESIAN_POINT('Ctrl Pts',(2.49010760687746,1.56953546399552,2.91173336506948));
#103628=CARTESIAN_POINT('Ctrl Pts',(2.538662997306,1.4897157661196,2.90669827039257));
#103629=CARTESIAN_POINT('Ctrl Pts',(2.58329393366614,1.40781975134736,2.90166317571565));
#103630=CARTESIAN_POINT('Ctrl Pts',(2.62797390125282,1.32583376620074,2.89662254951984));
#103631=CARTESIAN_POINT('Ctrl Pts',(2.66872059585565,1.24176730164257,2.89158192332404));
#103632=CARTESIAN_POINT('Ctrl Pts',(2.70535425628224,1.15603734715431,2.88654129712823));
#103633=CARTESIAN_POINT('Ctrl Pts',(2.74201042811318,1.07025471156216,2.88149757346486));
#103634=CARTESIAN_POINT('Ctrl Pts',(2.77454837928104,0.982806967050958,
2.8764538498015));
#103635=CARTESIAN_POINT('Ctrl Pts',(2.8028376891304,0.894128004477065,2.87141012613814));
#103636=CARTESIAN_POINT('Ctrl Pts',(2.83117278133661,0.805305527199894,
2.86635823990179));
#103637=CARTESIAN_POINT('Ctrl Pts',(2.85524539090762,0.715248282604754,
2.86130635366543));
#103638=CARTESIAN_POINT('Ctrl Pts',(2.87497586211889,0.624401947653728,
2.85625446742907));
#103639=CARTESIAN_POINT('Ctrl Pts',(2.88493472636369,0.578547679540833,
2.85370455117673));
#103640=CARTESIAN_POINT('Ctrl Pts',(2.89378817376357,0.532492488326335,
2.85115463492438));
#103641=CARTESIAN_POINT('Ctrl Pts',(2.9015309880173,0.486294073144374,2.84860471867204));
#103642=CARTESIAN_POINT('Ctrl Pts',(2.91687245028162,0.394757427687029,
2.84355236397507));
#103643=CARTESIAN_POINT('Ctrl Pts',(2.92790553549581,0.302329845343127,
2.83850000927811));
#103644=CARTESIAN_POINT('Ctrl Pts',(2.93453466172541,0.209452426894869,
2.83344765458114));
#103645=CARTESIAN_POINT('Ctrl Pts',(2.94115464739987,0.116703072257054,
2.82840226631159));
#103646=CARTESIAN_POINT('Ctrl Pts',(2.94338270935698,0.0235055533119512,
2.82335687804205));
#103647=CARTESIAN_POINT('Ctrl Pts',(2.94117447729558,-0.0696899856870516,
2.8183114897725));
#103648=CARTESIAN_POINT('Ctrl Pts',(2.93896860780362,-0.162785815540424,
2.81327149952263));
#103649=CARTESIAN_POINT('Ctrl Pts',(2.93233588886659,-0.25587922792747,
2.80823150927276));
#103650=CARTESIAN_POINT('Ctrl Pts',(2.92128392050546,-0.348517224533101,
2.8031915190229));
#103651=CARTESIAN_POINT('Ctrl Pts',(2.91023991530746,-0.441088473618765,
2.7981551601863));
#103652=CARTESIAN_POINT('Ctrl Pts',(2.89478304212267,-0.533204519295604,
2.79311880134969));
#103653=CARTESIAN_POINT('Ctrl Pts',(2.87497287736889,-0.624415690380407,
2.78808244251309));
#103654=CARTESIAN_POINT('Ctrl Pts',(2.85516991179049,-0.715593714582038,
2.78304791393035));
#103655=CARTESIAN_POINT('Ctrl Pts',(2.83101689169364,-0.805867083784066,
2.77801338534761));
#103656=CARTESIAN_POINT('Ctrl Pts',(2.80262463893058,-0.89479558182817,
2.77297885676487));
#103657=CARTESIAN_POINT('Ctrl Pts',(2.77423476224573,-0.983716637663765,
2.76794474950951));
#103658=CARTESIAN_POINT('Ctrl Pts',(2.74160649355356,-1.07129262297736,
2.76291064225416));
#103659=CARTESIAN_POINT('Ctrl Pts',(2.70490040442368,-1.15709887310835,
2.7578765349988));
#103660=CARTESIAN_POINT('Ctrl Pts',(2.66818711981468,-1.24292194380224,
2.75284144090953));
#103661=CARTESIAN_POINT('Ctrl Pts',(2.62739460225923,-1.32697418206009,
2.74780634682026));
#103662=CARTESIAN_POINT('Ctrl Pts',(2.5827309354394,-1.40885233971639,2.74277125273098));
#103663=CARTESIAN_POINT('Ctrl Pts',(2.53801820135102,-1.49082044828437,
2.73773062711393));
#103664=CARTESIAN_POINT('Ctrl Pts',(2.48942604193384,-1.57060931806829,
2.73269000149688));
#103665=CARTESIAN_POINT('Ctrl Pts',(2.43720759368571,-1.64784196611226,
2.72764937587983));
#103666=CARTESIAN_POINT('Ctrl Pts',(2.38495705712568,-1.72512207373004,
2.72260565279105));
#103667=CARTESIAN_POINT('Ctrl Pts',(2.32907606136527,-1.79984247695622,
2.71756192970227));
#103668=CARTESIAN_POINT('Ctrl Pts',(2.26985867718656,-1.87165851201571,
2.71251820661349));
#103669=CARTESIAN_POINT('Ctrl Pts',(2.21054545766423,-1.94359077163483,
2.70746632093965));
#103670=CARTESIAN_POINT('Ctrl Pts',(2.14788536855418,-2.01260895098623,
2.70241443526581));
#103671=CARTESIAN_POINT('Ctrl Pts',(2.08220988672817,-2.07840467368881,
2.69736254959197));
#103672=CARTESIAN_POINT('Ctrl Pts',(2.04906041035026,-2.11161484124075,
2.69481262745737));
#103673=CARTESIAN_POINT('Ctrl Pts',(2.01514324348483,-2.14400465555415,
2.69226270532277));
#103674=CARTESIAN_POINT('Ctrl Pts',(1.98050406139377,-2.17553847651628,
2.68971278318817));
#103675=CARTESIAN_POINT('Ctrl Pts',(1.91187080920727,-2.23801883996161,
2.68466042807019));
#103676=CARTESIAN_POINT('Ctrl Pts',(1.84015484173131,-2.29736029386187,
2.67960807295222));
#103677=CARTESIAN_POINT('Ctrl Pts',(1.76567516219451,-2.35324355339803,
2.67455571783425));
#103678=CARTESIAN_POINT('Ctrl Pts',(1.6912981788371,-2.40904975839687,2.66951032914753));
#103679=CARTESIAN_POINT('Ctrl Pts',(1.61416540810677,-2.46140698000676,
2.66446494046082));
#103680=CARTESIAN_POINT('Ctrl Pts',(1.53463119590279,-2.51003408195227,
2.6594195517741));
#103681=CARTESIAN_POINT('Ctrl Pts',(1.45518207676411,-2.55860915812111,
2.65437956111142));
#103682=CARTESIAN_POINT('Ctrl Pts',(1.37333699997642,-2.60346181652224,
2.64933957044874));
#103683=CARTESIAN_POINT('Ctrl Pts',(1.28948086241099,-2.64435305991386,
2.64429957978605));
#103684=CARTESIAN_POINT('Ctrl Pts',(1.20568514499045,-2.68521484028797,
2.63926322054469));
#103685=CARTESIAN_POINT('Ctrl Pts',(1.11988164505737,-2.72212068479541,
2.63422686130334));
#103686=CARTESIAN_POINT('Ctrl Pts',(1.03248061797671,-2.75487708863797,
2.62919050206198));
#103687=CARTESIAN_POINT('Ctrl Pts',(0.945111353228246,-2.78762158850394,
2.62415597307961));
#103688=CARTESIAN_POINT('Ctrl Pts',(0.856146130235803,-2.81621948765529,
2.61912144409723));
#103689=CARTESIAN_POINT('Ctrl Pts',(0.766015015937392,-2.84052547873777,
2.61408691511486));
#103690=CARTESIAN_POINT('Ctrl Pts',(0.67589144459097,-2.86482943568448,
2.60905280746546));
#103691=CARTESIAN_POINT('Ctrl Pts',(0.584602604900241,-2.88484208321642,
2.60401869981607));
#103692=CARTESIAN_POINT('Ctrl Pts',(0.4925924406045,-2.90046835656921,2.59898459216667));
#103693=CARTESIAN_POINT('Ctrl Pts',(0.400564239707177,-2.91609769311473,
2.59394949768941));
#103694=CARTESIAN_POINT('Ctrl Pts',(0.307814871387626,-2.92733887379562,
2.58891440321214));
#103695=CARTESIAN_POINT('Ctrl Pts',(0.214796014112857,-2.93414837258126,
2.58387930873488));
#103696=CARTESIAN_POINT('Ctrl Pts',(0.121674967031744,-2.94096535223026,
2.57883868274127));
#103697=CARTESIAN_POINT('Ctrl Pts',(0.0282842837671854,-2.94334089918746,
2.57379805674766));
#103698=CARTESIAN_POINT('Ctrl Pts',(-0.0649220303857701,-2.94128358543861,
2.56875743075405));
#103699=CARTESIAN_POINT('Ctrl Pts',(-0.158185619839219,-2.93922500747001,
2.56371370729466));
#103700=CARTESIAN_POINT('Ctrl Pts',(-0.251264171800973,-2.93272817676389,
2.55866998383527));
#103701=CARTESIAN_POINT('Ctrl Pts',(-0.343708673950207,-2.92185358076879,
2.55362626037589));
#103702=CARTESIAN_POINT('Ctrl Pts',(-0.436302784803891,-2.91096138573664,
2.5485743743442));
#103703=CARTESIAN_POINT('Ctrl Pts',(-0.528260359646463,-2.89567735423824,
2.54352248831251));
#103704=CARTESIAN_POINT('Ctrl Pts',(-0.619142625915856,-2.87611307301608,
2.53847060228083));
#103705=CARTESIAN_POINT('Ctrl Pts',(-0.665015066951347,-2.86623808448856,
2.53592068408865));
#103706=CARTESIAN_POINT('Ctrl Pts',(-0.710613790669298,-2.85527341748435,
2.53337076589647));
#103707=CARTESIAN_POINT('Ctrl Pts',(-0.755884097136884,-2.84323815951031,
2.5308208477043));
#103708=CARTESIAN_POINT('Ctrl Pts',(-0.845581768488794,-2.81939174231928,
2.52576849127415));
#103709=CARTESIAN_POINT('Ctrl Pts',(-0.934310826130412,-2.79125374089853,
2.52071613484401));
#103710=CARTESIAN_POINT('Ctrl Pts',(-1.02163008489205,-2.75891934815852,
2.51566377841386));
#103711=CARTESIAN_POINT('Ctrl Pts',(-1.1088289438365,-2.72662953956903,
2.51061838840555));
#103712=CARTESIAN_POINT('Ctrl Pts',(-1.19462145369141,-2.69015499047006,
2.50557299839724));
#103713=CARTESIAN_POINT('Ctrl Pts',(-1.27857935125012,-2.64964126676741,
2.50052760838893));
#103714=CARTESIAN_POINT('Ctrl Pts',(-1.36244742302372,-2.60917088832644,
2.49548761639714));
#103715=CARTESIAN_POINT('Ctrl Pts',(-1.44448438599058,-2.56467011690487,
2.49044762440536));
#103716=CARTESIAN_POINT('Ctrl Pts',(-1.52428084884236,-2.51633302522787,
2.48540763241357));
#103717=CARTESIAN_POINT('Ctrl Pts',(-1.60401981673635,-2.46803076139844,
2.48037127183748));
#103718=CARTESIAN_POINT('Ctrl Pts',(-1.68152111434295,-2.41589790094858,
2.47533491126138));
#103719=CARTESIAN_POINT('Ctrl Pts',(-1.7563998537718,-2.36017447526034,
2.47029855068528));
#103720=CARTESIAN_POINT('Ctrl Pts',(-1.83125138163373,-2.30447129993607,
2.46526402036519));
#103721=CARTESIAN_POINT('Ctrl Pts',(-1.90348188864995,-2.24518041653238,
2.4602294900451));
#103722=CARTESIAN_POINT('Ctrl Pts',(-1.97273626882861,-2.18258461775212,
2.45519495972501));
#103723=CARTESIAN_POINT('Ctrl Pts',(-2.04198485322095,-2.11999405751236,
2.45016085073657));
#103724=CARTESIAN_POINT('Ctrl Pts',(-2.10825747653603,-2.05409942982767,
2.44512674174813));
#103725=CARTESIAN_POINT('Ctrl Pts',(-2.17123374859856,-1.98522240792982,
2.44009263275968));
#103726=CARTESIAN_POINT('Ctrl Pts',(-2.23422236578921,-1.91633188419021,
2.43505753694369));
#103727=CARTESIAN_POINT('Ctrl Pts',(-2.29391304893903,-1.84445813323679,
2.43002244112769));
#103728=CARTESIAN_POINT('Ctrl Pts',(-2.35002454030773,-1.76995724805754,
2.4249873453117));
#103729=CARTESIAN_POINT('Ctrl Pts',(-2.40619767521922,-1.69537451692497,
2.41994671798804));
#103730=CARTESIAN_POINT('Ctrl Pts',(-2.45878350181698,-1.61815924588878,
2.41490609066438));
#103731=CARTESIAN_POINT('Ctrl Pts',(-2.50754329433084,-1.53869770489738,
2.40986546334073));
#103732=CARTESIAN_POINT('Ctrl Pts',(-2.55633304971164,-1.45918733483068,
2.40482173855422));
#103733=CARTESIAN_POINT('Ctrl Pts',(-2.60129187653794,-1.37742833581499,
2.39977801376772));
#103734=CARTESIAN_POINT('Ctrl Pts',(-2.64222739263561,-1.29383090301864,
2.39473428898121));
#103735=CARTESIAN_POINT('Ctrl Pts',(-2.68322915707253,-1.21009817960876,
2.38968240163997));
#103736=CARTESIAN_POINT('Ctrl Pts',(-2.72019443614329,-1.12452149002621,
2.38463051429873));
#103737=CARTESIAN_POINT('Ctrl Pts',(-2.75297934735898,-1.03753010222109,
2.3795786269575));
#103738=CARTESIAN_POINT('Ctrl Pts',(-2.76952730270978,-0.993621805754092,
2.37702872204514));
#103739=CARTESIAN_POINT('Ctrl Pts',(-2.78501103996012,-0.949353323379518,
2.37447881713278));
#103740=CARTESIAN_POINT('Ctrl Pts',(-2.79941697330728,-0.904780973252142,
2.37192891222043));
#103741=CARTESIAN_POINT('Ctrl Pts',(-2.83367003860432,-0.798801056327432,
2.36586598957881));
#103742=CARTESIAN_POINT('Ctrl Pts',(-2.86192675554772,-0.690794327218017,
2.35980306693719));
#103743=CARTESIAN_POINT('Ctrl Pts',(-2.88398318981509,-0.581381940607001,
2.35374014429557));
#103744=CARTESIAN_POINT('Ctrl Pts',(-2.90578467662655,-0.473234237546983,
2.34774730218846));
#103745=CARTESIAN_POINT('Ctrl Pts',(-2.92152834520193,-0.363713232418249,
2.34175446008135));
#103746=CARTESIAN_POINT('Ctrl Pts',(-2.93106335006533,-0.253439613919819,
2.33576161797424));
#103747=CARTESIAN_POINT('Ctrl Pts',(-2.93826847380877,-0.170111385114324,
2.3312331285214));
#103748=CARTESIAN_POINT('Ctrl Pts',(-2.94192931955188,-0.0863538349346285,
2.32670463906856));
#103749=CARTESIAN_POINT('Ctrl Pts',(-2.94199898604255,-0.00244256517021028,
2.32217614961572));
#103750=CARTESIAN_POINT('',(-2.93804968218247,0.00161843370594106,1.3221761170896));
#103751=CARTESIAN_POINT('Ctrl Pts',(-2.93974867080922,-0.00244009463185479,
2.3221761170896));
#103752=CARTESIAN_POINT('Ctrl Pts',(-2.93448192828745,0.671152046916237,
2.28579640363858));
#103753=CARTESIAN_POINT('Ctrl Pts',(-2.36994396481666,2.3333813133397,2.19645271169295));
#103754=CARTESIAN_POINT('Ctrl Pts',(0.393212503661621,3.45590805701087,
2.05414504125267));
#103755=CARTESIAN_POINT('Ctrl Pts',(3.11795753103548,1.54151400144106,1.89525310576881));
#103756=CARTESIAN_POINT('Ctrl Pts',(2.98473289321859,-1.78585963759114,
1.73636117028493));
#103757=CARTESIAN_POINT('Ctrl Pts',(0.115656289204281,-3.47627940135573,
1.57746923480107));
#103758=CARTESIAN_POINT('Ctrl Pts',(-2.46940960925412,-2.17641804373625,
1.43940755040262));
#103759=CARTESIAN_POINT('Ctrl Pts',(-2.93508362518438,-0.594223152876953,
1.3543098444988));
#103760=CARTESIAN_POINT('Ctrl Pts',(-2.93804968218247,0.00161843370594106,
1.3221761170896));
#103761=CARTESIAN_POINT('Ctrl Pts',(-2.93804968218247,0.00161843370594106,
1.3221761170896));
#103762=CARTESIAN_POINT('Ctrl Pts',(-2.93997238822952,0.387864625988779,
1.30134586600417));
#103763=CARTESIAN_POINT('Ctrl Pts',(-2.68942924946335,1.75380081078585,
1.22755163642413));
#103764=CARTESIAN_POINT('Ctrl Pts',(-0.62204903688223,3.42210546244733,
1.10079342834945));
#103765=CARTESIAN_POINT('Ctrl Pts',(2.53961703903404,2.37666649300172,0.941901492865588));
#103766=CARTESIAN_POINT('Ctrl Pts',(3.37339857704762,-0.847434397963935,
0.783009557381711));
#103767=CARTESIAN_POINT('Ctrl Pts',(1.11513000686983,-3.29443532088267,
0.624117621897844));
#103768=CARTESIAN_POINT('Ctrl Pts',(-2.05637049788623,-2.7413454552293,
0.470506475133804));
#103769=CARTESIAN_POINT('Ctrl Pts',(-2.93964728609037,-0.876412749831535,
0.369859306864387));
#103770=CARTESIAN_POINT('Ctrl Pts',(-2.94561598299575,0.00187102060485729,
0.322176117089595));
#103771=CARTESIAN_POINT('Origin',(0.,0.,-1.84858989190503));
#103772=CARTESIAN_POINT('',(-2.37174933328259,-0.00177836262041549,23.651410108095));
#103773=CARTESIAN_POINT('Ctrl Pts',(-2.36542649498009,0.173076744094118,
23.6397760267629));
#103774=CARTESIAN_POINT('Ctrl Pts',(-2.36967824820991,0.114968361061076,
23.6440297226054));
#103775=CARTESIAN_POINT('Ctrl Pts',(-2.37179115015004,0.0566713851742079,
23.6482936118239));
#103776=CARTESIAN_POINT('Ctrl Pts',(-2.37174939305784,-0.00169677038972837,
23.6525333695376));
#103777=CARTESIAN_POINT('',(-2.34668236863856,0.3439184833953,24.62825));
#103778=CARTESIAN_POINT('Ctrl Pts',(-2.37174933328259,-0.0017783626204155,
23.651410108095));
#103779=CARTESIAN_POINT('Ctrl Pts',(-2.37166213645339,-0.118070180242878,
23.6592395344289));
#103780=CARTESIAN_POINT('Ctrl Pts',(-2.3630207288615,-0.234043937961113,
23.6670689607629));
#103781=CARTESIAN_POINT('Ctrl Pts',(-2.34597095750765,-0.348738195543054,
23.6748983870969));
#103782=CARTESIAN_POINT('Ctrl Pts',(-2.33435655987608,-0.426868552013454,
23.6802318351991));
#103783=CARTESIAN_POINT('Ctrl Pts',(-2.3188129279233,-0.504565287258719,
23.6855652833013));
#103784=CARTESIAN_POINT('Ctrl Pts',(-2.29938446161523,-0.581402752128369,
23.6908987314035));
#103785=CARTESIAN_POINT('Ctrl Pts',(-2.27998401512876,-0.658129401660169,
23.6962244875828));
#103786=CARTESIAN_POINT('Ctrl Pts',(-2.2567099746355,-0.733998791410123,
23.7015502437621));
#103787=CARTESIAN_POINT('Ctrl Pts',(-2.22965819359468,-0.808592853193823,
23.7068759999414));
#103788=CARTESIAN_POINT('Ctrl Pts',(-2.20263780793542,-0.883100343633887,
23.7121955752284));
#103789=CARTESIAN_POINT('Ctrl Pts',(-2.17184855336974,-0.956335009257643,
23.7175151505153));
#103790=CARTESIAN_POINT('Ctrl Pts',(-2.13743638304207,-1.02789287912119,
23.7228347258023));
#103791=CARTESIAN_POINT('Ctrl Pts',(-2.10304607897219,-1.09940527952392,
23.7281509209128));
#103792=CARTESIAN_POINT('Ctrl Pts',(-2.06503763097987,-1.16924257789309,
23.7334671160234));
#103793=CARTESIAN_POINT('Ctrl Pts',(-2.02360503864635,-1.23702090122403,
23.738783311134));
#103794=CARTESIAN_POINT('Ctrl Pts',(-1.98218588602492,-1.30477723893687,
23.7440977818019));
#103795=CARTESIAN_POINT('Ctrl Pts',(-1.9373450388303,-1.37047552841582,
23.7494122524697));
#103796=CARTESIAN_POINT('Ctrl Pts',(-1.88932163343825,-1.43375793909649,
23.7547267231376));
#103797=CARTESIAN_POINT('Ctrl Pts',(-1.84129886847173,-1.49703950586218,
23.7600411229333));
#103798=CARTESIAN_POINT('Ctrl Pts',(-1.79009391396709,-1.5579048854719,
23.765355522729));
#103799=CARTESIAN_POINT('Ctrl Pts',(-1.7359873831785,-1.61602780543685,
23.7706699225247));
#103800=CARTESIAN_POINT('Ctrl Pts',(-1.68182686780958,-1.6742087173188,
23.7759896247421));
#103801=CARTESIAN_POINT('Ctrl Pts',(-1.62475931293704,-1.72964135975047,
23.7813093269595));
#103802=CARTESIAN_POINT('Ctrl Pts',(-1.56510314122222,-1.78203541486591,
23.7866290291769));
#103803=CARTESIAN_POINT('Ctrl Pts',(-1.50541836579805,-1.83445459167927,
23.7919512820645));
#103804=CARTESIAN_POINT('Ctrl Pts',(-1.44314286848062,-1.88383198720657,
23.797273534952));
#103805=CARTESIAN_POINT('Ctrl Pts',(-1.37862719154216,-1.92991842554047,
23.8025957878396));
#103806=CARTESIAN_POINT('Ctrl Pts',(-1.3139940832985,-1.97608875031657,
23.8079277282811));
#103807=CARTESIAN_POINT('Ctrl Pts',(-1.24711304291611,-2.01895589452395,
23.8132596687226));
#103808=CARTESIAN_POINT('Ctrl Pts',(-1.17836238220007,-2.05831488327607,
23.8185916091642));
#103809=CARTESIAN_POINT('Ctrl Pts',(-1.11303772220215,-2.09571252471422,
23.8236578469697));
#103810=CARTESIAN_POINT('Ctrl Pts',(-1.04602564777549,-2.12994316111438,
23.8287240847752));
#103811=CARTESIAN_POINT('Ctrl Pts',(-0.977666994686801,-2.1608714237548,
23.8337903225807));
#103812=CARTESIAN_POINT('Ctrl Pts',(-0.905825097966649,-2.19337564889603,
23.839114712643));
#103813=CARTESIAN_POINT('Ctrl Pts',(-0.832222031729365,-2.22235580829395,
23.8444391027054));
#103814=CARTESIAN_POINT('Ctrl Pts',(-0.757238117187071,-2.24761840541916,
23.8497634927677));
#103815=CARTESIAN_POINT('Ctrl Pts',(-0.682363045020286,-2.27284433279861,
23.855080154249));
#103816=CARTESIAN_POINT('Ctrl Pts',(-0.606111546422999,-2.29436326425291,
23.8603968157303));
#103817=CARTESIAN_POINT('Ctrl Pts',(-0.528885553033947,-2.31202900809916,
23.8657134772116));
#103818=CARTESIAN_POINT('Ctrl Pts',(-0.451749529117852,-2.32967417108145,
23.8710239447003));
#103819=CARTESIAN_POINT('Ctrl Pts',(-0.373641722320833,-2.34347496198871,
23.876334412189));
#103820=CARTESIAN_POINT('Ctrl Pts',(-0.294979449900713,-2.35333490745288,
23.8816448796777));
#103821=CARTESIAN_POINT('Ctrl Pts',(-0.216367310215482,-2.36318856901479,
23.8869519627198));
#103822=CARTESIAN_POINT('Ctrl Pts',(-0.137201871580469,-2.36910631132213,
23.8922590457619));
#103823=CARTESIAN_POINT('Ctrl Pts',(-0.0579096591383827,-2.37104292113797,
23.897566128804));
#103824=CARTESIAN_POINT('Ctrl Pts',(0.021356906466357,-2.37297890456295,
23.9028714952855));
#103825=CARTESIAN_POINT('Ctrl Pts',(0.100749694667562,-2.37093630073283,
23.9081768617669));
#103826=CARTESIAN_POINT('Ctrl Pts',(0.179839568219446,-2.36492194209505,
23.9134822282483));
#103827=CARTESIAN_POINT('Ctrl Pts',(0.258928683893683,-2.35890764108979,
23.9187875438911));
#103828=CARTESIAN_POINT('Ctrl Pts',(0.337714421852944,-2.34892169793918,
23.9240928595339));
#103829=CARTESIAN_POINT('Ctrl Pts',(0.415771675756215,-2.33502290698376,
23.9293981751768));
#103830=CARTESIAN_POINT('Ctrl Pts',(0.493908338240533,-2.32110997662152,
23.9347088879808));
#103831=CARTESIAN_POINT('Ctrl Pts',(0.571314572142124,-2.30327632954018,
23.9400196007849));
#103832=CARTESIAN_POINT('Ctrl Pts',(0.64757499476761,-2.28163202305975,
23.945330313589));
#103833=CARTESIAN_POINT('Ctrl Pts',(0.723872570910351,-2.25997717163232,
23.9506436137333));
#103834=CARTESIAN_POINT('Ctrl Pts',(0.799022777893084,-2.23450811410081,
23.9559569138776));
#103835=CARTESIAN_POINT('Ctrl Pts',(0.872627438099414,-2.20538418802168,
23.9612702140219));
#103836=CARTESIAN_POINT('Ctrl Pts',(0.946368638599109,-2.17620623561596,
23.9665933706014));
#103837=CARTESIAN_POINT('Ctrl Pts',(1.01855813423093,-2.14336006233295,
23.9719165271809));
#103838=CARTESIAN_POINT('Ctrl Pts',(1.08881987715376,-2.10705228639796,
23.9772396837603));
#103839=CARTESIAN_POINT('Ctrl Pts',(1.15676340963184,-2.0719424463794,23.9823872085284));
#103840=CARTESIAN_POINT('Ctrl Pts',(1.22290412114906,-2.03359613277576,
23.9875347332965));
#103841=CARTESIAN_POINT('Ctrl Pts',(1.28692882879557,-1.9922380008711,23.9926822580646));
#103842=CARTESIAN_POINT('Ctrl Pts',(1.35337617358078,-1.94931491459144,
23.9980245605229));
#103843=CARTESIAN_POINT('Ctrl Pts',(1.41779753409028,-1.90298390981766,
24.0033668629812));
#103844=CARTESIAN_POINT('Ctrl Pts',(1.47982291798039,-1.85346221809887,
24.0087091654396));
#103845=CARTESIAN_POINT('Ctrl Pts',(1.54175842012147,-1.80401228887453,
24.0140437263015));
#103846=CARTESIAN_POINT('Ctrl Pts',(1.60130447951582,-1.75138114452795,
24.0193782871635));
#103847=CARTESIAN_POINT('Ctrl Pts',(1.65811931244879,-1.69582971084492,
24.0247128480254));
#103848=CARTESIAN_POINT('Ctrl Pts',(1.71486708816156,-1.64034384322146,
24.0300411126298));
#103849=CARTESIAN_POINT('Ctrl Pts',(1.76888971219997,-1.58194486139646,
24.0353693772341));
#103850=CARTESIAN_POINT('Ctrl Pts',(1.81987897285177,-1.52093345898891,
24.0406976418385));
#103851=CARTESIAN_POINT('Ctrl Pts',(1.87083517715617,-1.45996161028518,
24.0460224521279));
#103852=CARTESIAN_POINT('Ctrl Pts',(1.9187616232362,-1.39638106028224,24.0513472624173));
#103853=CARTESIAN_POINT('Ctrl Pts',(1.9633882594744,-1.33052794223123,24.0566720727067));
#103854=CARTESIAN_POINT('Ctrl Pts',(2.00799972638391,-1.2646972087397,24.0619950730054));
#103855=CARTESIAN_POINT('Ctrl Pts',(2.04931334932713,-1.19659582750647,
24.067318073304));
#103856=CARTESIAN_POINT('Ctrl Pts',(2.08710143426901,-1.1265902829211,24.0726410736027));
#103857=CARTESIAN_POINT('Ctrl Pts',(2.12488832724072,-1.0565869465588,24.0779639059951));
#103858=CARTESIAN_POINT('Ctrl Pts',(2.15914968262113,-0.984679977673584,
24.0832867383875));
#103859=CARTESIAN_POINT('Ctrl Pts',(2.18970366579744,-0.911260620510532,
24.0886095707798));
#103860=CARTESIAN_POINT('Ctrl Pts',(2.22028687598047,-0.837771032633785,
24.093937494831));
#103861=CARTESIAN_POINT('Ctrl Pts',(2.24715544940571,-0.762766598356138,
24.0992654188823));
#103862=CARTESIAN_POINT('Ctrl Pts',(2.2701759021778,-0.68665816508012,24.1045933429335));
#103863=CARTESIAN_POINT('Ctrl Pts',(2.29320693481568,-0.61051475347345,
24.1099237156212));
#103864=CARTESIAN_POINT('Ctrl Pts',(2.31238620985614,-0.533266785567809,
24.1152540883089));
#103865=CARTESIAN_POINT('Ctrl Pts',(2.32763095878448,-0.455337437740462,
24.1205844609966));
#103866=CARTESIAN_POINT('Ctrl Pts',(2.34290264706581,-0.377270379136774,
24.1259242531108));
#103867=CARTESIAN_POINT('Ctrl Pts',(2.35422584846339,-0.298519997801786,
24.131264045225));
#103868=CARTESIAN_POINT('Ctrl Pts',(2.36156950805721,-0.219516562278207,
24.1366038373392));
#103869=CARTESIAN_POINT('Ctrl Pts',(2.36843227210291,-0.145686623693552,
24.1415939560756));
#103870=CARTESIAN_POINT('Ctrl Pts',(2.37182013699591,-0.071636038038402,
24.146584074812));
#103871=CARTESIAN_POINT('Ctrl Pts',(2.37174889865758,0.00228565451689994,
24.1515741935483));
#103872=CARTESIAN_POINT('Ctrl Pts',(2.37167267487504,0.0813805793809012,
24.1569135337727));
#103873=CARTESIAN_POINT('Ctrl Pts',(2.36763542177374,0.160617032165804,
24.1622528739972));
#103874=CARTESIAN_POINT('Ctrl Pts',(2.35961988042824,0.239566446706986,
24.1675922142216));
#103875=CARTESIAN_POINT('Ctrl Pts',(2.35161572251256,0.318403739673224,
24.1729239716762));
#103876=CARTESIAN_POINT('Ctrl Pts',(2.33964454414398,0.396954342918136,
24.1782557291308));
#103877=CARTESIAN_POINT('Ctrl Pts',(2.32374109811239,0.474789818175803,
24.1835874865854));
#103878=CARTESIAN_POINT('Ctrl Pts',(2.3078556896909,0.552537012821109,24.188913196787));
#103879=CARTESIAN_POINT('Ctrl Pts',(2.2880469701543,0.629570235907194,24.1942389069886));
#103880=CARTESIAN_POINT('Ctrl Pts',(2.26440130128787,0.705467794605676,
24.1995646171902));
#103881=CARTESIAN_POINT('Ctrl Pts',(2.24077029356514,0.781318294156822,
24.2048870252648));
#103882=CARTESIAN_POINT('Ctrl Pts',(2.21330719763369,0.856034082161029,
24.2102094333393));
#103883=CARTESIAN_POINT('Ctrl Pts',(2.18214881653151,0.929206438317201,
24.2155318414139));
#103884=CARTESIAN_POINT('Ctrl Pts',(2.15100012968629,1.00235602847599,24.2208525935362));
#103885=CARTESIAN_POINT('Ctrl Pts',(2.11615862383116,1.07396271088252,24.2261733456585));
#103886=CARTESIAN_POINT('Ctrl Pts',(2.07780952519887,1.14363702261376,24.2314940977808));
#103887=CARTESIAN_POINT('Ctrl Pts',(2.03946051212473,1.21331117889921,24.2368148380323));
#103888=CARTESIAN_POINT('Ctrl Pts',(1.99760414835687,1.2810525644594,24.2421355782838));
#103889=CARTESIAN_POINT('Ctrl Pts',(1.95247126540384,1.34649694402635,24.2474563185353));
#103890=CARTESIAN_POINT('Ctrl Pts',(1.90729301366787,1.41200711003676,24.2527824073375));
#103891=CARTESIAN_POINT('Ctrl Pts',(1.85883192928299,1.47521527208597,24.2581084961396));
#103892=CARTESIAN_POINT('Ctrl Pts',(1.80736146548855,1.53578728851592,24.2634345849418));
#103893=CARTESIAN_POINT('Ctrl Pts',(1.75586601055456,1.59638871528344,24.2687632597907));
#103894=CARTESIAN_POINT('Ctrl Pts',(1.70135858561781,1.65435110556944,24.2740919346397));
#103895=CARTESIAN_POINT('Ctrl Pts',(1.64415039897993,1.70937635646283,24.2794206094887));
#103896=CARTESIAN_POINT('Ctrl Pts',(1.58683840100284,1.76450145748819,24.284758953878));
#103897=CARTESIAN_POINT('Ctrl Pts',(1.52681620164722,1.81667846148374,24.2900972982674));
#103898=CARTESIAN_POINT('Ctrl Pts',(1.46442891020077,1.86564895665508,24.2954356426568));
#103899=CARTESIAN_POINT('Ctrl Pts',(1.40587696564674,1.91160892144241,24.3004458047819));
#103900=CARTESIAN_POINT('Ctrl Pts',(1.34524234866685,1.95474472685475,24.3054559669071));
#103901=CARTESIAN_POINT('Ctrl Pts',(1.28283147795962,1.99487880876406,24.3104661290322));
#103902=CARTESIAN_POINT('Ctrl Pts',(1.21713308801171,2.03712697056025,24.3157402035848));
#103903=CARTESIAN_POINT('Ctrl Pts',(1.14920531743009,2.07621601382973,24.3210142781374));
#103904=CARTESIAN_POINT('Ctrl Pts',(1.07938820249835,2.1118994225122,24.32628835269));
#103905=CARTESIAN_POINT('Ctrl Pts',(1.00967364853039,2.14753041246055,24.3315546796556));
#103906=CARTESIAN_POINT('Ctrl Pts',(0.938075681216748,2.17976548001854,
24.3368210066212));
#103907=CARTESIAN_POINT('Ctrl Pts',(0.864963090391752,2.20840143876967,
24.3420873335868));
#103908=CARTESIAN_POINT('Ctrl Pts',(0.791342100728035,2.23723652174838,
24.3473902807089));
#103909=CARTESIAN_POINT('Ctrl Pts',(0.716185750227005,2.26242197002789,
24.3526932278309));
#103910=CARTESIAN_POINT('Ctrl Pts',(0.639895415943316,2.28379769663487,
24.357996174953));
#103911=CARTESIAN_POINT('Ctrl Pts',(0.564265586288636,2.30498835698798,
24.3632532103465));
#103912=CARTESIAN_POINT('Ctrl Pts',(0.48752180228139,2.32243487533405,24.3685102457399));
#103913=CARTESIAN_POINT('Ctrl Pts',(0.410072754950791,2.33603047885662,
24.3737672811334));
#103914=CARTESIAN_POINT('Ctrl Pts',(0.332646181205444,2.34962213730865,
24.3790227910797));
#103915=CARTESIAN_POINT('Ctrl Pts',(0.254515222474931,2.35936501513378,
24.3842783010259));
#103916=CARTESIAN_POINT('Ctrl Pts',(0.176098874936079,2.365203426504,24.3895338109722));
#103917=CARTESIAN_POINT('Ctrl Pts',(0.0976795929290665,2.37104205635714,
24.3947895175882));
#103918=CARTESIAN_POINT('Ctrl Pts',(0.0189753795552956,2.37297589548929,
24.4000452242043));
#103919=CARTESIAN_POINT('Ctrl Pts',(-0.0595911775780031,2.3710012555996,
24.4053009308204));
#103920=CARTESIAN_POINT('Ctrl Pts',(-0.139389335116919,2.36899566147979,
24.410639025295));
#103921=CARTESIAN_POINT('Ctrl Pts',(-0.21904497246151,2.36295799177357,
24.4159771197697));
#103922=CARTESIAN_POINT('Ctrl Pts',(-0.298119195240333,2.35293922741945,
24.4213152142443));
#103923=CARTESIAN_POINT('Ctrl Pts',(-0.376107035853347,2.34305810851458,
24.4265799698933));
#103924=CARTESIAN_POINT('Ctrl Pts',(-0.453528874794992,2.32930476836392,
24.4318447255424));
#103925=CARTESIAN_POINT('Ctrl Pts',(-0.529974611026111,2.31177961193703,
24.4371094811914));
#103926=CARTESIAN_POINT('Ctrl Pts',(-0.608017697892443,2.29388826347471,
24.4424842450788));
#103927=CARTESIAN_POINT('Ctrl Pts',(-0.685042921119731,2.27206584119297,
24.4478590089663));
#103928=CARTESIAN_POINT('Ctrl Pts',(-0.760633074143077,2.24647176457209,
24.4532337728538));
#103929=CARTESIAN_POINT('Ctrl Pts',(-0.836223227166402,2.22087768795122,
24.4586085367413));
#103930=CARTESIAN_POINT('Ctrl Pts',(-0.910377856403356,2.19151222800949,
24.4639833006288));
#103931=CARTESIAN_POINT('Ctrl Pts',(-0.982706159455222,2.15858441268086,
24.4693580645162));
#103932=CARTESIAN_POINT('Ctrl Pts',(-1.05647039700162,2.12500288111855,
24.4748395336427));
#103933=CARTESIAN_POINT('Ctrl Pts',(-1.12862529498818,2.08758455147576,
24.4803210027692));
#103934=CARTESIAN_POINT('Ctrl Pts',(-1.19875810291352,2.04650362159444,
24.4858024718957));
#103935=CARTESIAN_POINT('Ctrl Pts',(-1.26877844878286,2.00548856738492,
24.4912751511662));
#103936=CARTESIAN_POINT('Ctrl Pts',(-1.33678277824863,1.96082281185819,
24.4967478304366));
#103937=CARTESIAN_POINT('Ctrl Pts',(-1.40238062809185,1.91272753847815,
24.502220509707));
#103938=CARTESIAN_POINT('Ctrl Pts',(-1.46787345789692,1.86470926407687,
24.5076844273948));
#103939=CARTESIAN_POINT('Ctrl Pts',(-1.53096712723125,1.81327265922936,
24.5131483450825));
#103940=CARTESIAN_POINT('Ctrl Pts',(-1.59129919398357,1.75868272798912,
24.5186122627702));
#103941=CARTESIAN_POINT('Ctrl Pts',(-1.65157432175483,1.7041443165331,24.5240710238319));
#103942=CARTESIAN_POINT('Ctrl Pts',(-1.70909270619569,1.64645878773391,
24.5295297848937));
#103943=CARTESIAN_POINT('Ctrl Pts',(-1.76352453575373,1.58593167390484,
24.5349885459554));
#103944=CARTESIAN_POINT('Ctrl Pts',(-1.81791838836082,1.52544678969126,
24.5404434984532));
#103945=CARTESIAN_POINT('Ctrl Pts',(-1.86922967744731,1.46212458763374,
24.545898450951));
#103946=CARTESIAN_POINT('Ctrl Pts',(-1.91716584794229,1.39630697698741,
24.5513534034488));
#103947=CARTESIAN_POINT('Ctrl Pts',(-1.96508035726408,1.33051910769606,
24.5568058909881));
#103948=CARTESIAN_POINT('Ctrl Pts',(-2.00962252561581,1.26223842631984,
24.5622583785274));
#103949=CARTESIAN_POINT('Ctrl Pts',(-2.05054114082474,1.19183853448577,
24.5677108660667));
#103950=CARTESIAN_POINT('Ctrl Pts',(-2.09146309494411,1.12143289810406,
24.5731637985225));
#103951=CARTESIAN_POINT('Ctrl Pts',(-2.12876067700963,1.0489080787843,24.5786167309784));
#103952=CARTESIAN_POINT('Ctrl Pts',(-2.16222733168544,0.97466457235936,
24.5840696634342));
#103953=CARTESIAN_POINT('Ctrl Pts',(-2.19569368267863,0.900421739633752,
24.5895225464091));
#103954=CARTESIAN_POINT('Ctrl Pts',(-2.22532900145471,0.824460652069974,
24.594975429384));
#103955=CARTESIAN_POINT('Ctrl Pts',(-2.25097447102949,0.747202779219605,
24.6004283123589));
#103956=CARTESIAN_POINT('Ctrl Pts',(-2.27663814439174,0.669890066823669,
24.6058850659247));
#103957=CARTESIAN_POINT('Ctrl Pts',(-2.29830617760441,0.591279147240244,
24.6113418194906));
#103958=CARTESIAN_POINT('Ctrl Pts',(-2.31586947221595,0.511807239259295,
24.6167985730565));
#103959=CARTESIAN_POINT('Ctrl Pts',(-2.32815545768968,0.456214554138488,
24.620615715371));
#103960=CARTESIAN_POINT('Ctrl Pts',(-2.33843389221547,0.4002008733358,24.6244328576855));
#103961=CARTESIAN_POINT('Ctrl Pts',(-2.34668236863855,0.343918483395331,
24.62825));
#103962=CARTESIAN_POINT('',(-0.439445221994668,2.33068358199179,24.62825));
#103963=CARTESIAN_POINT('Origin',(0.,0.,24.62825));
#103964=CARTESIAN_POINT('',(-2.37174962922866,0.00132618012251302,23.848589891949));
#103965=CARTESIAN_POINT('Ctrl Pts',(-2.37174962922866,0.00132618012251301,
23.848589891949));
#103966=CARTESIAN_POINT('Ctrl Pts',(-2.37179321578096,-0.0766243090381988,
23.8538460302553));
#103967=CARTESIAN_POINT('Ctrl Pts',(-2.36798967073156,-0.154732553614779,
23.8591021685616));
#103968=CARTESIAN_POINT('Ctrl Pts',(-2.36031867986084,-0.232580721471071,
23.8643583068678));
#103969=CARTESIAN_POINT('Ctrl Pts',(-2.35253306808389,-0.311592106400268,
23.8696929830509));
#103970=CARTESIAN_POINT('Ctrl Pts',(-2.34076339777506,-0.390335080010402,
23.8750276592339));
#103971=CARTESIAN_POINT('Ctrl Pts',(-2.32504340342227,-0.468370830328489,
23.880362335417));
#103972=CARTESIAN_POINT('Ctrl Pts',(-2.30959037090728,-0.545081353241827,
23.8856064164684));
#103973=CARTESIAN_POINT('Ctrl Pts',(-2.29032023401202,-0.621107992227486,
23.8908504975198));
#103974=CARTESIAN_POINT('Ctrl Pts',(-2.26731719654381,-0.69603936149957,
23.8960945785712));
#103975=CARTESIAN_POINT('Ctrl Pts',(-2.2443252230489,-0.770934690371743,
23.9013361373308));
#103976=CARTESIAN_POINT('Ctrl Pts',(-2.21760405191751,-0.844735333714892,
23.9065776960904));
#103977=CARTESIAN_POINT('Ctrl Pts',(-2.18728829509854,-0.917043061488905,
23.91181925485));
#103978=CARTESIAN_POINT('Ctrl Pts',(-2.15697706859641,-0.989339983762697,
23.9170600303231));
#103979=CARTESIAN_POINT('Ctrl Pts',(-2.1230725101674,-1.0601439884811,23.9223008057963));
#103980=CARTESIAN_POINT('Ctrl Pts',(-2.08575750639758,-1.12907647526912,
23.9275415812694));
#103981=CARTESIAN_POINT('Ctrl Pts',(-2.04727975669769,-1.2001569175808,
23.9329456607687));
#103982=CARTESIAN_POINT('Ctrl Pts',(-2.00517572827963,-1.26924678139352,
23.938349740268));
#103983=CARTESIAN_POINT('Ctrl Pts',(-1.95969619098761,-1.33595991763549,
23.9437538197673));
#103984=CARTESIAN_POINT('Ctrl Pts',(-1.91553321992236,-1.40074180595176,
23.9490014590524));
#103985=CARTESIAN_POINT('Ctrl Pts',(-1.86818787072067,-1.46328234982385,
23.9542490983375));
#103986=CARTESIAN_POINT('Ctrl Pts',(-1.81793154408544,-1.5232606354525,
23.9594967376227));
#103987=CARTESIAN_POINT('Ctrl Pts',(-1.76542788963009,-1.58592098877134,
23.964979037229));
#103988=CARTESIAN_POINT('Ctrl Pts',(-1.70974721301348,-1.64578411662999,
23.9704613368355));
#103989=CARTESIAN_POINT('Ctrl Pts',(-1.65124101992624,-1.70252787249224,
23.9759436364419));
#103990=CARTESIAN_POINT('Ctrl Pts',(-1.59273482683902,-1.75927162835447,
23.9814259360483));
#103991=CARTESIAN_POINT('Ctrl Pts',(-1.53140361733028,-1.81289568600277,
23.9869082356546));
#103992=CARTESIAN_POINT('Ctrl Pts',(-1.46763483942312,-1.86312802582417,
23.992390535261));
#103993=CARTESIAN_POINT('Ctrl Pts',(-1.40549780860171,-1.91207499564471,
23.9977325510687));
#103994=CARTESIAN_POINT('Ctrl Pts',(-1.34079355743106,-1.95800139835332,
24.0030745668764));
#103995=CARTESIAN_POINT('Ctrl Pts',(-1.27384742898195,-2.00062759907387,
24.008416582684));
#103996=CARTESIAN_POINT('Ctrl Pts',(-1.20699840183584,-2.04319197307303,
24.0137508502214));
#103997=CARTESIAN_POINT('Ctrl Pts',(-1.1379143461198,-2.08246540313572,
24.0190851177588));
#103998=CARTESIAN_POINT('Ctrl Pts',(-1.06695280520039,-2.11820909590508,
24.0244193852962));
#103999=CARTESIAN_POINT('Ctrl Pts',(-0.9960751231509,-2.15391054853079,
24.0297473490578));
#104000=CARTESIAN_POINT('Ctrl Pts',(-0.923324780467033,-2.186090345244,
24.0350753128194));
#104001=CARTESIAN_POINT('Ctrl Pts',(-0.849086067784299,-2.21455433710591,
24.0404032765809));
#104002=CARTESIAN_POINT('Ctrl Pts',(-0.774895554277249,-2.2429998488394,
24.0457277811842));
#104003=CARTESIAN_POINT('Ctrl Pts',(-0.699219023791896,-2.26773417796237,
24.0510522857874));
#104004=CARTESIAN_POINT('Ctrl Pts',(-0.622461932851828,-2.28861075865914,
24.0563767903906));
#104005=CARTESIAN_POINT('Ctrl Pts',(-0.545730997554536,-2.30948022548043,
24.0616994806228));
#104006=CARTESIAN_POINT('Ctrl Pts',(-0.467920683258017,-2.32649443208219,
24.0670221708551));
#104007=CARTESIAN_POINT('Ctrl Pts',(-0.389451437705792,-2.33955671873304,
24.0723448610873));
#104008=CARTESIAN_POINT('Ctrl Pts',(-0.310984725306586,-2.35261858370567,
24.0776673794919));
#104009=CARTESIAN_POINT('Ctrl Pts',(-0.231859584730243,-2.36172870688726,
24.0829898978964));
#104010=CARTESIAN_POINT('Ctrl Pts',(-0.152505029891621,-2.36684183636291,
24.0883124163009));
#104011=CARTESIAN_POINT('Ctrl Pts',(-0.0730745180504347,-2.37195986005023,
24.0936400293411));
#104012=CARTESIAN_POINT('Ctrl Pts',(0.00658537969246999,-2.37307321674422,
24.0989676423813));
#104013=CARTESIAN_POINT('Ctrl Pts',(0.0860427682642641,-2.37018874871379,
24.1042952554215));
#104014=CARTESIAN_POINT('Ctrl Pts',(0.165536632852462,-2.36730295652829,
24.1096253141764));
#104015=CARTESIAN_POINT('Ctrl Pts',(0.244827337132171,-2.36041572285409,
24.1149553729312));
#104016=CARTESIAN_POINT('Ctrl Pts',(0.323487755211197,-2.34958586451494,
24.1202854316861));
#104017=CARTESIAN_POINT('Ctrl Pts',(0.402287444608774,-2.33873683149191,
24.1256249275166));
#104018=CARTESIAN_POINT('Ctrl Pts',(0.480454157696104,-2.32393131117814,
24.130964423347));
#104019=CARTESIAN_POINT('Ctrl Pts',(0.557570811734681,-2.30527934368083,
24.1363039191774));
#104020=CARTESIAN_POINT('Ctrl Pts',(0.630032081969307,-2.28775335951983,
24.1413210799336));
#104021=CARTESIAN_POINT('Ctrl Pts',(0.701566063359796,-2.26683188662173,
24.1463382406897));
#104022=CARTESIAN_POINT('Ctrl Pts',(0.771841893365145,-2.24264534738476,
24.1513554014458));
#104023=CARTESIAN_POINT('Ctrl Pts',(0.846625670762385,-2.21690732670013,
24.1566943954232));
#104024=CARTESIAN_POINT('Ctrl Pts',(0.920258278935062,-2.18737722550626,
24.1620333894005));
#104025=CARTESIAN_POINT('Ctrl Pts',(0.992328779471983,-2.15417772152895,
24.1673723833779));
#104026=CARTESIAN_POINT('Ctrl Pts',(1.06429683066958,-2.12102541116376,
24.1727037878921));
#104027=CARTESIAN_POINT('Ctrl Pts',(1.13470676339634,-2.08421425145252,
24.1780351924064));
#104028=CARTESIAN_POINT('Ctrl Pts',(1.20316463057147,-2.04391607808193,
24.1833665969206));
#104029=CARTESIAN_POINT('Ctrl Pts',(1.27154475530295,-2.00366366831167,
24.1886919469603));
#104030=CARTESIAN_POINT('Ctrl Pts',(1.3379768193361,-1.9599323504935,24.194017297));
#104031=CARTESIAN_POINT('Ctrl Pts',(1.40208999717757,-1.91294059037771,
24.1993426470397));
#104032=CARTESIAN_POINT('Ctrl Pts',(1.46616336362737,-1.86597801002542,
24.2046646902772));
#104033=CARTESIAN_POINT('Ctrl Pts',(1.52792032624963,-1.81575928178115,
24.2099867335147));
#104034=CARTESIAN_POINT('Ctrl Pts',(1.58701869317772,-1.76254637669609,
24.2153087767522));
#104035=CARTESIAN_POINT('Ctrl Pts',(1.64609862573789,-1.70935007014531,
24.2206291599015));
#104036=CARTESIAN_POINT('Ctrl Pts',(1.70252126248582,-1.653161753986,24.2259495430508));
#104037=CARTESIAN_POINT('Ctrl Pts',(1.75597833633348,-1.59428295632473,
24.2312699262001));
#104038=CARTESIAN_POINT('Ctrl Pts',(1.80943525472935,-1.53540432988147,
24.2365902938778));
#104039=CARTESIAN_POINT('Ctrl Pts',(1.85992631430492,-1.47383558439784,
24.2419106615556));
#104040=CARTESIAN_POINT('Ctrl Pts',(1.90718190670332,-1.40991320202468,
24.2472310292333));
#104041=CARTESIAN_POINT('Ctrl Pts',(1.95448504064441,-1.34592651046575,
24.252556749473));
#104042=CARTESIAN_POINT('Ctrl Pts',(1.99854592669908,-1.27958182858898,
24.2578824697128));
#104043=CARTESIAN_POINT('Ctrl Pts',(2.03913724985554,-1.21124619246113,
24.2632081899525));
#104044=CARTESIAN_POINT('Ctrl Pts',(2.07974826398607,-1.14287740650878,
24.2685364937153));
#104045=CARTESIAN_POINT('Ctrl Pts',(2.1168861436007,-1.07251615593724,24.2738647974781));
#104046=CARTESIAN_POINT('Ctrl Pts',(2.15036991320664,-1.00055349625878,
24.2791931012408));
#104047=CARTESIAN_POINT('Ctrl Pts',(2.18391456865124,-0.928459981932298,
24.2845310938244));
#104048=CARTESIAN_POINT('Ctrl Pts',(2.21379166050636,-0.85475967381021,
24.289869086408));
#104049=CARTESIAN_POINT('Ctrl Pts',(2.23986875603263,-0.779862820147777,
24.2952070789915));
#104050=CARTESIAN_POINT('Ctrl Pts',(2.26447901027324,-0.709178927894634,
24.3002448085379));
#104051=CARTESIAN_POINT('Ctrl Pts',(2.28570510192159,-0.637429778567851,
24.3052825380843));
#104052=CARTESIAN_POINT('Ctrl Pts',(2.30347747792983,-0.564968646183165,
24.3103202676306));
#104053=CARTESIAN_POINT('Ctrl Pts',(2.32208249405447,-0.489112692212707,
24.3155940160252));
#104054=CARTESIAN_POINT('Ctrl Pts',(2.33697600536397,-0.412174836926209,
24.3208677644198));
#104055=CARTESIAN_POINT('Ctrl Pts',(2.34803532246676,-0.334556702142403,
24.3261415128144));
#104056=CARTESIAN_POINT('Ctrl Pts',(2.35907837887199,-0.257052690590922,
24.3314075071292));
#104057=CARTESIAN_POINT('Ctrl Pts',(2.36629836182808,-0.178870854899216,
24.336673501444));
#104058=CARTESIAN_POINT('Ctrl Pts',(2.36962290107848,-0.10042593880272,
24.3419394957588));
#104059=CARTESIAN_POINT('Ctrl Pts',(2.37297273989634,-0.0213840610531468,
24.3472455640111));
#104060=CARTESIAN_POINT('Ctrl Pts',(2.37236746320867,0.0579244408043494,
24.3525516322635));
#104061=CARTESIAN_POINT('Ctrl Pts',(2.36778602442185,0.137067155265542,
24.3578577005158));
#104062=CARTESIAN_POINT('Ctrl Pts',(2.36324722143088,0.215473351620838,
24.363114389424));
#104063=CARTESIAN_POINT('Ctrl Pts',(2.35480598256657,0.293716345200748,
24.3683710783321));
#104064=CARTESIAN_POINT('Ctrl Pts',(2.34249411781659,0.371374972897555,
24.3736277672403));
#104065=CARTESIAN_POINT('Ctrl Pts',(2.33018583400637,0.449011013368738,
24.378882927226));
#104066=CARTESIAN_POINT('Ctrl Pts',(2.31400923306241,0.526062551519991,
24.3841380872117));
#104067=CARTESIAN_POINT('Ctrl Pts',(2.29404778847505,0.602115276913609,
24.3893932471974));
#104068=CARTESIAN_POINT('Ctrl Pts',(2.27408560879438,0.678170802998758,
24.3946486007078));
#104069=CARTESIAN_POINT('Ctrl Pts',(2.25033843198666,0.753226979464458,
24.3999039542182));
#104070=CARTESIAN_POINT('Ctrl Pts',(2.22294007465867,0.826882994731737,
24.4051593077287));
#104071=CARTESIAN_POINT('Ctrl Pts',(2.19508051054008,0.901778889237123,
24.4105031265692));
#104072=CARTESIAN_POINT('Ctrl Pts',(2.16344587286729,0.975226562332597,
24.4158469454098));
#104073=CARTESIAN_POINT('Ctrl Pts',(2.12822766055512,1.04682619729737,24.4211907642503));
#104074=CARTESIAN_POINT('Ctrl Pts',(2.0935328011096,1.11736184088527,24.4264551723904));
#104075=CARTESIAN_POINT('Ctrl Pts',(2.05536045962072,1.18610361502611,24.4317195805305));
#104076=CARTESIAN_POINT('Ctrl Pts',(2.01393889054517,1.25269637488486,24.4369839886706));
#104077=CARTESIAN_POINT('Ctrl Pts',(1.97158008909876,1.32079590746127,24.4423675128613));
#104078=CARTESIAN_POINT('Ctrl Pts',(1.92582353812938,1.38664755401379,24.4477510370521));
#104079=CARTESIAN_POINT('Ctrl Pts',(1.87695710355523,1.44990692594854,24.4531345612429));
#104080=CARTESIAN_POINT('Ctrl Pts',(1.82809066898111,1.51316629788328,24.4585180854337));
#104081=CARTESIAN_POINT('Ctrl Pts',(1.77611475814255,1.57383305154166,24.4639016096245));
#104082=CARTESIAN_POINT('Ctrl Pts',(1.72135581562934,1.63160418560969,24.4692851338153));
#104083=CARTESIAN_POINT('Ctrl Pts',(1.66560241229698,1.69042448400909,24.4747664265829));
#104084=CARTESIAN_POINT('Ctrl Pts',(1.60674482849547,1.74647496705611,24.4802477193504));
#104085=CARTESIAN_POINT('Ctrl Pts',(1.54508202303006,1.79942201959667,24.485729012118));
#104086=CARTESIAN_POINT('Ctrl Pts',(1.48351820138346,1.85228407922429,24.4912015060759));
#104087=CARTESIAN_POINT('Ctrl Pts',(1.41915844225612,1.90205233235669,24.4966740000338));
#104088=CARTESIAN_POINT('Ctrl Pts',(1.35233888606395,1.94842952136825,24.5021464939917));
#104089=CARTESIAN_POINT('Ctrl Pts',(1.28562644926117,1.9947323624426,24.507610214916));
#104090=CARTESIAN_POINT('Ctrl Pts',(1.21646242279782,2.03765471372029,24.5130739358403));
#104091=CARTESIAN_POINT('Ctrl Pts',(1.1452152697361,2.07694006857764,24.5185376567646));
#104092=CARTESIAN_POINT('Ctrl Pts',(1.07403544407832,2.11618829941189,24.5239962145613));
#104093=CARTESIAN_POINT('Ctrl Pts',(1.0007767869189,2.15180615708435,24.529454772358));
#104094=CARTESIAN_POINT('Ctrl Pts',(0.925835471708704,2.18358117362875,
24.5349133301546));
#104095=CARTESIAN_POINT('Ctrl Pts',(0.850946524880646,2.21533398604978,
24.5403680735554));
#104096=CARTESIAN_POINT('Ctrl Pts',(0.774377659975556,2.24324912780332,
24.5458228169563));
#104097=CARTESIAN_POINT('Ctrl Pts',(0.696547330083548,2.26716119397221,
24.5512775603571));
#104098=CARTESIAN_POINT('Ctrl Pts',(0.618752244884669,2.29106243179904,
24.5567298336314));
#104099=CARTESIAN_POINT('Ctrl Pts',(0.539697248628001,2.31096407270931,
24.5621821069058));
#104100=CARTESIAN_POINT('Ctrl Pts',(0.459817314452615,2.32675011546784,
24.5676343801802));
#104101=CARTESIAN_POINT('Ctrl Pts',(0.3799308894113,2.34253744096511,24.5730870964941));
#104102=CARTESIAN_POINT('Ctrl Pts',(0.299219819518825,2.35420840571182,
24.5785398128081));
#104103=CARTESIAN_POINT('Ctrl Pts',(0.218129982814233,2.3616979851576,24.5839925291221));
#104104=CARTESIAN_POINT('Ctrl Pts',(0.137040934973298,2.36918749174275,
24.5894451923906));
#104105=CARTESIAN_POINT('Ctrl Pts',(0.0555735637191289,2.37249565997143,
24.594897855659));
#104106=CARTESIAN_POINT('Ctrl Pts',(-0.0258219500668697,2.37160943019603,
24.6003505189275));
#104107=CARTESIAN_POINT('Ctrl Pts',(-0.107275365906951,2.37072256998633,
24.6058070610388));
#104108=CARTESIAN_POINT('Ctrl Pts',(-0.188656384466935,2.36563536069865,
24.6112636031501));
#104109=CARTESIAN_POINT('Ctrl Pts',(-0.269516104398332,2.35638688079228,
24.6167201452614));
#104110=CARTESIAN_POINT('Ctrl Pts',(-0.326469195812739,2.34987276570507,
24.6205634301743));
#104111=CARTESIAN_POINT('Ctrl Pts',(-0.383163708688597,2.34129533654314,
24.6244067150871));
#104112=CARTESIAN_POINT('Ctrl Pts',(-0.439445221994602,2.3306835819918,
24.62825));
#104113=CARTESIAN_POINT('Ctrl Pts',(-2.3717496963229,0.00120020508255365,
23.846830862774));
#104114=CARTESIAN_POINT('Ctrl Pts',(-2.37172951172941,0.0410873911748103,
23.8439742920646));
#104115=CARTESIAN_POINT('Ctrl Pts',(-2.3707031149012,0.0809706682818765,
23.8411464421663));
#104116=CARTESIAN_POINT('Ctrl Pts',(-2.3677819269107,0.138244320542981,
23.8371431007408));
#104117=CARTESIAN_POINT('Ctrl Pts',(-2.36670035225053,0.155667035764427,
23.8359329655335));
#104118=CARTESIAN_POINT('Ctrl Pts',(-2.36542649454004,0.173076750108263,
23.8347324553251));
#104119=CARTESIAN_POINT('Origin',(0.,0.,24.5));
#104120=CARTESIAN_POINT('',(-2.86732885971112,2.07314048065506E-11,24.1326711402889));
#104121=CARTESIAN_POINT('Ctrl Pts',(-0.439445221994083,2.33068358199193,
24.62825));
#104122=CARTESIAN_POINT('Ctrl Pts',(-0.252498301061248,2.37423453518697,
24.6200912309808));
#104123=CARTESIAN_POINT('Ctrl Pts',(-0.0607381560960383,2.39429049548881,
24.6126350903112));
#104124=CARTESIAN_POINT('Ctrl Pts',(0.331258812598871,2.3882268490475,24.5972095049321));
#104125=CARTESIAN_POINT('Ctrl Pts',(0.530411343122747,2.3601563111261,24.5892481862326));
#104126=CARTESIAN_POINT('Ctrl Pts',(1.0261899805794,2.22744702151644,24.5675775528286));
#104127=CARTESIAN_POINT('Ctrl Pts',(1.31173953974594,2.08916181590285,24.5530814337998));
#104128=CARTESIAN_POINT('Ctrl Pts',(1.86756500186408,1.67230844586517,24.5222920288584));
#104129=CARTESIAN_POINT('Ctrl Pts',(2.06239788769764,1.41434287106475,24.5109590645687));
#104130=CARTESIAN_POINT('Ctrl Pts',(2.33502645953121,0.960352452908593,
24.4915954879617));
#104131=CARTESIAN_POINT('Ctrl Pts',(2.44004047150229,0.689439917790241,
24.4807543798427));
#104132=CARTESIAN_POINT('Ctrl Pts',(2.56661735298791,0.0761676158146572,
24.4546463607253));
#104133=CARTESIAN_POINT('Ctrl Pts',(2.56936506573517,-0.267196718376941,
24.4390319275492));
#104134=CARTESIAN_POINT('Ctrl Pts',(2.43860393076487,-0.928950669615914,
24.4121318022675));
#104135=CARTESIAN_POINT('Ctrl Pts',(2.30709388532842,-1.24234973758447,
24.4012358857251));
#104136=CARTESIAN_POINT('Ctrl Pts',(2.03281881994024,-1.65534374027188,
24.3833376745132));
#104137=CARTESIAN_POINT('Ctrl Pts',(1.93226128984899,-1.78052177711593,
24.377347194124));
#104138=CARTESIAN_POINT('Ctrl Pts',(1.57667382943023,-2.14998763016186,
24.3572490357678));
#104139=CARTESIAN_POINT('Ctrl Pts',(1.28320635471831,-2.354434589116,24.3418379695899));
#104140=CARTESIAN_POINT('Ctrl Pts',(0.690934627167233,-2.60924580390895,
24.3166545770257));
#104141=CARTESIAN_POINT('Ctrl Pts',(0.405746860161139,-2.67782592413793,
24.3071921961513));
#104142=CARTESIAN_POINT('Ctrl Pts',(-0.238690314097037,-2.72752391529108,
24.2852767058604));
#104143=CARTESIAN_POINT('Ctrl Pts',(-0.597229103766921,-2.68511165509286,
24.2723822195236));
#104144=CARTESIAN_POINT('Ctrl Pts',(-1.18860058374266,-2.49648698036282,
24.2476728398377));
#104145=CARTESIAN_POINT('Ctrl Pts',(-1.51651301242023,-2.35274314730956,
24.2325132567834));
#104146=CARTESIAN_POINT('Ctrl Pts',(-2.1008881867237,-1.87203354808299,
24.2062476358257));
#104147=CARTESIAN_POINT('Ctrl Pts',(-2.3194136975749,-1.61103995421478,
24.1961087219178));
#104148=CARTESIAN_POINT('Ctrl Pts',(-2.59356453211614,-1.13401729928166,
24.1773943967977));
#104149=CARTESIAN_POINT('Ctrl Pts',(-2.67903863724766,-0.937448621830812,
24.1696977612319));
#104150=CARTESIAN_POINT('Ctrl Pts',(-2.81541952069172,-0.495679813412592,
24.1521284724464));
#104151=CARTESIAN_POINT('Ctrl Pts',(-2.85786427493396,-0.248796193213268,
24.1421357250696));
#104152=CARTESIAN_POINT('Ctrl Pts',(-2.86732885971112,4.1433870223706E-11,
24.1326711402889));
#104153=CARTESIAN_POINT('Ctrl Pts',(0.261019001493371,2.92766592745733,
24.0607213977006));
#104154=CARTESIAN_POINT('Ctrl Pts',(0.163059463857162,2.92391694727034,
24.0731547417967));
#104155=CARTESIAN_POINT('Ctrl Pts',(0.065549179711928,2.91537842014871,
24.085491147687));
#104156=CARTESIAN_POINT('Ctrl Pts',(-0.0310928127263946,2.90207104271783,
24.0977623977378));
#104157=CARTESIAN_POINT('Ctrl Pts',(-0.129744753844374,2.88848690003178,
24.1102888637896));
#104158=CARTESIAN_POINT('Ctrl Pts',(-0.227491648374659,2.86993346603253,
24.1227473148004));
#104159=CARTESIAN_POINT('Ctrl Pts',(-0.323877162841241,2.84642522927533,
24.135208035046));
#104160=CARTESIAN_POINT('Ctrl Pts',(-0.414180307230089,2.82440047057626,
24.1468824264289));
#104161=CARTESIAN_POINT('Ctrl Pts',(-0.503288202647077,2.79802678119133,
24.1585592114491));
#104162=CARTESIAN_POINT('Ctrl Pts',(-0.59082047893217,2.76730769459531,
24.1703249806927));
#104163=CARTESIAN_POINT('Ctrl Pts',(-0.619499004310833,2.75724308595102,
24.1741798434492));
#104164=CARTESIAN_POINT('Ctrl Pts',(-0.648008369034724,2.74671193578173,
24.1780444749336));
#104165=CARTESIAN_POINT('Ctrl Pts',(-0.67633512265761,2.73571405062978,
24.1819225409948));
#104166=CARTESIAN_POINT('Ctrl Pts',(-0.698212434468718,2.72722016651107,
24.1849176480788));
#104167=CARTESIAN_POINT('Ctrl Pts',(-0.719980822195904,2.71844788221606,
24.1879207747589));
#104168=CARTESIAN_POINT('Ctrl Pts',(-0.741634076278984,2.70939702033487,
24.1909337286391));
#104169=CARTESIAN_POINT('Ctrl Pts',(-0.754534483051411,2.70400476846083,
24.1927287627938));
#104170=CARTESIAN_POINT('Ctrl Pts',(-0.767392655677935,2.69851414135042,
24.1945271022539));
#104171=CARTESIAN_POINT('Ctrl Pts',(-0.780196516280907,2.69293005235174,
24.1963276099237));
#104172=CARTESIAN_POINT('Ctrl Pts',(-0.863568168703393,2.65656955597254,
24.2080515191642));
#104173=CARTESIAN_POINT('Ctrl Pts',(-0.944764154889942,2.61619706804206,
24.2198839165918));
#104174=CARTESIAN_POINT('Ctrl Pts',(-1.02351699322116,2.57187520645671,
24.2319448862063));
#104175=CARTESIAN_POINT('Ctrl Pts',(-1.06274981800173,2.54979509015393,
24.2379533795839));
#104176=CARTESIAN_POINT('Ctrl Pts',(-1.10137646364671,2.52673412661812,
24.2440188319126));
#104177=CARTESIAN_POINT('Ctrl Pts',(-1.13936436506882,2.50269537352569,
24.2501572246662));
#104178=CARTESIAN_POINT('Ctrl Pts',(-1.21752318249746,2.45323645519046,
24.2627867593489));
#104179=CARTESIAN_POINT('Ctrl Pts',(-1.29298521017775,2.39963837998968,
24.2757248979837));
#104180=CARTESIAN_POINT('Ctrl Pts',(-1.36553505111976,2.34210598208496,
24.288884656243));
#104181=CARTESIAN_POINT('Ctrl Pts',(-1.4404209245149,2.28272109840127,24.302468145581));
#104182=CARTESIAN_POINT('Ctrl Pts',(-1.51220416706068,2.21914223789968,
24.3162871082082));
#104183=CARTESIAN_POINT('Ctrl Pts',(-1.58055507906647,2.15159877555774,
24.3302562578134));
#104184=CARTESIAN_POINT('Ctrl Pts',(-1.59151079358875,2.14077248415138,
24.3324953210637));
#104185=CARTESIAN_POINT('Ctrl Pts',(-1.60237813755092,2.12984438461238,
24.3347382762028));
#104186=CARTESIAN_POINT('Ctrl Pts',(-1.61315554165587,2.1188154898271,24.3369848138799));
#104187=CARTESIAN_POINT('Ctrl Pts',(-1.62162021392896,2.11015329446144,
24.3387492652264));
#104188=CARTESIAN_POINT('Ctrl Pts',(-1.63002854377014,2.1014297392921,24.3405157547639));
#104189=CARTESIAN_POINT('Ctrl Pts',(-1.63837321661078,2.09265245906859,
24.3422827254666));
#104190=CARTESIAN_POINT('Ctrl Pts',(-1.70020980675046,2.02761011527781,
24.3553765213791));
#104191=CARTESIAN_POINT('Ctrl Pts',(-1.75865725508163,1.9595127394449,24.3685160721984));
#104192=CARTESIAN_POINT('Ctrl Pts',(-1.81349417189549,1.88863596512469,
24.3816595102506));
#104193=CARTESIAN_POINT('Ctrl Pts',(-1.86812219692787,1.81802918365808,
24.3947528806412));
#104194=CARTESIAN_POINT('Ctrl Pts',(-1.9191664041851,1.74466328829154,24.4078498587507));
#104195=CARTESIAN_POINT('Ctrl Pts',(-1.96636441994797,1.66882873674077,
24.4209345908626));
#104196=CARTESIAN_POINT('Ctrl Pts',(-2.01275888332875,1.5942852783336,24.4337965537015));
#104197=CARTESIAN_POINT('Ctrl Pts',(-2.05543625621973,1.51735616516087,
24.44664654175));
#104198=CARTESIAN_POINT('Ctrl Pts',(-2.09411646704632,1.43834332346446,
24.4594970392244));
#104199=CARTESIAN_POINT('Ctrl Pts',(-2.11496000855021,1.39576580358944,
24.4664217656344));
#104200=CARTESIAN_POINT('Ctrl Pts',(-2.13464239483683,1.35258370172021,
24.4733471300791));
#104201=CARTESIAN_POINT('Ctrl Pts',(-2.15311705514232,1.30884776401137,
24.4802786815796));
#104202=CARTESIAN_POINT('Ctrl Pts',(-2.15871542149974,1.29559448637429,
24.4823791458958));
#104203=CARTESIAN_POINT('Ctrl Pts',(-2.16420353529864,1.28228872410263,
24.4844804552686));
#104204=CARTESIAN_POINT('Ctrl Pts',(-2.16957799719695,1.26893709952057,
24.4865819988588));
#104205=CARTESIAN_POINT('Ctrl Pts',(-2.20143397005055,1.18979820184384,
24.4990384487929));
#104206=CARTESIAN_POINT('Ctrl Pts',(-2.22918818249487,1.10932539194073,
24.511457595635));
#104207=CARTESIAN_POINT('Ctrl Pts',(-2.25269334859829,1.02782771604728,
24.5239028418307));
#104208=CARTESIAN_POINT('Ctrl Pts',(-2.27585078395726,0.947535700534353,
24.5361639755337));
#104209=CARTESIAN_POINT('Ctrl Pts',(-2.29488421224564,0.866249028053862,
24.5484506467591));
#104210=CARTESIAN_POINT('Ctrl Pts',(-2.30963484158374,0.784256574631775,
24.5608461556698));
#104211=CARTESIAN_POINT('Ctrl Pts',(-2.32395200420878,0.704673577678735,
24.5728774061898));
#104212=CARTESIAN_POINT('Ctrl Pts',(-2.33423483748586,0.62442576084056,
24.5850115045248));
#104213=CARTESIAN_POINT('Ctrl Pts',(-2.34031596902869,0.54376943844709,
24.5973422971468));
#104214=CARTESIAN_POINT('Ctrl Pts',(-2.34532119633868,0.477383236352302,
24.607491464214));
#104215=CARTESIAN_POINT('Ctrl Pts',(-2.34747983552917,0.410720154511199,
24.6177743044544));
#104216=CARTESIAN_POINT('Ctrl Pts',(-2.34668236863854,0.343918483395396,
24.62825));
#104217=CARTESIAN_POINT('',(-2.86788692854124,0.00160361121558927,24.1321126231202));
#104218=CARTESIAN_POINT('Ctrl Pts',(-2.86788692854124,0.00160361121558927,
24.1321126231202));
#104219=CARTESIAN_POINT('Ctrl Pts',(-2.87138354375354,0.0925483242271544,
24.1285651557038));
#104220=CARTESIAN_POINT('Ctrl Pts',(-2.87043240913469,0.183377764669063,
24.1251424880545));
#104221=CARTESIAN_POINT('Ctrl Pts',(-2.86500154312585,0.273846896636642,
24.121940590448));
#104222=CARTESIAN_POINT('Ctrl Pts',(-2.8596177192724,0.363532385082704,
24.118766427675));
#104223=CARTESIAN_POINT('Ctrl Pts',(-2.84983102614631,0.45287124908063,
24.1158088702711));
#104224=CARTESIAN_POINT('Ctrl Pts',(-2.83576722797345,0.541646561528832,
24.112967480463));
#104225=CARTESIAN_POINT('Ctrl Pts',(-2.83488131448154,0.547238738413019,
24.112788494279));
#104226=CARTESIAN_POINT('Ctrl Pts',(-2.83397841666917,0.552828690663718,
24.1126099690542));
#104227=CARTESIAN_POINT('Ctrl Pts',(-2.83305856079414,0.558416368474958,
24.1124318796832));
#104228=CARTESIAN_POINT('Ctrl Pts',(-2.81723894257586,0.654512868045957,
24.1093691109023));
#104229=CARTESIAN_POINT('Ctrl Pts',(-2.79640642791614,0.749933056172748,
24.1064347116094));
#104230=CARTESIAN_POINT('Ctrl Pts',(-2.77068225948842,0.844353392490152,
24.1035171613742));
#104231=CARTESIAN_POINT('Ctrl Pts',(-2.75536245067389,0.90058461740422,
24.1017796392485));
#104232=CARTESIAN_POINT('Ctrl Pts',(-2.7383071381334,0.95646026262038,24.1000484439012));
#104233=CARTESIAN_POINT('Ctrl Pts',(-2.71953884864361,1.01190378419375,
24.0983038033337));
#104234=CARTESIAN_POINT('Ctrl Pts',(-2.71440485874386,1.02707013592327,
24.0978265639424));
#104235=CARTESIAN_POINT('Ctrl Pts',(-2.70914211347083,1.0422054863952,24.0973482919757));
#104236=CARTESIAN_POINT('Ctrl Pts',(-2.70375754058507,1.05729073335641,
24.0968691842923));
#104237=CARTESIAN_POINT('Ctrl Pts',(-2.67057083570499,1.15026554297752,
24.0939163028599));
#104238=CARTESIAN_POINT('Ctrl Pts',(-2.63270767785936,1.24148802007126,
24.0909242366852));
#104239=CARTESIAN_POINT('Ctrl Pts',(-2.59041302986795,1.33060124549307,
24.0878291018868));
#104240=CARTESIAN_POINT('Ctrl Pts',(-2.54756420783155,1.42088209469093,
24.0846934124686));
#104241=CARTESIAN_POINT('Ctrl Pts',(-2.5001667870123,1.50899753746854,24.0814517729648));
#104242=CARTESIAN_POINT('Ctrl Pts',(-2.44846895759319,1.59456926778762,
24.078074027962));
#104243=CARTESIAN_POINT('Ctrl Pts',(-2.39685116861105,1.68000851287929,
24.0747015125054));
#104244=CARTESIAN_POINT('Ctrl Pts',(-2.34094650304388,1.76291158751629,
24.0711933279152));
#104245=CARTESIAN_POINT('Ctrl Pts',(-2.28099543401435,1.84290139915102,
24.0675563539964));
#104246=CARTESIAN_POINT('Ctrl Pts',(-2.23753645918706,1.9008866071973,24.0649198846132));
#104247=CARTESIAN_POINT('Ctrl Pts',(-2.19195107688015,1.95734095850997,
24.0622165183716));
#104248=CARTESIAN_POINT('Ctrl Pts',(-2.14432694750403,2.01212145383533,
24.0594607972727));
#104249=CARTESIAN_POINT('Ctrl Pts',(-2.86732885971111,4.14306955368129E-11,
24.1326711402889));
#104250=CARTESIAN_POINT('Ctrl Pts',(-2.86734966299874,0.000546857498953776,
24.1326503370013));
#104251=CARTESIAN_POINT('Ctrl Pts',(-2.8673703069382,0.00109372421048583,
24.1326295366167));
#104252=CARTESIAN_POINT('Ctrl Pts',(-2.86739079150826,0.00164060010131629,
24.1326087391507));
#104253=CARTESIAN_POINT('',(-2.,-2.44929359829471E-16,25.));
#104254=CARTESIAN_POINT('',(-2.5,3.06161699786838E-16,24.5));
#104255=CARTESIAN_POINT('Origin',(0.,0.,25.));
#104256=CARTESIAN_POINT('Ctrl Pts',(1.70915978346929,-2.39931405854793,
-0.331525224265037));
#104257=CARTESIAN_POINT('Ctrl Pts',(2.50802990535057,-1.83028257961684,
-0.278535267625054));
#104258=CARTESIAN_POINT('Ctrl Pts',(3.47835091600118,0.158233065351694,
-0.172581332490446));
#104259=CARTESIAN_POINT('Ctrl Pts',(1.74735082995237,3.01534926870841,-0.0136634188612144));
#104260=CARTESIAN_POINT('Ctrl Pts',(-1.58653605777943,3.09925236818656,
0.145228516622657));
#104261=CARTESIAN_POINT('Ctrl Pts',(-3.46537971655703,0.346752180227429,
0.304120452106527));
#104262=CARTESIAN_POINT('Ctrl Pts',(-2.16822080433006,-2.72587883991964,
0.463012387590399));
#104263=CARTESIAN_POINT('Ctrl Pts',(1.11658306675895,-3.29872810449766,
0.621904323074271));
#104264=CARTESIAN_POINT('Ctrl Pts',(3.37779425300656,-0.848538639554367,
0.780796258558139));
#104265=CARTESIAN_POINT('Ctrl Pts',(2.54292626363602,2.37976338639486,0.939688194042012));
#104266=CARTESIAN_POINT('Ctrl Pts',(-0.622859592152919,3.42656460546492,
1.09858012952589));
#104267=CARTESIAN_POINT('Ctrl Pts',(-3.21770598735519,1.33261290508638,
1.25747206500976));
#104268=CARTESIAN_POINT('Ctrl Pts',(-2.86316102813789,-1.98288004182896,
1.41636400049363));
#104269=CARTESIAN_POINT('Ctrl Pts',(0.115806994067153,-3.48080913522564,
1.5752559359775));
#104270=CARTESIAN_POINT('Ctrl Pts',(2.98862212193643,-1.78818668555055,
1.73414787146137));
#104271=CARTESIAN_POINT('Ctrl Pts',(3.12202035689114,1.54352265706882,1.89303980694524));
#104272=CARTESIAN_POINT('Ctrl Pts',(0.393724875594412,3.4604112461881,2.05193174242911));
#104273=CARTESIAN_POINT('Ctrl Pts',(-2.69546468997399,2.20543421423937,
2.21082367791299));
#104274=CARTESIAN_POINT('Ctrl Pts',(-3.31394901819685,-1.07107955396263,
2.36971561339685));
#104275=CARTESIAN_POINT('Ctrl Pts',(-0.894815353243767,-3.36582441055242,
2.52860754888072));
#104276=CARTESIAN_POINT('Ctrl Pts',(2.34452011799349,-2.57540183372274,
2.6874994843646));
#104277=CARTESIAN_POINT('Ctrl Pts',(3.43483152420483,0.575674793782504,
2.84639141984846));
#104278=CARTESIAN_POINT('Ctrl Pts',(1.37672220743361,3.19907875884332,3.00528335533234));
#104279=CARTESIAN_POINT('Ctrl Pts',(-1.94331237532776,2.89015675325956,
3.1641752908162));
#104280=CARTESIAN_POINT('Ctrl Pts',(-3.48207621113987,-0.0679285026538166,
3.32306722630008));
#104281=CARTESIAN_POINT('Ctrl Pts',(-1.8291141108827,-2.96374941187267,
3.48195916178395));
#104282=CARTESIAN_POINT('Ctrl Pts',(1.50044281000745,-3.14295090576371,
3.64085109726782));
#104283=CARTESIAN_POINT('Ctrl Pts',(3.45467020416205,-0.441274062288436,
3.79974303275169));
#104284=CARTESIAN_POINT('Ctrl Pts',(2.24229244183481,2.66488153982562,3.95863496823556));
#104285=CARTESIAN_POINT('Ctrl Pts',(-1.02540591201219,3.3283647236689,4.11752690371944));
#104286=CARTESIAN_POINT('Ctrl Pts',(-3.35320104615321,0.941016344939749,
4.2764188392033));
#104287=CARTESIAN_POINT('Ctrl Pts',(-2.6073992534791,-2.30888244615925,
4.43531077468718));
#104288=CARTESIAN_POINT('Ctrl Pts',(0.528385788631286,-3.44242319825643,
4.59420271017105));
#104289=CARTESIAN_POINT('Ctrl Pts',(3.17984408930906,-1.42058459272181,
4.75309464565492));
#104290=CARTESIAN_POINT('Ctrl Pts',(2.91660718202859,1.90338423948601,4.91198658113878));
#104291=CARTESIAN_POINT('Ctrl Pts',(-0.0200378352627403,3.48268107965435,
5.07087851662267));
#104292=CARTESIAN_POINT('Ctrl Pts',(-2.93831585694904,1.86969755367164,
5.22977045210653));
#104293=CARTESIAN_POINT('Ctrl Pts',(-3.16328725505062,-1.45708021722857,
5.3886623875904));
#104294=CARTESIAN_POINT('Ctrl Pts',(-0.488739700424178,-3.44827529681711,
5.54755432307427));
#104295=CARTESIAN_POINT('Ctrl Pts',(2.63379436635632,-2.27872689306034,
5.70644625855815));
#104296=CARTESIAN_POINT('Ctrl Pts',(3.34215100721795,0.979538494577416,
5.86533819404202));
#104297=CARTESIAN_POINT('Ctrl Pts',(0.987039361146014,3.33994346014362,
6.02423012952589));
#104298=CARTESIAN_POINT('Ctrl Pts',(-2.27280811951147,2.63890361121622,
6.18312206500976));
#104299=CARTESIAN_POINT('Ctrl Pts',(-3.44936385740458,-0.480996877992278,
6.34201400049363));
#104300=CARTESIAN_POINT('Ctrl Pts',(-1.46417832016298,-3.16000804811825,
6.5009059359775));
#104301=CARTESIAN_POINT('Ctrl Pts',(1.86309614141146,-2.94250603827164,
6.65979787146138));
#104302=CARTESIAN_POINT('Ctrl Pts',(3.48262731658261,-0.0278566186018233,
6.81868980694524));
#104303=CARTESIAN_POINT('Ctrl Pts',(1.90992740569023,2.91232661671056,6.97758174242912));
#104304=CARTESIAN_POINT('Ctrl Pts',(-1.41344206652397,3.18302537564308,
7.13647367791298));
#104305=CARTESIAN_POINT('Ctrl Pts',(-3.4412282641157,0.536112909430946,
7.29536561339686));
#104306=CARTESIAN_POINT('Ctrl Pts',(-2.31473039960172,-2.60220909893247,
7.45425754888073));
#104307=CARTESIAN_POINT('Ctrl Pts',(0.933485830320249,-3.35530523529509,
7.6131494843646));
#104308=CARTESIAN_POINT('Ctrl Pts',(3.32605423603801,-1.03287571195233,
7.77204141984847));
#104309=CARTESIAN_POINT('Ctrl Pts',(2.66990890897756,2.23630396752532,7.93093335533233));
#104310=CARTESIAN_POINT('Ctrl Pts',(-0.433517002948718,3.45565218527005,
8.08982529081622));
#104311=CARTESIAN_POINT('Ctrl Pts',(-3.13957439756035,1.50749514745186,
8.24871722630007));
#104312=CARTESIAN_POINT('Ctrl Pts',(-2.96784841834379,-1.82245570128375,
8.40760916178396));
#104313=CARTESIAN_POINT('Ctrl Pts',(-0.0757458043231992,-3.48191493154769,
8.56650109726781));
#104314=CARTESIAN_POINT('Ctrl Pts',(2.88578660772602,-1.94979605909861,
8.72539303275171));
#104315=CARTESIAN_POINT('Ctrl Pts',(3.20216153391245,1.36953661073329,8.88428496823555));
#104316=CARTESIAN_POINT('Ctrl Pts',(0.58338473069051,3.4335304386891,9.04317690371945));
#104317=CARTESIAN_POINT('Ctrl Pts',(-2.57013171107317,2.35029615264616,
9.2020688392033));
#104318=CARTESIAN_POINT('Ctrl Pts',(-3.36782492010113,-0.887256628576624,
9.36096077468718));
#104319=CARTESIAN_POINT('Ctrl Pts',(-1.07851672901495,-3.31153600050524,
9.51985271017105));
#104320=CARTESIAN_POINT('Ctrl Pts',(2.19937689376752,-2.70040928315855,
9.67874464565492));
#104321=CARTESIAN_POINT('Ctrl Pts',(3.4612869926098,0.385955142727138,9.8376365811388));
#104322=CARTESIAN_POINT('Ctrl Pts',(1.55052688267461,3.11854700197234,9.99652851662266));
#104323=CARTESIAN_POINT('Ctrl Pts',(-1.78147060488158,2.99262952958601,
10.1554204521065));
#104324=CARTESIAN_POINT('Ctrl Pts',(-3.48054405927083,0.12362066527021,
10.3143123875904));
#104325=CARTESIAN_POINT('Ctrl Pts',(-1.98929597408154,-2.85870084914638,
10.4732043230742));
#104326=CARTESIAN_POINT('Ctrl Pts',(1.32537215309932,-3.22069211089731,
10.6320962585581));
#104327=CARTESIAN_POINT('Ctrl Pts',(3.42518327632198,-0.630546224325814,
10.790988194042));
#104328=CARTESIAN_POINT('Ctrl Pts',(2.38541742612644,2.53756826913872,10.9498801295259));
#104329=CARTESIAN_POINT('Ctrl Pts',(-0.840859632047186,3.37970769395828,
11.1087720650097));
#104330=CARTESIAN_POINT('Ctrl Pts',(-3.29639149918183,1.12395378086871,
11.2676640004936));
#104331=CARTESIAN_POINT('Ctrl Pts',(-2.73039896563801,-2.16203388175354,
11.4265559359775));
#104332=CARTESIAN_POINT('Ctrl Pts',(0.338320292055619,-3.46626721378932,
11.5854478714614));
#104333=CARTESIAN_POINT('Ctrl Pts',(3.09692983797972,-1.59326538782405,
11.7443398069452));
#104334=CARTESIAN_POINT('Ctrl Pts',(3.0168446854836,1.74014860315912,11.9032317424291));
#104335=CARTESIAN_POINT('Ctrl Pts',(0.171472147521156,3.47851495900647,
12.062123677913));
#104336=CARTESIAN_POINT('Ctrl Pts',(-2.83107446333298,2.02841968055707,
12.2210156133968));
#104337=CARTESIAN_POINT('Ctrl Pts',(-3.23861360216155,-1.28095704584561,
12.3799075488807));
#104338=CARTESIAN_POINT('Ctrl Pts',(-0.677588471324607,-3.41618835559974,
12.5387994843646));
#104339=CARTESIAN_POINT('Ctrl Pts',(2.50452493141022,-2.42008757803348,
12.6976914198484));
#104340=CARTESIAN_POINT('Ctrl Pts',(3.39095130963907,0.794303615165157,
12.8565833553323));
#104341=CARTESIAN_POINT('Ctrl Pts',(1.16917827462158,3.28062359614148,13.0154752908162));
#104342=CARTESIAN_POINT('Ctrl Pts',(-2.12428199365964,2.75987228487492,
13.1743672263));
#104343=CARTESIAN_POINT('Ctrl Pts',(-3.47059190696705,-0.290621459465966,
13.3332591617839));
#104344=CARTESIAN_POINT('Ctrl Pts',(-1.63570258034773,-3.07472699374288,
13.4921510972678));
#104345=CARTESIAN_POINT('Ctrl Pts',(1.6984975107849,-3.04048930655329,13.6510430327517));
#104346=CARTESIAN_POINT('Ctrl Pts',(3.47582801449077,-0.219291201575626,
13.8099349682355));
#104347=CARTESIAN_POINT('Ctrl Pts',(2.06715977959038,2.80291267488859,13.9688269037194));
#104348=CARTESIAN_POINT('Ctrl Pts',(-1.23629968859761,3.25592261845714,
14.1277188392033));
#104349=CARTESIAN_POINT('Ctrl Pts',(-3.40654737760948,0.724502575226165,
14.2866107746872));
#104350=CARTESIAN_POINT('Ctrl Pts',(-2.45430005167269,-2.47100794692505,
14.445502710171));
#104351=CARTESIAN_POINT('Ctrl Pts',(0.747597382437242,-3.40155364079126,
14.6043946456549));
#104352=CARTESIAN_POINT('Ctrl Pts',(3.26423527335331,-1.21418165757984,
14.7632865811388));
#104353=CARTESIAN_POINT('Ctrl Pts',(2.7888236669811,2.08612836898727,14.9221785166226));
#104354=CARTESIAN_POINT('Ctrl Pts',(-0.242867665590079,3.47426025427258,
15.0810704521065));
#104355=CARTESIAN_POINT('Ctrl Pts',(-3.05194266818393,1.67783043467617,
15.2399623875904));
#104356=CARTESIAN_POINT('Ctrl Pts',(-3.06355892120926,-1.65652520466382,
15.3988543230742));
#104357=CARTESIAN_POINT('Ctrl Pts',(-0.267068784065951,-3.47248373386902,
15.5577462585581));
#104358=CARTESIAN_POINT('Ctrl Pts',(2.77422080966953,-2.10550894479311,
15.716638194042));
#104359=CARTESIAN_POINT('Ctrl Pts',(3.27261588636508,1.19140852679432,15.8755301295258));
#104360=CARTESIAN_POINT('Ctrl Pts',(0.771279663803726,3.39626216561827,
16.0344220650098));
#104361=CARTESIAN_POINT('Ctrl Pts',(-2.43702365429483,2.48804837690404,
16.1933140004936));
#104362=CARTESIAN_POINT('Ctrl Pts',(-3.41151268234012,-0.70074976677835,
16.3522059359775));
#104363=CARTESIAN_POINT('Ctrl Pts',(-1.25895541886534,-3.2472296301181,
16.5110978714614));
#104364=CARTESIAN_POINT('Ctrl Pts',(2.04758022321287,-2.81724763677509,
16.6699898069452));
#104365=CARTESIAN_POINT('Ctrl Pts',(3.47727156196124,0.195067941453848,
16.8288817424291));
#104366=CARTESIAN_POINT('Ctrl Pts',(1.71964098374098,3.0285811701927,16.9877736779129));
#104367=CARTESIAN_POINT('Ctrl Pts',(-1.61423962244767,3.08604916660887,
17.1466656133968));
#104368=CARTESIAN_POINT('Ctrl Pts',(-3.46848274959953,0.31479585946735,
17.3055575488807));
#104369=CARTESIAN_POINT('Ctrl Pts',(-2.14345992370895,-2.74500429377823,
17.4644494843646));
#104370=CARTESIAN_POINT('Ctrl Pts',(1.14629205009097,-3.28869024891454,
17.6233414198484));
#104371=CARTESIAN_POINT('Ctrl Pts',(3.38533466472848,-0.817910890742338,
17.7822333553323));
#104372=CARTESIAN_POINT('Ctrl Pts',(2.52132617136549,2.40257848050695,17.9411252908162));
#104373=CARTESIAN_POINT('Ctrl Pts',(-0.653769627841278,3.42082655086738,
18.1000172263));
#104374=CARTESIAN_POINT('Ctrl Pts',(-3.2296098824818,1.30349109102539,18.2589091617839));
#104375=CARTESIAN_POINT('Ctrl Pts',(-2.84513881881822,-2.00864484642347,
18.4178010972678));
#104376=CARTESIAN_POINT('Ctrl Pts',(0.147231326769927,-3.4796252605449,
18.5766930327517));
#104377=CARTESIAN_POINT('Ctrl Pts',(3.00464691781065,-1.7611263204821,18.7355849682355));
#104378=CARTESIAN_POINT('Ctrl Pts',(3.10795578947974,1.57164876103529,18.8944769037194));
#104379=CARTESIAN_POINT('Ctrl Pts',(0.362463401803061,3.4638258183312,19.0533688392033));
#104380=CARTESIAN_POINT('Ctrl Pts',(-2.71526865252999,2.18100553919064,
19.2122607746872));
#104381=CARTESIAN_POINT('Ctrl Pts',(-3.30414266619359,-1.10095879076405,
19.371152710171));
#104382=CARTESIAN_POINT('Ctrl Pts',(-0.864387437285646,-3.37376694148966,
19.5300446456549));
#104383=CARTESIAN_POINT('Ctrl Pts',(2.3676789396587,-2.55412714171859,19.6889365811388));
#104384=CARTESIAN_POINT('Ctrl Pts',(3.42949348506363,0.606665850414551,
19.8478285166226));
#104385=CARTESIAN_POINT('Ctrl Pts',(1.34778025145053,3.21137936248784,20.0067204521065));
#104386=CARTESIAN_POINT('Ctrl Pts',(-1.96932960158824,2.87249193869747,
20.1656123875904));
#104387=CARTESIAN_POINT('Ctrl Pts',(-3.48132090556751,-0.0993668687370002,
20.3245043230742));
#104388=CARTESIAN_POINT('Ctrl Pts',(-1.80227859806866,-2.98014443642408,
20.4833962585581));
#104389=CARTESIAN_POINT('Ctrl Pts',(1.52876067262735,-3.12927464877839,
20.642288194042));
#104390=CARTESIAN_POINT('Ctrl Pts',(3.45851382540476,-0.410062392811356,
20.8011801295258));
#104391=CARTESIAN_POINT('Ctrl Pts',(2.21813868189191,2.68501950265137,20.9600720650098));
#104392=CARTESIAN_POINT('Ctrl Pts',(-1.05541730517558,3.31897022882153,
21.1189640004936));
#104393=CARTESIAN_POINT('Ctrl Pts',(-3.36156121580965,0.910700489284517,
21.2778559359775));
#104394=CARTESIAN_POINT('Ctrl Pts',(-2.58644502317988,-2.33233158473218,
21.4367478714614));
#104395=CARTESIAN_POINT('Ctrl Pts',(0.559447225046381,-3.43751193576291,
21.5956398069452));
#104396=CARTESIAN_POINT('Ctrl Pts',(3.19254174220684,-1.39181435274289,
21.7545317424291));
#104397=CARTESIAN_POINT('Ctrl Pts',(2.89930139518638,1.9296415963275,21.913423677913));
#104398=CARTESIAN_POINT('Ctrl Pts',(-0.0514828017540393,3.48235880156699,
22.0723156133968));
#104399=CARTESIAN_POINT('Ctrl Pts',(-2.95507992042546,1.84308884050832,
22.2312075488807));
#104400=CARTESIAN_POINT('Ctrl Pts',(-3.14999873389981,-1.48558119003127,
22.3900994843646));
#104401=CARTESIAN_POINT('Ctrl Pts',(-0.457589516865705,-3.45255212377537,
22.5489914198484));
#104402=CARTESIAN_POINT('Ctrl Pts',(2.65427341857437,-2.25484402904363,
22.7078833553323));
#104403=CARTESIAN_POINT('Ctrl Pts',(3.33314941459721,1.00966036216743,22.8667752908162));
#104404=CARTESIAN_POINT('Ctrl Pts',(0.956880835440033,3.34875003908667,
23.0256672263001));
#104405=CARTESIAN_POINT('Ctrl Pts',(-2.29661858999409,2.61821597477262,
23.1845591617839));
#104406=CARTESIAN_POINT('Ctrl Pts',(-3.4447362843645,-0.512012483791419,
23.3434510972678));
#104407=CARTESIAN_POINT('Ctrl Pts',(-1.43586018489416,-3.17331095792505,
23.5023430327517));
#104408=CARTESIAN_POINT('Ctrl Pts',(1.89011394218839,-2.92516032722353,
23.6612349682356));
#104409=CARTESIAN_POINT('Ctrl Pts',(3.48173145950731,0.00281925901121507,
23.8201269037194));
#104410=CARTESIAN_POINT('Ctrl Pts',(1.88550732670284,2.93094323660242,23.9790188392033));
#104411=CARTESIAN_POINT('Ctrl Pts',(-1.44671136682348,3.16717464109652,
24.1379368411285));
#104412=CARTESIAN_POINT('Ctrl Pts',(-2.77319825394964,1.39625348399268,
24.243890864559));
#104413=CARTESIAN_POINT('Ctrl Pts',(-2.91490778362121,0.425731991800965,
24.2968809094949));
#104414=CARTESIAN_POINT('Ctrl Pts',(1.5973099225308,-2.24229951468148,-0.220223892917422));
#104415=CARTESIAN_POINT('Ctrl Pts',(2.3439008409669,-1.71050626964966,-0.167233936277439));
#104416=CARTESIAN_POINT('Ctrl Pts',(3.25072265677533,0.147878067225332,
-0.0612800011428309));
#104417=CARTESIAN_POINT('Ctrl Pts',(1.63300169230522,2.81802049953892,0.0976379124864005));
#104418=CARTESIAN_POINT('Ctrl Pts',(-1.48271086884576,2.89643286017587,
0.256529847970272));
#104419=CARTESIAN_POINT('Ctrl Pts',(-3.23860031117624,0.324060221574034,
0.415421783454143));
#104420=CARTESIAN_POINT('Ctrl Pts',(-2.02632933356543,-2.54749342965608,
0.574313718938014));
#104421=CARTESIAN_POINT('Ctrl Pts',(1.04351227375809,-3.0828546189813,0.733205654421883));
#104422=CARTESIAN_POINT('Ctrl Pts',(3.15674656563897,-0.793009057268962,
0.892097589905756));
#104423=CARTESIAN_POINT('Ctrl Pts',(2.37651353165193,2.22402826647853,1.05098952538963));
#104424=CARTESIAN_POINT('Ctrl Pts',(-0.582098769530993,3.20232531647345,
1.2098814608735));
#104425=CARTESIAN_POINT('Ctrl Pts',(-3.00713470507515,1.24540481046566,
1.36877339635737));
#104426=CARTESIAN_POINT('Ctrl Pts',(-2.67579167511483,-1.85311753566579,
1.52766533184124));
#104427=CARTESIAN_POINT('Ctrl Pts',(0.108228418730068,-3.2530200066176,
1.68655726732511));
#104428=CARTESIAN_POINT('Ctrl Pts',(2.79304241548106,-1.67116519110322,
1.84544920280898));
#104429=CARTESIAN_POINT('Ctrl Pts',(2.91771087913327,1.44251232660216,2.00434113829285));
#104430=CARTESIAN_POINT('Ctrl Pts',(0.36795895656849,3.23395698461494,2.16323307377672));
#104431=CARTESIAN_POINT('Ctrl Pts',(-2.51906962518594,2.06110744470182,
2.32212500926059));
#104432=CARTESIAN_POINT('Ctrl Pts',(-3.09707945431668,-1.00098657592543,
2.48101694474447));
#104433=CARTESIAN_POINT('Ctrl Pts',(-0.836257356622319,-3.14556004679618,
2.63990888022834));
#104434=CARTESIAN_POINT('Ctrl Pts',(2.1910913679718,-2.40686385398051,2.79880081571221));
#104435=CARTESIAN_POINT('Ctrl Pts',(3.21005123622639,0.538001811857031,
2.95769275119608));
#104436=CARTESIAN_POINT('Ctrl Pts',(1.28662753697526,2.98972646904068,3.11658468667995));
#104437=CARTESIAN_POINT('Ctrl Pts',(-1.81613923385632,2.70102076137102,
3.27547662216383));
#104438=CARTESIAN_POINT('Ctrl Pts',(-3.25420416327164,-0.063483164278144,
3.43436855764768));
#104439=CARTESIAN_POINT('Ctrl Pts',(-1.70941426718082,-2.76979741114071,
3.59326049313157));
#104440=CARTESIAN_POINT('Ctrl Pts',(1.40225168635204,-2.93727170294948,
3.75215242861543));
#104441=CARTESIAN_POINT('Ctrl Pts',(3.22859164459082,-0.412396456472955,
3.91104436409931));
#104442=CARTESIAN_POINT('Ctrl Pts',(2.095553617163,2.49048788012811,4.06993629958317));
#104443=CARTESIAN_POINT('Ctrl Pts',(-0.958301882433825,3.11055177540303,
4.22882823506705));
#104444=CARTESIAN_POINT('Ctrl Pts',(-3.13376277341917,0.879434889337815,
4.38772017055092));
#104445=CARTESIAN_POINT('Ctrl Pts',(-2.43676731682029,-2.15778587635696,
4.54661210603478));
#104446=CARTESIAN_POINT('Ctrl Pts',(0.493807466843058,-3.21714610026924,
4.70550404151867));
#104447=CARTESIAN_POINT('Ctrl Pts',(2.97175054379318,-1.32761950503133,
4.86439597700252));
#104448=CARTESIAN_POINT('Ctrl Pts',(2.72574023624785,1.77882405233552,5.0232879124864));
#104449=CARTESIAN_POINT('Ctrl Pts',(-0.0187265306618801,3.25476944832535,
5.18217984797027));
#104450=CARTESIAN_POINT('Ctrl Pts',(-2.74602826443034,1.74734187142485,
5.34107178345415));
#104451=CARTESIAN_POINT('Ctrl Pts',(-2.95627721245081,-1.36172680366859,
5.49996371893801));
#104452=CARTESIAN_POINT('Ctrl Pts',(-0.456755875356298,-3.22261522912952,
5.65885565442189));
#104453=CARTESIAN_POINT('Ctrl Pts',(2.46143509575639,-2.12960374578606,
5.81774758990576));
#104454=CARTESIAN_POINT('Ctrl Pts',(3.12343586483733,0.915436094402749,
5.97663952538962));
#104455=CARTESIAN_POINT('Ctrl Pts',(0.922446093534211,3.12137278280112,
6.13553146087351));
#104456=CARTESIAN_POINT('Ctrl Pts',(-2.12407230524417,2.46620998432462,
6.29442339635736));
#104457=CARTESIAN_POINT('Ctrl Pts',(-3.22363255275512,-0.449519754299316,
6.45331533184125));
#104458=CARTESIAN_POINT('Ctrl Pts',(-1.36836039659416,-2.95321260151052,
6.6122072673251));
#104459=CARTESIAN_POINT('Ctrl Pts',(1.74117246502532,-2.74994423429374,
6.77109920280899));
#104460=CARTESIAN_POINT('Ctrl Pts',(3.25471920358593,-0.0260336416356283,
6.92999113829285));
#104461=CARTESIAN_POINT('Ctrl Pts',(1.78493902438429,2.72173979724695,7.08888307377672));
#104462=CARTESIAN_POINT('Ctrl Pts',(-1.32094439596421,2.97472364219914,
7.2477750092606));
#104463=CARTESIAN_POINT('Ctrl Pts',(-3.21602936432787,0.501028913805074,
7.40666694474447));
#104464=CARTESIAN_POINT('Ctrl Pts',(-2.16325113136153,-2.43191681341095,
7.56555888022833));
#104465=CARTESIAN_POINT('Ctrl Pts',(0.872397182366315,-3.13572926141387,
7.72445081571221));
#104466=CARTESIAN_POINT('Ctrl Pts',(3.10839248938752,-0.965282847981423,
7.88334275119608));
#104467=CARTESIAN_POINT('Ctrl Pts',(2.49518625105183,2.08995703717797,8.04223468667995));
#104468=CARTESIAN_POINT('Ctrl Pts',(-0.405147030191767,3.22950936345052,
8.20112662216383));
#104469=CARTESIAN_POINT('Ctrl Pts',(-2.93411615827254,1.40884250874675,
8.36001855764769));
#104470=CARTESIAN_POINT('Ctrl Pts',(-2.77362817276533,-1.70319159342991,
8.51891049313157));
#104471=CARTESIAN_POINT('Ctrl Pts',(-0.0707888905447793,-3.25405343804665,
8.67780242861544));
#104472=CARTESIAN_POINT('Ctrl Pts',(2.69693660441204,-1.82219861608723,
8.8366943640993));
#104473=CARTESIAN_POINT('Ctrl Pts',(2.99260750289983,1.27991217600095,8.99558629958318));
#104474=CARTESIAN_POINT('Ctrl Pts',(0.545207199465845,3.20883529560781,
9.15447823506705));
#104475=CARTESIAN_POINT('Ctrl Pts',(-2.40193861569527,2.19648941065502,
9.31337017055092));
#104476=CARTESIAN_POINT('Ctrl Pts',(-3.14742964013857,-0.829193285709043,
9.47226210603479));
#104477=CARTESIAN_POINT('Ctrl Pts',(-1.00793705160453,-3.09482434795427,
9.63115404151866));
#104478=CARTESIAN_POINT('Ctrl Pts',(2.05544652394575,-2.52369063712,9.79004597700253));
#104479=CARTESIAN_POINT('Ctrl Pts',(3.23477542093817,0.360697686133515,
9.94893791248641));
#104480=CARTESIAN_POINT('Ctrl Pts',(1.44905818566578,2.91446482552848,10.1078298479703));
#104481=CARTESIAN_POINT('Ctrl Pts',(-1.66488862035959,2.79678757264204,
10.2667217834542));
#104482=CARTESIAN_POINT('Ctrl Pts',(-3.25277227761243,0.115530752113285,
10.425613718938));
#104483=CARTESIAN_POINT('Ctrl Pts',(-1.85911360013471,-2.67162337661616,
10.5845056544219));
#104484=CARTESIAN_POINT('Ctrl Pts',(1.23863790364548,-3.00992541242147,
10.7433975899058));
#104485=CARTESIAN_POINT('Ctrl Pts',(3.20103438348542,-0.589282377499889,
10.9022895253897));
#104486=CARTESIAN_POINT('Ctrl Pts',(2.2293122977628,2.37150617197835,11.0611814608735));
#104487=CARTESIAN_POINT('Ctrl Pts',(-0.78583257499675,3.15853478827791,
11.2200733963574));
#104488=CARTESIAN_POINT('Ctrl Pts',(-3.08067092445951,1.05040063779377,
11.3789653318413));
#104489=CARTESIAN_POINT('Ctrl Pts',(-2.55171775188206,-2.02054729205179,
11.5378572673251));
#104490=CARTESIAN_POINT('Ctrl Pts',(0.316180128224772,-3.23942972932021,
11.696749202809));
#104491=CARTESIAN_POINT('Ctrl Pts',(2.89426231966781,-1.48899982190694,
11.8556411382929));
#104492=CARTESIAN_POINT('Ctrl Pts',(2.81941805410138,1.62627078953506,12.0145330737768));
#104493=CARTESIAN_POINT('Ctrl Pts',(0.160250764921038,3.25087596457171,
12.1734250092606));
#104494=CARTESIAN_POINT('Ctrl Pts',(-2.64580490100596,1.89567699529763,
12.3323169447445));
#104495=CARTESIAN_POINT('Ctrl Pts',(-3.02667409566324,-1.19712938453989,
12.4912088802284));
#104496=CARTESIAN_POINT('Ctrl Pts',(-0.633246112567888,-3.19262810324119,
12.6501008157122));
#104497=CARTESIAN_POINT('Ctrl Pts',(2.34062523753456,-2.26171358533835,
12.8089927511961));
#104498=CARTESIAN_POINT('Ctrl Pts',(3.16904260566617,0.74232325045119,12.96788468668));
#104499=CARTESIAN_POINT('Ctrl Pts',(1.09266557598831,3.06593489554784,13.1267766221638));
#104500=CARTESIAN_POINT('Ctrl Pts',(-1.98526594151343,2.57926229495074,
13.2856685576477));
#104501=CARTESIAN_POINT('Ctrl Pts',(-3.24347140839053,-0.27160277546613,
13.4445604931316));
#104502=CARTESIAN_POINT('Ctrl Pts',(-1.52865986385155,-2.87351246131581,
13.6034524286155));
#104503=CARTESIAN_POINT('Ctrl Pts',(1.58734540422173,-2.84151533734801,
13.7623443640993));
#104504=CARTESIAN_POINT('Ctrl Pts',(3.24836485754839,-0.204940471679879,
13.9212362995832));
#104505=CARTESIAN_POINT('Ctrl Pts',(1.93188188683804,2.61948606027878,14.0801282350671));
#104506=CARTESIAN_POINT('Ctrl Pts',(-1.15539446862615,3.04285038517439,
14.2390201705509));
#104507=CARTESIAN_POINT('Ctrl Pts',(-3.18361804464065,0.677090090406219,
14.3979121060348));
#104508=CARTESIAN_POINT('Ctrl Pts',(-2.29368714576657,-2.30930165245534,
14.5568040415187));
#104509=CARTESIAN_POINT('Ctrl Pts',(0.698673540399568,-3.17895110510264,
14.7156959770026));
#104510=CARTESIAN_POINT('Ctrl Pts',(3.05061904804408,-1.13472387319489,
14.8745879124864));
#104511=CARTESIAN_POINT('Ctrl Pts',(2.60631905720107,1.94960914461292,15.0334798479703));
#104512=CARTESIAN_POINT('Ctrl Pts',(-0.226974058166443,3.24689969380135,
15.1923717834542));
#104513=CARTESIAN_POINT('Ctrl Pts',(-2.85221917461115,1.56803081113487,
15.351263718938));
#104514=CARTESIAN_POINT('Ctrl Pts',(-2.86307524342312,-1.54811982584858,
15.5101556544219));
#104515=CARTESIAN_POINT('Ctrl Pts',(-0.249591420833051,-3.24523943143405,
15.6690475899058));
#104516=CARTESIAN_POINT('Ctrl Pts',(2.59267183175928,-1.96772142781691,
15.8279395253897));
#104517=CARTESIAN_POINT('Ctrl Pts',(3.0584512217531,1.11344104866165,15.9868314608735));
#104518=CARTESIAN_POINT('Ctrl Pts',(0.720806019399342,3.17400591163366,
16.1457233963574));
#104519=CARTESIAN_POINT('Ctrl Pts',(-2.27754134054451,2.32522693232264,
16.3046153318412));
#104520=CARTESIAN_POINT('Ctrl Pts',(-3.18825841272756,-0.654891699718197,
16.4635072673252));
#104521=CARTESIAN_POINT('Ctrl Pts',(-1.1765675754994,-3.03472627842632,
16.622399202809));
#104522=CARTESIAN_POINT('Ctrl Pts',(1.9135836446356,-2.63288292175533,16.7812911382929));
#104523=CARTESIAN_POINT('Ctrl Pts',(3.24971393720761,0.182302416348347,
16.9401830737767));
#104524=CARTESIAN_POINT('Ctrl Pts',(1.60710521806487,2.83038648646373,17.0990750092606));
#104525=CARTESIAN_POINT('Ctrl Pts',(-1.50860147261613,2.88409369499471,
17.2579669447445));
#104526=CARTESIAN_POINT('Ctrl Pts',(-3.24150027729799,0.294195168153433,
17.4168588802284));
#104527=CARTESIAN_POINT('Ctrl Pts',(-2.00318884038906,-2.56536728645793,
17.5757508157122));
#104528=CARTESIAN_POINT('Ctrl Pts',(1.07127705872643,-3.07347365502525,
17.7346427511961));
#104529=CARTESIAN_POINT('Ctrl Pts',(3.16379352203233,-0.764385632147803,
17.89353468668));
#104530=CARTESIAN_POINT('Ctrl Pts',(2.35632698031541,2.2453503081982,18.0524266221638));
#104531=CARTESIAN_POINT('Ctrl Pts',(-0.610986008271525,3.19696276837624,
18.2113185576477));
#104532=CARTESIAN_POINT('Ctrl Pts',(-3.01825959227787,1.21818876957141,
18.3702104931316));
#104533=CARTESIAN_POINT('Ctrl Pts',(-2.65894886495122,-1.87719625459478,
18.5291024286155));
#104534=CARTESIAN_POINT('Ctrl Pts',(0.137596298152765,-3.25191360638933,
18.6879943640993));
#104535=CARTESIAN_POINT('Ctrl Pts',(2.80801852579208,-1.64587569503084,
18.8468862995832));
#104536=CARTESIAN_POINT('Ctrl Pts',(2.90456671713063,1.4687978180947,19.0057782350671));
#104537=CARTESIAN_POINT('Ctrl Pts',(0.338743278337104,3.23714810227294,
19.164670170551));
#104538=CARTESIAN_POINT('Ctrl Pts',(-2.53757758810555,2.03827741709,19.3235621060348));
#104539=CARTESIAN_POINT('Ctrl Pts',(-3.0879148440151,-1.02891047273259,
19.4824540415187));
#104540=CARTESIAN_POINT('Ctrl Pts',(-0.80782068700727,-3.15298280714823,
19.6413459770026));
#104541=CARTESIAN_POINT('Ctrl Pts',(2.21273464322184,-2.38698140825151,
19.8002379124864));
#104542=CARTESIAN_POINT('Ctrl Pts',(3.20506252600188,0.566964769414809,
19.9591298479703));
#104543=CARTESIAN_POINT('Ctrl Pts',(1.25957958398902,3.00122210358845,20.1180217834542));
#104544=CARTESIAN_POINT('Ctrl Pts',(-1.84045385561639,2.68451195754086,
20.276913718938));
#104545=CARTESIAN_POINT('Ctrl Pts',(-3.25349828597628,-0.0928641587167671,
20.4358056544219));
#104546=CARTESIAN_POINT('Ctrl Pts',(-1.68433490870969,-2.78511952183474,
20.5946975899058));
#104547=CARTESIAN_POINT('Ctrl Pts',(1.42871638753743,-2.9244904397832,20.7535895253897));
#104548=CARTESIAN_POINT('Ctrl Pts',(3.23218373376165,-0.38322732329028,
20.9124814608735));
#104549=CARTESIAN_POINT('Ctrl Pts',(2.07298051381926,2.50930798586206,21.0713733963574));
#104550=CARTESIAN_POINT('Ctrl Pts',(-0.986349287101606,3.10177206973596,
21.2302653318412));
#104551=CARTESIAN_POINT('Ctrl Pts',(-3.14157584161525,0.851102946639152,
21.3891572673252));
#104552=CARTESIAN_POINT('Ctrl Pts',(-2.41718436132387,-2.17970046976106,
21.548049202809));
#104553=CARTESIAN_POINT('Ctrl Pts',(0.522836198430219,-3.21255623781816,
21.7069411382929));
#104554=CARTESIAN_POINT('Ctrl Pts',(2.98361724412315,-1.30073203070833,
21.8658330737767));
#104555=CARTESIAN_POINT('Ctrl Pts',(2.70956696485005,1.80336309018792,22.0247250092606));
#104556=CARTESIAN_POINT('Ctrl Pts',(-0.0481136935684708,3.254468260577,
22.1836169447445));
#104557=CARTESIAN_POINT('Ctrl Pts',(-2.76169526361428,1.72247447051088,
22.3425088802284));
#104558=CARTESIAN_POINT('Ctrl Pts',(-2.94385831113143,-1.38836263204452,
22.5014008157122));
#104559=CARTESIAN_POINT('Ctrl Pts',(-0.427644204365768,-3.22661217441425,
22.6602927511961));
#104560=CARTESIAN_POINT('Ctrl Pts',(2.48057396950494,-2.10728381055163,
22.8191846866799));
#104561=CARTESIAN_POINT('Ctrl Pts',(3.11502334931318,0.943586743892659,
22.9780766221639));
#104562=CARTESIAN_POINT('Ctrl Pts',(0.894261184887878,3.12960304662157,
23.1369685576477));
#104563=CARTESIAN_POINT('Ctrl Pts',(-2.14632458448094,2.44687617640059,
23.2958604931316));
#104564=CARTESIAN_POINT('Ctrl Pts',(-3.21930781471386,-0.47850565449158,
23.4547524286154));
#104565=CARTESIAN_POINT('Ctrl Pts',(-1.34189544060237,-2.96564494987165,
23.6136443640994));
#104566=CARTESIAN_POINT('Ctrl Pts',(1.76642218227432,-2.73373365138718,
23.7725362995832));
#104567=CARTESIAN_POINT('Ctrl Pts',(3.25388197267903,0.00263476266896457,
23.9314282350671));
#104568=CARTESIAN_POINT('Ctrl Pts',(1.76211703029526,2.73913811890468,24.0903201705509));
#104569=CARTESIAN_POINT('Ctrl Pts',(-1.35203650566515,2.95991020239352,
24.2492381724761));
#104570=CARTESIAN_POINT('Ctrl Pts',(-2.5917161935483,1.3048806588596,24.3551921959067));
#104571=CARTESIAN_POINT('Ctrl Pts',(-2.72415204890299,0.397871481308887,
24.4081822408425));
#104572=CARTESIAN_POINT('Ctrl Pts',(1.48546006159232,-2.08528497081503,
-0.108922561569808));
#104573=CARTESIAN_POINT('Ctrl Pts',(2.17977177658322,-1.59072995968249,
-0.0559326049298234));
#104574=CARTESIAN_POINT('Ctrl Pts',(3.02309439754947,0.137523069098973,
0.0500213302047839));
#104575=CARTESIAN_POINT('Ctrl Pts',(1.51865255465809,2.62069173036942,0.208939243834015));
#104576=CARTESIAN_POINT('Ctrl Pts',(-1.37888567991209,2.69361335216517,
0.367831179317886));
#104577=CARTESIAN_POINT('Ctrl Pts',(-3.01182090579545,0.301368262920637,
0.526723114801757));
#104578=CARTESIAN_POINT('Ctrl Pts',(-1.88443786280079,-2.3691080193925,
0.685615050285628));
#104579=CARTESIAN_POINT('Ctrl Pts',(0.970441480757242,-2.86698113346493,
0.844506985769499));
#104580=CARTESIAN_POINT('Ctrl Pts',(2.93569887827138,-0.737479474983559,
1.00339892125337));
#104581=CARTESIAN_POINT('Ctrl Pts',(2.21010079966783,2.0682931465622,1.16229085673724));
#104582=CARTESIAN_POINT('Ctrl Pts',(-0.54133794690907,2.97808602748199,
1.32118279222111));
#104583=CARTESIAN_POINT('Ctrl Pts',(-2.79656342279512,1.15819671584495,
1.48007472770498));
#104584=CARTESIAN_POINT('Ctrl Pts',(-2.48842232209177,-1.72335502950263,
1.63896666318885));
#104585=CARTESIAN_POINT('Ctrl Pts',(0.100649843392986,-3.02523087800956,
1.79785859867272));
#104586=CARTESIAN_POINT('Ctrl Pts',(2.59746270902568,-1.55414369665589,
1.95675053415659));
#104587=CARTESIAN_POINT('Ctrl Pts',(2.7134014013754,1.3415019961355,2.11564246964046));
#104588=CARTESIAN_POINT('Ctrl Pts',(0.342193037542567,3.00750272304177,
2.27453440512433));
#104589=CARTESIAN_POINT('Ctrl Pts',(-2.3426745603979,1.91678067516427,2.4334263406082));
#104590=CARTESIAN_POINT('Ctrl Pts',(-2.8802098904365,-0.930893597888221,
2.59231827609208));
#104591=CARTESIAN_POINT('Ctrl Pts',(-0.77769936000087,-2.92529568303992,
2.75121021157595));
#104592=CARTESIAN_POINT('Ctrl Pts',(2.03766261795009,-2.23832587423829,
2.91010214705982));
#104593=CARTESIAN_POINT('Ctrl Pts',(2.98527094824794,0.500328829931562,
3.06899408254369));
#104594=CARTESIAN_POINT('Ctrl Pts',(1.1965328665169,2.78037417923805,3.22788601802756));
#104595=CARTESIAN_POINT('Ctrl Pts',(-1.68896609238486,2.51188476948248,
3.38677795351144));
#104596=CARTESIAN_POINT('Ctrl Pts',(-3.0263321154034,-0.059037825902474,
3.5456698889953));
#104597=CARTESIAN_POINT('Ctrl Pts',(-1.58971442347893,-2.57584541040876,
3.70456182447918));
#104598=CARTESIAN_POINT('Ctrl Pts',(1.30406056269662,-2.73159250013523,
3.86345375996304));
#104599=CARTESIAN_POINT('Ctrl Pts',(3.00251308501958,-0.383518850657475,
4.02234569544692));
#104600=CARTESIAN_POINT('Ctrl Pts',(1.94881479249118,2.31609422043059,4.18123763093079));
#104601=CARTESIAN_POINT('Ctrl Pts',(-0.891197852855459,2.89273882713716,
4.34012956641466));
#104602=CARTESIAN_POINT('Ctrl Pts',(-2.91432450068511,0.81785343373588,
4.49902150189853));
#104603=CARTESIAN_POINT('Ctrl Pts',(-2.26613538016149,-2.00668930655468,
4.6579134373824));
#104604=CARTESIAN_POINT('Ctrl Pts',(0.459229145054833,-2.99186900228206,
4.81680537286627));
#104605=CARTESIAN_POINT('Ctrl Pts',(2.7636569982773,-1.23465441734085,4.97569730835014));
#104606=CARTESIAN_POINT('Ctrl Pts',(2.53487329046712,1.65426386518503,5.13458924383401));
#104607=CARTESIAN_POINT('Ctrl Pts',(-0.0174152260610237,3.02685781699636,
5.29348117931788));
#104608=CARTESIAN_POINT('Ctrl Pts',(-2.55374067191164,1.62498618917805,
5.45237311480176));
#104609=CARTESIAN_POINT('Ctrl Pts',(-2.749267169851,-1.26637339010859,5.61126505028562));
#104610=CARTESIAN_POINT('Ctrl Pts',(-0.424772050288417,-2.99695516144193,
5.7701569857695));
#104611=CARTESIAN_POINT('Ctrl Pts',(2.28907582515644,-1.98048059851179,
5.92904892125336));
#104612=CARTESIAN_POINT('Ctrl Pts',(2.90472072245671,0.851333694228085,
6.08794085673724));
#104613=CARTESIAN_POINT('Ctrl Pts',(0.857852825922402,2.90280210545861,
6.24683279222111));
#104614=CARTESIAN_POINT('Ctrl Pts',(-1.97533649097687,2.29351635743302,
6.40572472770499));
#104615=CARTESIAN_POINT('Ctrl Pts',(-2.99790124810567,-0.418042630606353,
6.56461666318884));
#104616=CARTESIAN_POINT('Ctrl Pts',(-1.27254247302535,-2.74641715490278,
6.72350859867273));
#104617=CARTESIAN_POINT('Ctrl Pts',(1.61924878863919,-2.55738243031585,
6.88240053415659));
#104618=CARTESIAN_POINT('Ctrl Pts',(3.02681109058924,-0.0242106646694371,
7.04129246964047));
#104619=CARTESIAN_POINT('Ctrl Pts',(1.65995064307836,2.53115297778335,7.20018440512434));
#104620=CARTESIAN_POINT('Ctrl Pts',(-1.22844672540447,2.7664219087552,7.3590763406082));
#104621=CARTESIAN_POINT('Ctrl Pts',(-2.99083046454003,0.465944918179204,
7.51796827609208));
#104622=CARTESIAN_POINT('Ctrl Pts',(-2.01177186312133,-2.26162452788943,
7.67686021157594));
#104623=CARTESIAN_POINT('Ctrl Pts',(0.811308534412381,-2.91615328753264,
7.83575214705982));
#104624=CARTESIAN_POINT('Ctrl Pts',(2.89073074273702,-0.897689984010518,
7.9946440825437));
#104625=CARTESIAN_POINT('Ctrl Pts',(2.32046359312609,1.94361010683061,8.15353601802756));
#104626=CARTESIAN_POINT('Ctrl Pts',(-0.376777057434817,3.00336654163099,
8.31242795351144));
#104627=CARTESIAN_POINT('Ctrl Pts',(-2.72865791898473,1.31018987004163,
8.4713198889953));
#104628=CARTESIAN_POINT('Ctrl Pts',(-2.57940792718688,-1.58392748557606,
8.63021182447918));
#104629=CARTESIAN_POINT('Ctrl Pts',(-0.0658319767663575,-3.02619194454561,
8.78910375996304));
#104630=CARTESIAN_POINT('Ctrl Pts',(2.50808660109806,-1.69460117307586,
8.94799569544693));
#104631=CARTESIAN_POINT('Ctrl Pts',(2.78305347188721,1.19028774126861,9.10688763093078));
#104632=CARTESIAN_POINT('Ctrl Pts',(0.507029668241175,2.98414015252653,
9.26577956641467));
#104633=CARTESIAN_POINT('Ctrl Pts',(-2.23374552031738,2.04268266866388,
9.42467150189852));
#104634=CARTESIAN_POINT('Ctrl Pts',(-2.92703436017603,-0.771129942841463,
9.58356343738241));
#104635=CARTESIAN_POINT('Ctrl Pts',(-0.93735737419411,-2.87811269540331,
9.74245537286627));
#104636=CARTESIAN_POINT('Ctrl Pts',(1.911516154124,-2.34697199108145,9.90134730835015));
#104637=CARTESIAN_POINT('Ctrl Pts',(3.00826384926654,0.335440229539894,
10.060239243834));
#104638=CARTESIAN_POINT('Ctrl Pts',(1.34758948865696,2.71038264908462,10.2191311793179));
#104639=CARTESIAN_POINT('Ctrl Pts',(-1.54830663583761,2.60094561569807,
10.3780231148017));
#104640=CARTESIAN_POINT('Ctrl Pts',(-3.02500049595403,0.10744083895636,
10.5369150502856));
#104641=CARTESIAN_POINT('Ctrl Pts',(-1.72893122618789,-2.48454590408593,
10.6958069857695));
#104642=CARTESIAN_POINT('Ctrl Pts',(1.15190365419162,-2.79915871394563,
10.8546989212533));
#104643=CARTESIAN_POINT('Ctrl Pts',(2.97688549064886,-0.548018530673967,
11.0135908567372));
#104644=CARTESIAN_POINT('Ctrl Pts',(2.07320716939916,2.20544407481798,11.1724827922211));
#104645=CARTESIAN_POINT('Ctrl Pts',(-0.730805517946308,2.93736188259754,
11.331374727705));
#104646=CARTESIAN_POINT('Ctrl Pts',(-2.86495034973719,0.976847494718856,
11.4902666631888));
#104647=CARTESIAN_POINT('Ctrl Pts',(-2.37303653812609,-1.87906070235006,
11.6491585986727));
#104648=CARTESIAN_POINT('Ctrl Pts',(0.294039964393921,-3.0125922448511,
11.8080505341566));
#104649=CARTESIAN_POINT('Ctrl Pts',(2.69159480135589,-1.38473425598983,
11.9669424696404));
#104650=CARTESIAN_POINT('Ctrl Pts',(2.62199142271915,1.51239297591101,12.1258344051243));
#104651=CARTESIAN_POINT('Ctrl Pts',(0.149029382320921,3.02323697013694,
12.2847263406082));
#104652=CARTESIAN_POINT('Ctrl Pts',(-2.46053533867895,1.76293431003818,
12.4436182760921));
#104653=CARTESIAN_POINT('Ctrl Pts',(-2.81473458916494,-1.11330172323418,
12.6025102115759));
#104654=CARTESIAN_POINT('Ctrl Pts',(-0.588903753811167,-2.96906785088264,
12.7614021470598));
#104655=CARTESIAN_POINT('Ctrl Pts',(2.1767255436589,-2.10333959264322,12.9202940825437));
#104656=CARTESIAN_POINT('Ctrl Pts',(2.94713390169327,0.690342885737227,
13.0791860180275));
#104657=CARTESIAN_POINT('Ctrl Pts',(1.01615287735504,2.85124619495422,13.2380779535114));
#104658=CARTESIAN_POINT('Ctrl Pts',(-1.84624988936723,2.39865230502655,
13.3969698889953));
#104659=CARTESIAN_POINT('Ctrl Pts',(-3.01635090981402,-0.252584091466298,
13.5558618244792));
#104660=CARTESIAN_POINT('Ctrl Pts',(-1.42161714735535,-2.67229792888874,
13.714753759963));
#104661=CARTESIAN_POINT('Ctrl Pts',(1.47619329765856,-2.64254136814274,
13.8736456954469));
#104662=CARTESIAN_POINT('Ctrl Pts',(3.02090170060603,-0.190589741784131,
14.0325376309308));
#104663=CARTESIAN_POINT('Ctrl Pts',(1.79660399408569,2.43605944566898,14.1914295664146));
#104664=CARTESIAN_POINT('Ctrl Pts',(-1.0744892486547,2.82977815189164,14.3503215018985));
#104665=CARTESIAN_POINT('Ctrl Pts',(-2.96068871167182,0.629677605586279,
14.5092134373824));
#104666=CARTESIAN_POINT('Ctrl Pts',(-2.13307423986045,-2.14759535798565,
14.6681053728662));
#104667=CARTESIAN_POINT('Ctrl Pts',(0.649749698361895,-2.95634856941403,
14.8269973083501));
#104668=CARTESIAN_POINT('Ctrl Pts',(2.83700282273485,-1.05526608880994,
14.985889243834));
#104669=CARTESIAN_POINT('Ctrl Pts',(2.42381444742106,1.81308992023858,15.1447811793179));
#104670=CARTESIAN_POINT('Ctrl Pts',(-0.21108045074281,3.01953913333011,
15.3036731148017));
#104671=CARTESIAN_POINT('Ctrl Pts',(-2.65249568103837,1.45823118759357,
15.4625650502856));
#104672=CARTESIAN_POINT('Ctrl Pts',(-2.66259156563698,-1.43971444703336,
15.6214569857695));
#104673=CARTESIAN_POINT('Ctrl Pts',(-0.232114057600147,-3.01799512899908,
15.7803489212533));
#104674=CARTESIAN_POINT('Ctrl Pts',(2.41112285384901,-1.82993391084071,
15.9392408567372));
#104675=CARTESIAN_POINT('Ctrl Pts',(2.84428655714113,1.03547357052898,16.0981327922211));
#104676=CARTESIAN_POINT('Ctrl Pts',(0.670332374994958,2.95174965764906,
16.257024727705));
#104677=CARTESIAN_POINT('Ctrl Pts',(-2.11805902679419,2.16240548774123,
16.4159166631888));
#104678=CARTESIAN_POINT('Ctrl Pts',(-2.96500414311501,-0.609033632658046,
16.5748085986727));
#104679=CARTESIAN_POINT('Ctrl Pts',(-1.09417973213347,-2.82222292673453,
16.7337005341566));
#104680=CARTESIAN_POINT('Ctrl Pts',(1.77958706605832,-2.44851820673558,
16.8925924696404));
#104681=CARTESIAN_POINT('Ctrl Pts',(3.02215631245399,0.169536891242848,
17.0514844051243));
#104682=CARTESIAN_POINT('Ctrl Pts',(1.49456945238876,2.63219180273477,17.2103763406082));
#104683=CARTESIAN_POINT('Ctrl Pts',(-1.40296332278459,2.68213822338054,
17.3692682760921));
#104684=CARTESIAN_POINT('Ctrl Pts',(-3.01451780499646,0.273594476839516,
17.5281602115759));
#104685=CARTESIAN_POINT('Ctrl Pts',(-1.86291775706917,-2.38573027913763,
17.6870521470598));
#104686=CARTESIAN_POINT('Ctrl Pts',(0.996262067361875,-2.85825706113596,
17.8459440825436));
#104687=CARTESIAN_POINT('Ctrl Pts',(2.94225237933618,-0.710860373553265,
18.0048360180275));
#104688=CARTESIAN_POINT('Ctrl Pts',(2.19132778926533,2.08812213588945,18.1637279535114));
#104689=CARTESIAN_POINT('Ctrl Pts',(-0.568202388701774,2.97309898588511,
18.3226198889953));
#104690=CARTESIAN_POINT('Ctrl Pts',(-2.80690930207393,1.13288644811743,
18.4815118244792));
#104691=CARTESIAN_POINT('Ctrl Pts',(-2.47275891108423,-1.74574766276608,
18.640403759963));
#104692=CARTESIAN_POINT('Ctrl Pts',(0.127961269535608,-3.02420195223377,
18.7992956954469));
#104693=CARTESIAN_POINT('Ctrl Pts',(2.61139013377353,-1.53062506957956,
18.9581876309307));
#104694=CARTESIAN_POINT('Ctrl Pts',(2.7011776447815,1.36594687515411,19.1170795664147));
#104695=CARTESIAN_POINT('Ctrl Pts',(0.315023154871148,3.01047038621467,
19.2759715018985));
#104696=CARTESIAN_POINT('Ctrl Pts',(-2.35988652368112,1.89554929498936,
19.4348634373824));
#104697=CARTESIAN_POINT('Ctrl Pts',(-2.8716870218366,-0.956862154701133,
19.5937553728662));
#104698=CARTESIAN_POINT('Ctrl Pts',(-0.751253936728898,-2.9321986728068,
19.7526473083501));
#104699=CARTESIAN_POINT('Ctrl Pts',(2.057790346785,-2.21983567478444,19.911539243834));
#104700=CARTESIAN_POINT('Ctrl Pts',(2.98063156694013,0.527263688415071,
20.0704311793178));
#104701=CARTESIAN_POINT('Ctrl Pts',(1.17137891652752,2.79106484468908,20.2293231148018));
#104702=CARTESIAN_POINT('Ctrl Pts',(-1.71157810964454,2.49653197638425,
20.3882150502856));
#104703=CARTESIAN_POINT('Ctrl Pts',(-3.02567566638506,-0.0863614486965333,
20.5471069857695));
#104704=CARTESIAN_POINT('Ctrl Pts',(-1.56639121935072,-2.59009460724541,
20.7059989212533));
#104705=CARTESIAN_POINT('Ctrl Pts',(1.32867210244754,-2.719706230788,20.8648908567372));
#104706=CARTESIAN_POINT('Ctrl Pts',(3.00585364211853,-0.356392253769203,
21.0237827922211));
#104707=CARTESIAN_POINT('Ctrl Pts',(1.92782234574661,2.33359646907276,21.182674727705));
#104708=CARTESIAN_POINT('Ctrl Pts',(-0.91728126902763,2.88457391065039,
21.3415666631888));
#104709=CARTESIAN_POINT('Ctrl Pts',(-2.92159046742086,0.791505403993785,
21.5004585986727));
#104710=CARTESIAN_POINT('Ctrl Pts',(-2.24792369946788,-2.02706935478992,
21.6593505341566));
#104711=CARTESIAN_POINT('Ctrl Pts',(0.486225171814051,-2.98760053987341,
21.8182424696404));
#104712=CARTESIAN_POINT('Ctrl Pts',(2.77469274603948,-1.20964970867379,
21.9771344051243));
#104713=CARTESIAN_POINT('Ctrl Pts',(2.51983253451372,1.67708458404834,22.1360263406082));
#104714=CARTESIAN_POINT('Ctrl Pts',(-0.0447445853828995,3.02657771958701,
22.2949182760921));
#104715=CARTESIAN_POINT('Ctrl Pts',(-2.56831060680309,1.60186010051345,
22.4538102115759));
#104716=CARTESIAN_POINT('Ctrl Pts',(-2.73771788836306,-1.29114407405777,
22.6127021470598));
#104717=CARTESIAN_POINT('Ctrl Pts',(-0.397698891865832,-3.00067222505312,
22.7715940825436));
#104718=CARTESIAN_POINT('Ctrl Pts',(2.3068745204355,-1.95972359205962,22.9304860180276));
#104719=CARTESIAN_POINT('Ctrl Pts',(2.89689728402915,0.877513125617889,
23.0893779535114));
#104720=CARTESIAN_POINT('Ctrl Pts',(0.831641534335725,2.91045605415649,
23.2482698889953));
#104721=CARTESIAN_POINT('Ctrl Pts',(-1.9960305789678,2.27553637802856,23.4071618244792));
#104722=CARTESIAN_POINT('Ctrl Pts',(-2.99387934506323,-0.44499882519174,
23.566053759963));
#104723=CARTESIAN_POINT('Ctrl Pts',(-1.24793069631059,-2.75797894181825,
23.7249456954469));
#104724=CARTESIAN_POINT('Ctrl Pts',(1.64273042236025,-2.54230697555083,
23.8838376309308));
#104725=CARTESIAN_POINT('Ctrl Pts',(3.02603248585074,0.00245026632671095,
24.0427295664146));
#104726=CARTESIAN_POINT('Ctrl Pts',(1.63872673388769,2.54733300120695,24.2016215018985));
#104727=CARTESIAN_POINT('Ctrl Pts',(-1.25736164450683,2.75264576369051,
24.3605395038237));
#104728=CARTESIAN_POINT('Ctrl Pts',(-2.41023413314696,1.21350783372652,
24.4664935272542));
#104729=CARTESIAN_POINT('Ctrl Pts',(-2.53339631418477,0.370010970816811,
24.5194835721902));
#104730=CARTESIAN_POINT('Ctrl Pts',(1.37361020065383,-1.92827042694857,
0.00237876977780734));
#104731=CARTESIAN_POINT('Ctrl Pts',(2.01564271219955,-1.47095364971531,
0.0553687264177913));
#104732=CARTESIAN_POINT('Ctrl Pts',(2.79546613832361,0.127168070972611,
0.161322661552399));
#104733=CARTESIAN_POINT('Ctrl Pts',(1.40430341701095,2.42336296119994,0.32024057518163));
#104734=CARTESIAN_POINT('Ctrl Pts',(-1.27506049097842,2.49079384415449,
0.479132510665502));
#104735=CARTESIAN_POINT('Ctrl Pts',(-2.78504150041466,0.278676304267241,
0.638024446149372));
#104736=CARTESIAN_POINT('Ctrl Pts',(-1.74254639203617,-2.19072260912893,
0.796916381633244));
#104737=CARTESIAN_POINT('Ctrl Pts',(0.897370687756388,-2.65110764794858,
0.955808317117115));
#104738=CARTESIAN_POINT('Ctrl Pts',(2.71465119090379,-0.681949892698155,
1.11470025260098));
#104739=CARTESIAN_POINT('Ctrl Pts',(2.04368806768372,1.91255802664586,1.27359218808486));
#104740=CARTESIAN_POINT('Ctrl Pts',(-0.500577124287141,2.75384673849052,
1.43248412356873));
#104741=CARTESIAN_POINT('Ctrl Pts',(-2.58599214051509,1.07098862122423,
1.5913760590526));
#104742=CARTESIAN_POINT('Ctrl Pts',(-2.3010529690687,-1.59359252333946,
1.75026799453647));
#104743=CARTESIAN_POINT('Ctrl Pts',(0.0930712680559027,-2.79744174940153,
1.90915993002034));
#104744=CARTESIAN_POINT('Ctrl Pts',(2.4018830025703,-1.43712220220855,2.06805186550421));
#104745=CARTESIAN_POINT('Ctrl Pts',(2.50909192361753,1.24049166566884,2.22694380098809));
#104746=CARTESIAN_POINT('Ctrl Pts',(0.316427118516644,2.78104846146861,
2.38583573647195));
#104747=CARTESIAN_POINT('Ctrl Pts',(-2.16627949560986,1.77245390562672,
2.54472767195583));
#104748=CARTESIAN_POINT('Ctrl Pts',(-2.66334032655633,-0.860800619851015,
2.7036196074397));
#104749=CARTESIAN_POINT('Ctrl Pts',(-0.719141363379423,-2.70503131928368,
2.86251154292357));
#104750=CARTESIAN_POINT('Ctrl Pts',(1.8842338679284,-2.06978789449606,3.02140347840744));
#104751=CARTESIAN_POINT('Ctrl Pts',(2.76049066026949,0.46265584800609,3.18029541389131));
#104752=CARTESIAN_POINT('Ctrl Pts',(1.10643819605854,2.57102188943541,3.33918734937518));
#104753=CARTESIAN_POINT('Ctrl Pts',(-1.56179295091342,2.32274877759393,
3.49807928485906));
#104754=CARTESIAN_POINT('Ctrl Pts',(-2.79846006753516,-0.0545924875268026,
3.65697122034292));
#104755=CARTESIAN_POINT('Ctrl Pts',(-1.47001457977705,-2.38189340967681,
3.8158631558268));
#104756=CARTESIAN_POINT('Ctrl Pts',(1.20586943904121,-2.52591329732098,
3.97475509131066));
#104757=CARTESIAN_POINT('Ctrl Pts',(2.77643452544834,-0.354641244841995,
4.13364702679454));
#104758=CARTESIAN_POINT('Ctrl Pts',(1.80207596781938,2.14170056073307,4.2925389622784));
#104759=CARTESIAN_POINT('Ctrl Pts',(-0.824093823277095,2.6749258788713,
4.45143089776229));
#104760=CARTESIAN_POINT('Ctrl Pts',(-2.69488622795106,0.756271978133945,
4.61032283324614));
#104761=CARTESIAN_POINT('Ctrl Pts',(-2.09550344350268,-1.8555927367524,
4.76921476873002));
#104762=CARTESIAN_POINT('Ctrl Pts',(0.424650823266605,-2.76659190429488,
4.92810670421389));
#104763=CARTESIAN_POINT('Ctrl Pts',(2.55556345276143,-1.14168932965037,
5.08699863969777));
#104764=CARTESIAN_POINT('Ctrl Pts',(2.34400634468638,1.52970367803454,5.24589057518163));
#104765=CARTESIAN_POINT('Ctrl Pts',(-0.0161039214601648,2.79894618566735,
5.40478251066551));
#104766=CARTESIAN_POINT('Ctrl Pts',(-2.36145307939294,1.50263050693126,
5.56367444614937));
#104767=CARTESIAN_POINT('Ctrl Pts',(-2.54225712725118,-1.17101997654861,
5.72256638163325));
#104768=CARTESIAN_POINT('Ctrl Pts',(-0.392788225220536,-2.77129509375434,
5.88145831711711));
#104769=CARTESIAN_POINT('Ctrl Pts',(2.11671655455651,-1.83135745123752,
6.040350252601));
#104770=CARTESIAN_POINT('Ctrl Pts',(2.6860055800761,0.787231294053425,6.19924218808485));
#104771=CARTESIAN_POINT('Ctrl Pts',(0.7932595583106,2.68423142811611,6.35813412356874));
#104772=CARTESIAN_POINT('Ctrl Pts',(-1.82660067670958,2.12082273054143,
6.5170260590526));
#104773=CARTESIAN_POINT('Ctrl Pts',(-2.7721699434562,-0.386565506913394,
6.67591799453647));
#104774=CARTESIAN_POINT('Ctrl Pts',(-1.17672454945654,-2.53962170829505,
6.83480993002035));
#104775=CARTESIAN_POINT('Ctrl Pts',(1.49732511225305,-2.36482062633797,
6.99370186550422));
#104776=CARTESIAN_POINT('Ctrl Pts',(2.79890297759256,-0.0223876877032405,
7.15259380098808));
#104777=CARTESIAN_POINT('Ctrl Pts',(1.53496226177243,2.34056615831974,7.31148573647197));
#104778=CARTESIAN_POINT('Ctrl Pts',(-1.13594905484471,2.55812017531127,
7.47037767195582));
#104779=CARTESIAN_POINT('Ctrl Pts',(-2.76563156475219,0.43086092255333,
7.6292696074397));
#104780=CARTESIAN_POINT('Ctrl Pts',(-1.86029259488113,-2.09133224236791,
7.78816154292357));
#104781=CARTESIAN_POINT('Ctrl Pts',(0.750219886458444,-2.69657731365141,
7.94705347840744));
#104782=CARTESIAN_POINT('Ctrl Pts',(2.67306899608655,-0.830097120039615,
8.10594541389131));
#104783=CARTESIAN_POINT('Ctrl Pts',(2.14574093520035,1.79726317648325,8.26483734937519));
#104784=CARTESIAN_POINT('Ctrl Pts',(-0.348407084677866,2.77722371981146,
8.42372928485904));
#104785=CARTESIAN_POINT('Ctrl Pts',(-2.52319967969691,1.21153723133653,
8.58262122034293));
#104786=CARTESIAN_POINT('Ctrl Pts',(-2.38518768160842,-1.4646633777222,
8.74151315582679));
#104787=CARTESIAN_POINT('Ctrl Pts',(-0.060875062987935,-2.79833045104458,
8.90040509131068));
#104788=CARTESIAN_POINT('Ctrl Pts',(2.31923659778409,-1.56700373006449,
9.05929702679454));
#104789=CARTESIAN_POINT('Ctrl Pts',(2.57349944087459,1.10066330653626,9.21818896227841));
#104790=CARTESIAN_POINT('Ctrl Pts',(0.468852137016506,2.75944500944524,
9.37708089776229));
#104791=CARTESIAN_POINT('Ctrl Pts',(-2.06555242493947,1.88887592667273,
9.53597283324615));
#104792=CARTESIAN_POINT('Ctrl Pts',(-2.70663908021347,-0.71306659997388,
9.69486476873003));
#104793=CARTESIAN_POINT('Ctrl Pts',(-0.86677769678369,-2.66140104285234,
9.85375670421389));
#104794=CARTESIAN_POINT('Ctrl Pts',(1.76758578430224,-2.17025334504288,
10.0126486396978));
#104795=CARTESIAN_POINT('Ctrl Pts',(2.78175227759491,0.310182772946269,
10.1715405751816));
#104796=CARTESIAN_POINT('Ctrl Pts',(1.24612079164814,2.50630047264078,10.3304325106655));
#104797=CARTESIAN_POINT('Ctrl Pts',(-1.43172465131564,2.40510365875409,
10.4893244461494));
#104798=CARTESIAN_POINT('Ctrl Pts',(-2.79722871429563,0.0993509257994383,
10.6482163816333));
#104799=CARTESIAN_POINT('Ctrl Pts',(-1.59874885224106,-2.29746843155571,
10.8071083171171));
#104800=CARTESIAN_POINT('Ctrl Pts',(1.06516940473778,-2.58839201546978,
10.966000252601));
#104801=CARTESIAN_POINT('Ctrl Pts',(2.7527365978123,-0.506754683848045,
11.1248921880849));
#104802=CARTESIAN_POINT('Ctrl Pts',(1.91710204103551,2.03938197765761,11.2837841235688));
#104803=CARTESIAN_POINT('Ctrl Pts',(-0.675778460895874,2.71618897691717,
11.4426760590526));
#104804=CARTESIAN_POINT('Ctrl Pts',(-2.64922977501486,0.903294351643931,
11.6015679945365));
#104805=CARTESIAN_POINT('Ctrl Pts',(-2.19435532437014,-1.73757411264833,
11.7604599300203));
#104806=CARTESIAN_POINT('Ctrl Pts',(0.271899800563075,-2.785754760382,11.9193518655042));
#104807=CARTESIAN_POINT('Ctrl Pts',(2.48892728304396,-1.28046869007272,
12.0782438009881));
#104808=CARTESIAN_POINT('Ctrl Pts',(2.42456479133692,1.39851516228695,12.237135736472));
#104809=CARTESIAN_POINT('Ctrl Pts',(0.137807999720803,2.79559797570218,
12.3960276719558));
#104810=CARTESIAN_POINT('Ctrl Pts',(-2.27526577635195,1.63019162477874,
12.5549196074397));
#104811=CARTESIAN_POINT('Ctrl Pts',(-2.60279508266664,-1.02947406192846,
12.7138115429236));
#104812=CARTESIAN_POINT('Ctrl Pts',(-0.544561395054448,-2.74550759852408,
12.8727034784075));
#104813=CARTESIAN_POINT('Ctrl Pts',(2.01282584978326,-1.94496559994811,
13.0315954138913));
#104814=CARTESIAN_POINT('Ctrl Pts',(2.72522519772037,0.638362521023264,
13.1904873493752));
#104815=CARTESIAN_POINT('Ctrl Pts',(0.939640178721769,2.63655749436058,
13.3493792848591));
#104816=CARTESIAN_POINT('Ctrl Pts',(-1.70723383722103,2.21804231510237,
13.5082712203429));
#104817=CARTESIAN_POINT('Ctrl Pts',(-2.78923041123751,-0.233565407466463,
13.6671631558268));
#104818=CARTESIAN_POINT('Ctrl Pts',(-1.31457443085917,-2.47108339646165,
13.8260550913107));
#104819=CARTESIAN_POINT('Ctrl Pts',(1.36504119109539,-2.44356739893747,
13.9849470267946));
#104820=CARTESIAN_POINT('Ctrl Pts',(2.79343854366366,-0.176239011888379,
14.1438389622784));
#104821=CARTESIAN_POINT('Ctrl Pts',(1.66132610133334,2.25263283105917,14.3027308977623));
#104822=CARTESIAN_POINT('Ctrl Pts',(-0.993584028683246,2.61670591860889,
14.4616228332461));
#104823=CARTESIAN_POINT('Ctrl Pts',(-2.73775937870298,0.582265120766335,
14.6205147687301));
#104824=CARTESIAN_POINT('Ctrl Pts',(-1.97246133395434,-1.98588906351594,
14.7794067042139));
#104825=CARTESIAN_POINT('Ctrl Pts',(0.600825856324219,-2.73374603372541,
14.9382986396978));
#104826=CARTESIAN_POINT('Ctrl Pts',(2.62338659742562,-0.975808304424984,
15.0971905751816));
#104827=CARTESIAN_POINT('Ctrl Pts',(2.24130983764105,1.67657069586423,15.2560825106655));
#104828=CARTESIAN_POINT('Ctrl Pts',(-0.195186843319176,2.79217857285889,
15.4149744461494));
#104829=CARTESIAN_POINT('Ctrl Pts',(-2.45277218746558,1.34843156405227,
15.5738663816333));
#104830=CARTESIAN_POINT('Ctrl Pts',(-2.46210788785084,-1.33130906821812,
15.7327583171171));
#104831=CARTESIAN_POINT('Ctrl Pts',(-0.214636694367242,-2.79075082656412,
15.891650252601));
#104832=CARTESIAN_POINT('Ctrl Pts',(2.22957387593874,-1.69214639386452,
16.0505421880849));
#104833=CARTESIAN_POINT('Ctrl Pts',(2.63012189252914,0.957506092396307,
16.2094341235687));
#104834=CARTESIAN_POINT('Ctrl Pts',(0.619858730590574,2.72949340366446,
16.3683260590526));
#104835=CARTESIAN_POINT('Ctrl Pts',(-1.95857671304387,1.99958404315983,
16.5272179945365));
#104836=CARTESIAN_POINT('Ctrl Pts',(-2.74174987350245,-0.563175565597893,
16.6861099300203));
#104837=CARTESIAN_POINT('Ctrl Pts',(-1.01179188876755,-2.60971957504275,
16.8450018655043));
#104838=CARTESIAN_POINT('Ctrl Pts',(1.64559048748105,-2.26415349171583,
17.0038938009881));
#104839=CARTESIAN_POINT('Ctrl Pts',(2.79459868770037,0.156771366137347,
17.162785736472));
#104840=CARTESIAN_POINT('Ctrl Pts',(1.38203368671266,2.43399711900581,17.3216776719558));
#104841=CARTESIAN_POINT('Ctrl Pts',(-1.29732517295305,2.48018275176639,
17.4805696074397));
#104842=CARTESIAN_POINT('Ctrl Pts',(-2.78753533269492,0.252993785525599,
17.6394615429236));
#104843=CARTESIAN_POINT('Ctrl Pts',(-1.72264667374927,-2.20609327181733,
17.7983534784075));
#104844=CARTESIAN_POINT('Ctrl Pts',(0.921247075997331,-2.64304046724668,
17.9572454138913));
#104845=CARTESIAN_POINT('Ctrl Pts',(2.72071123664003,-0.657335114958726,
18.1161373493752));
#104846=CARTESIAN_POINT('Ctrl Pts',(2.02632859821525,1.93089396358069,18.2750292848591));
#104847=CARTESIAN_POINT('Ctrl Pts',(-0.525418769132025,2.74923520339397,
18.4339212203429));
#104848=CARTESIAN_POINT('Ctrl Pts',(-2.59555901186999,1.04758412666344,
18.5928131558268));
#104849=CARTESIAN_POINT('Ctrl Pts',(-2.28656895721723,-1.61429907093739,
18.7517050913106));
#104850=CARTESIAN_POINT('Ctrl Pts',(0.118326240918447,-2.79649029807819,
18.9105970267946));
#104851=CARTESIAN_POINT('Ctrl Pts',(2.41476174175496,-1.41537444412829,
19.0694889622784));
#104852=CARTESIAN_POINT('Ctrl Pts',(2.49778857243239,1.26309593221353,19.2283808977623));
#104853=CARTESIAN_POINT('Ctrl Pts',(0.291303031405191,2.7837926701564,19.3872728332461));
#104854=CARTESIAN_POINT('Ctrl Pts',(-2.18219545925668,1.75282117288872,
19.54616476873));
#104855=CARTESIAN_POINT('Ctrl Pts',(-2.6554591996581,-0.884813836669676,
19.7050567042139));
#104856=CARTESIAN_POINT('Ctrl Pts',(-0.694687186450524,-2.71141453846537,
19.8639486396978));
#104857=CARTESIAN_POINT('Ctrl Pts',(1.90284605034815,-2.05268994131736,
20.0228405751816));
#104858=CARTESIAN_POINT('Ctrl Pts',(2.75620060787838,0.487562607415334,
20.1817325106655));
#104859=CARTESIAN_POINT('Ctrl Pts',(1.08317824906602,2.58090758578969,20.3406244461494));
#104860=CARTESIAN_POINT('Ctrl Pts',(-1.58270236367269,2.30855199522763,
20.4995163816333));
#104861=CARTESIAN_POINT('Ctrl Pts',(-2.79785304679384,-0.0798587386763005,
20.6584083171171));
#104862=CARTESIAN_POINT('Ctrl Pts',(-1.44844752999174,-2.39506969265607,
20.817300252601));
#104863=CARTESIAN_POINT('Ctrl Pts',(1.22862781735764,-2.51492202179281,
20.9761921880849));
#104864=CARTESIAN_POINT('Ctrl Pts',(2.77952355047542,-0.329557184248122,
21.1350841235687));
#104865=CARTESIAN_POINT('Ctrl Pts',(1.78266417767396,2.15788495228345,21.2939760590526));
#104866=CARTESIAN_POINT('Ctrl Pts',(-0.848213250953649,2.66737575156481,
21.4528679945365));
#104867=CARTESIAN_POINT('Ctrl Pts',(-2.70160509322647,0.731907861348415,
21.6117599300204));
#104868=CARTESIAN_POINT('Ctrl Pts',(-2.07866303761187,-1.8744382398188,
21.7706518655042));
#104869=CARTESIAN_POINT('Ctrl Pts',(0.449614145197882,-2.76264484192865,
21.9295438009881));
#104870=CARTESIAN_POINT('Ctrl Pts',(2.56576824795581,-1.11856738663923,
22.088435736472));
#104871=CARTESIAN_POINT('Ctrl Pts',(2.33009810417738,1.55080607790876,22.2473276719558));
#104872=CARTESIAN_POINT('Ctrl Pts',(-0.0413754771973295,2.79868717859702,
22.4062196074398));
#104873=CARTESIAN_POINT('Ctrl Pts',(-2.37492594999191,1.48124573051601,
22.5651115429236));
#104874=CARTESIAN_POINT('Ctrl Pts',(-2.53157746559467,-1.19392551607101,
22.7240034784075));
#104875=CARTESIAN_POINT('Ctrl Pts',(-0.367753579365892,-2.77473227569199,
22.8828954138913));
#104876=CARTESIAN_POINT('Ctrl Pts',(2.13317507136606,-1.81216337356762,
23.0417873493752));
#104877=CARTESIAN_POINT('Ctrl Pts',(2.67877121874512,0.811439507343116,
23.2006792848591));
#104878=CARTESIAN_POINT('Ctrl Pts',(0.769021883783568,2.6913090616914,23.3595712203429));
#104879=CARTESIAN_POINT('Ctrl Pts',(-1.84573657345466,2.10419657965654,
23.5184631558268));
#104880=CARTESIAN_POINT('Ctrl Pts',(-2.76845087541259,-0.411491995891901,
23.6773550913107));
#104881=CARTESIAN_POINT('Ctrl Pts',(-1.15396595201881,-2.55031293376487,
23.8362470267946));
#104882=CARTESIAN_POINT('Ctrl Pts',(1.51903866244618,-2.35088029971449,
23.9951389622784));
#104883=CARTESIAN_POINT('Ctrl Pts',(2.79818299902246,0.00226576998445874,
24.1540308977623));
#104884=CARTESIAN_POINT('Ctrl Pts',(1.51533643748012,2.35552788350921,24.3129228332461));
#104885=CARTESIAN_POINT('Ctrl Pts',(-1.16268678334851,2.5453813249875,24.4718408351714));
#104886=CARTESIAN_POINT('Ctrl Pts',(-2.22875207274563,1.12213500859344,
24.5777948586019));
#104887=CARTESIAN_POINT('Ctrl Pts',(-2.34264057946653,0.342150460324734,
24.6307849035378));
#104888=CARTESIAN_POINT('Ctrl Pts',(1.29201691215935,2.64852191642673,4.54887863488018E-15));
#104889=CARTESIAN_POINT('Ctrl Pts',(1.35230445507443,2.6121804996145,5.43378674156395E-15));
#104890=CARTESIAN_POINT('Ctrl Pts',(1.41110201644458,2.57358023305008,1.59117262741764E-15));
#104891=CARTESIAN_POINT('Ctrl Pts',(1.4682648448244,2.53271326293103,1.84054160801139E-15));
#104892=CARTESIAN_POINT('Ctrl Pts',(1.54796966940638,2.47573052122881,2.00750960553563E-15));
#104893=CARTESIAN_POINT('Ctrl Pts',(1.6244980979052,2.41434172809349,1.79546376567514E-15));
#104894=CARTESIAN_POINT('Ctrl Pts',(1.69767241980579,2.34892928422125,1.99493199737333E-15));
#104895=CARTESIAN_POINT('Ctrl Pts',(1.73624314581282,2.31444990150181,2.10007317684866E-15));
#104896=CARTESIAN_POINT('Ctrl Pts',(1.7738812599705,2.27885201635259,3.69427176174795E-15));
#104897=CARTESIAN_POINT('Ctrl Pts',(1.81055574615744,2.24218867772291,1.97064586870965E-15));
#104898=CARTESIAN_POINT('Ctrl Pts',(1.83140721175525,2.22134355012547,5.86266064330246E-16));
#104899=CARTESIAN_POINT('Ctrl Pts',(1.85194673165548,2.2001543900091,8.11396458076517E-16));
#104900=CARTESIAN_POINT('Ctrl Pts',(1.87216939098153,2.1786293341467,1.80411241501588E-15));
#104901=CARTESIAN_POINT('Ctrl Pts',(1.88524297304094,2.16471377637492,2.44588525584221E-15));
#104902=CARTESIAN_POINT('Ctrl Pts',(1.89818330708257,2.15065853098203,1.189897513384E-15));
#104903=CARTESIAN_POINT('Ctrl Pts',(1.91097839287718,2.13647800248694,1.09634523681734E-15));
#104904=CARTESIAN_POINT('Ctrl Pts',(1.97606835821047,2.06434014245464,3.44342342483582E-16));
#104905=CARTESIAN_POINT('Ctrl Pts',(2.03746495618161,1.98889786290504,8.29405017125788E-16));
#104906=CARTESIAN_POINT('Ctrl Pts',(2.0949947735992,1.91052554193752,7.63278329429795E-17));
#104907=CARTESIAN_POINT('Ctrl Pts',(2.15236598115915,1.83236929366463,-6.74673115466274E-16));
#104908=CARTESIAN_POINT('Ctrl Pts',(2.20589202711639,1.75129816353633,-1.41513655082523E-15));
#104909=CARTESIAN_POINT('Ctrl Pts',(2.25535281672612,1.66766527191713,-2.42861286636753E-15));
#104910=CARTESIAN_POINT('Ctrl Pts',(2.27484369419206,1.6347082881016,-2.827990693465E-15));
#104911=CARTESIAN_POINT('Ctrl Pts',(2.29370272849397,1.6013533709117,-3.52613603609337E-15));
#104912=CARTESIAN_POINT('Ctrl Pts',(2.31191421992203,1.56762185467499,-2.13717932240343E-15));
#104913=CARTESIAN_POINT('Ctrl Pts',(2.3215636330504,1.54974911004558,-1.4012364590331E-15));
#104914=CARTESIAN_POINT('Ctrl Pts',(2.33103139846528,1.53176995434509,-1.06177166968173E-15));
#104915=CARTESIAN_POINT('Ctrl Pts',(2.34030381034639,1.51371048032841,-1.2490009027033E-15));
#104916=CARTESIAN_POINT('Ctrl Pts',(2.38367085566508,1.42924636913981,-2.12467151974787E-15));
#104917=CARTESIAN_POINT('Ctrl Pts',(2.42283443804809,1.34290694301736,-9.36944287622972E-16));
#104918=CARTESIAN_POINT('Ctrl Pts',(2.45762895649157,1.2550365169234,-2.38697950294409E-15));
#104919=CARTESIAN_POINT('Ctrl Pts',(2.4920487142431,1.16811251524223,-3.82139685013631E-15));
#104920=CARTESIAN_POINT('Ctrl Pts',(2.52219321924462,1.07968940189563,-3.00090063764714E-15));
#104921=CARTESIAN_POINT('Ctrl Pts',(2.54785251130495,0.990091831681564,
-3.27515792264421E-15));
#104922=CARTESIAN_POINT('Ctrl Pts',(2.57275717075288,0.903129300981329,
-3.54134937749438E-15));
#104923=CARTESIAN_POINT('Ctrl Pts',(2.59343656824167,0.815059624988842,
-1.78047228398232E-15));
#104924=CARTESIAN_POINT('Ctrl Pts',(2.60965039179134,0.726183587939375,
-2.74780198594726E-15));
#104925=CARTESIAN_POINT('Ctrl Pts',(2.61912055200124,0.674272926206792,
-3.31279933067173E-15));
#104926=CARTESIAN_POINT('Ctrl Pts',(2.62706637598171,0.62208730687767,-6.0589320933173E-15));
#104927=CARTESIAN_POINT('Ctrl Pts',(2.63343195267653,0.56968881258124,-5.32907051820075E-15));
#104928=CARTESIAN_POINT('Ctrl Pts',(2.63584888151175,0.549793768053726,
-5.02254639302231E-15));
#104929=CARTESIAN_POINT('Ctrl Pts',(2.63803838941423,0.52986220654713,-1.31175086481935E-15));
#104930=CARTESIAN_POINT('Ctrl Pts',(2.63999431323799,0.509930525450882,
-2.02615701994091E-15));
#104931=CARTESIAN_POINT('Ctrl Pts',(2.64870355681473,0.42117969402649,-3.85326558685E-15));
#104932=CARTESIAN_POINT('Ctrl Pts',(2.65280061996473,0.332324654199259,
-3.41581273799203E-15));
#104933=CARTESIAN_POINT('Ctrl Pts',(2.65210228927602,0.24365609144491,-2.05391259555654E-15));
#104934=CARTESIAN_POINT('Ctrl Pts',(2.65178733264356,0.203665364440984,
-1.99754801784407E-15));
#104935=CARTESIAN_POINT('Ctrl Pts',(2.65049624272211,0.163712613523904,
-2.3425961516863E-15));
#104936=CARTESIAN_POINT('Ctrl Pts',(2.64820874432577,0.123825020344308,
-2.24820162486594E-15));
#104937=CARTESIAN_POINT('Ctrl Pts',(2.64295670172582,0.0322440430970331,
-2.21457773022915E-15));
#104938=CARTESIAN_POINT('Ctrl Pts',(2.63245536449145,-0.05899509673886,
-1.93770170853692E-15));
#104939=CARTESIAN_POINT('Ctrl Pts',(2.61690932751102,-0.149544955572229,
-3.13638004456607E-15));
#104940=CARTESIAN_POINT('Ctrl Pts',(2.6013632905306,-0.240094814405598,
-4.33505838059522E-15));
#104941=CARTESIAN_POINT('Ctrl Pts',(2.58077188138282,-0.329956281632541,
-1.29603811372711E-15));
#104942=CARTESIAN_POINT('Ctrl Pts',(2.55529474752967,-0.418751394683592,
-2.24820162486594E-15));
#104943=CARTESIAN_POINT('Ctrl Pts',(2.5508308695639,-0.434309288711294,
-2.57358246102794E-15));
#104944=CARTESIAN_POINT('Ctrl Pts',(2.54621690810265,-0.449834351812699,
3.60179654402708E-16));
#104945=CARTESIAN_POINT('Ctrl Pts',(2.54145360363441,-0.465324422952669,
-1.55431223447522E-15));
#104946=CARTESIAN_POINT('Ctrl Pts',(2.53754660451264,-0.478029824159677,
-3.18176020908992E-15));
#104947=CARTESIAN_POINT('Ctrl Pts',(2.5335420591532,-0.490702157165281,
9.72084519165929E-17));
#104948=CARTESIAN_POINT('Ctrl Pts',(2.52944084941284,-0.503340204338878,
-4.71844785465692E-16));
#104949=CARTESIAN_POINT('Ctrl Pts',(2.50206015777548,-0.587714936299748,
-2.72570571264101E-15));
#104950=CARTESIAN_POINT('Ctrl Pts',(2.47037373520267,-0.670566907612742,
-2.45628779146457E-15));
#104951=CARTESIAN_POINT('Ctrl Pts',(2.43459352459919,-0.751592967054325,
-2.44249065417534E-15));
#104952=CARTESIAN_POINT('Ctrl Pts',(2.39879623125327,-0.832657711212454,
-2.42868692964309E-15));
#104953=CARTESIAN_POINT('Ctrl Pts',(2.35890058949824,-0.911895594830773,
-2.48837357958352E-15));
#104954=CARTESIAN_POINT('Ctrl Pts',(2.31507655407985,-0.988972835355777,
-6.93889390390723E-16));
#104955=CARTESIAN_POINT('Ctrl Pts',(2.27205772689207,-1.06463388433495,
1.06762354398604E-15));
#104956=CARTESIAN_POINT('Ctrl Pts',(2.22525285000344,-1.13821355917498,
-1.39552169477871E-15));
#104957=CARTESIAN_POINT('Ctrl Pts',(2.17479201285555,-1.20935690519725,
-1.38777878078145E-15));
#104958=CARTESIAN_POINT('Ctrl Pts',(2.15736382618763,-1.23392842609816,
-1.38510452965671E-15));
#104959=CARTESIAN_POINT('Ctrl Pts',(2.1394993027235,-1.25820893371577,-8.89972469010783E-16));
#104960=CARTESIAN_POINT('Ctrl Pts',(2.12120315232448,-1.2821824919793,-1.22124532708767E-15));
#104961=CARTESIAN_POINT('Ctrl Pts',(2.11083609771111,-1.29576650732539,
-1.45441170047064E-15));
#104962=CARTESIAN_POINT('Ctrl Pts',(2.10033045792001,-1.30925195930262,
9.10990193106776E-16));
#104963=CARTESIAN_POINT('Ctrl Pts',(2.08968705080315,-1.32263584234787,
4.44089209850063E-16));
#104964=CARTESIAN_POINT('Ctrl Pts',(2.08126174077994,-1.33323051027069,
4.10545969975963E-17));
#104965=CARTESIAN_POINT('Ctrl Pts',(2.07275349646736,-1.34375719535956,
5.44615819269545E-16));
#104966=CARTESIAN_POINT('Ctrl Pts',(2.06416789660031,-1.35420866670935,
5.55111512312578E-16));
#104967=CARTESIAN_POINT('Ctrl Pts',(2.01002859219675,-1.42011383322463,
1.37201142676444E-15));
#104968=CARTESIAN_POINT('Ctrl Pts',(1.95275671705684,-1.48310619814664,
1.18076742119145E-15));
#104969=CARTESIAN_POINT('Ctrl Pts',(1.89251077597855,-1.54288980711619,
2.22044604925031E-16));
#104970=CARTESIAN_POINT('Ctrl Pts',(1.83320824964783,-1.60173724117744,
-6.61500643283973E-16));
#104971=CARTESIAN_POINT('Ctrl Pts',(1.77102343304878,-1.65747614431305,
2.34162966278675E-15));
#104972=CARTESIAN_POINT('Ctrl Pts',(1.70608147665216,-1.7097819039225,7.7715611723761E-16));
#104973=CARTESIAN_POINT('Ctrl Pts',(1.64316795857729,-1.76045391220805,
1.2348827422763E-16));
#104974=CARTESIAN_POINT('Ctrl Pts',(1.57766627853085,-1.80790418089787,
-3.2358106014976E-16));
#104975=CARTESIAN_POINT('Ctrl Pts',(1.50967443903864,-1.85179189330092,
-2.33146835171283E-15));
#104976=CARTESIAN_POINT('Ctrl Pts',(1.46645654143987,-1.87968839786154,
-2.59398396294788E-15));
#104977=CARTESIAN_POINT('Ctrl Pts',(1.42223225631607,-1.90614459401194,
8.75155213223675E-16));
#104978=CARTESIAN_POINT('Ctrl Pts',(1.37702479013102,-1.93106208855765,
7.7715611723761E-16));
#104979=CARTESIAN_POINT('Ctrl Pts',(-1.03676051102385,2.12842394760949,
-0.331722097696724));
#104980=CARTESIAN_POINT('Ctrl Pts',(-1.7455522477269,1.78318492571192,-0.278722164800846));
#104981=CARTESIAN_POINT('Ctrl Pts',(-2.77856061136894,0.334956131708931,
-0.172733943176718));
#104982=CARTESIAN_POINT('Ctrl Pts',(-1.78365806106894,-2.16005006104753,
-0.0137574328243411));
#104983=CARTESIAN_POINT('Ctrl Pts',(0.849859252582268,-2.66646553285166,
0.145207433360407));
#104984=CARTESIAN_POINT('Ctrl Pts',(2.70250349758136,-0.730105073536833,
0.304172299545154));
#104985=CARTESIAN_POINT('Ctrl Pts',(2.07654652319967,1.8778076872183,0.463137165729903));
#104986=CARTESIAN_POINT('Ctrl Pts',(-0.454739712339021,2.76212359428796,
0.62210203191465));
#104987=CARTESIAN_POINT('Ctrl Pts',(-2.56867903914637,1.11298801703124,
0.781066898099398));
#104988=CARTESIAN_POINT('Ctrl Pts',(-2.3262392006046,-1.55744028288047,
0.940031764284147));
#104989=CARTESIAN_POINT('Ctrl Pts',(0.0503084804544499,-2.79896185679702,
1.0989966304689));
#104990=CARTESIAN_POINT('Ctrl Pts',(2.38067870632853,-1.47282370987667,
1.25796149665364));
#104991=CARTESIAN_POINT('Ctrl Pts',(2.52706021534629,1.20449898638212,1.41692636283839));
#104992=CARTESIAN_POINT('Ctrl Pts',(0.355144551310132,2.77681184748758,
1.57589122902314));
#104993=CARTESIAN_POINT('Ctrl Pts',(-2.1425722229245,1.80172569768908,1.73485609520789));
#104994=CARTESIAN_POINT('Ctrl Pts',(-2.67472461252547,-0.826244041728367,
1.89382096139263));
#104995=CARTESIAN_POINT('Ctrl Pts',(-0.753120451482905,-2.6962261287845,
2.05278582757738));
#104996=CARTESIAN_POINT('Ctrl Pts',(1.85938553014776,-2.09272889546975,
2.21175069376213));
#104997=CARTESIAN_POINT('Ctrl Pts',(2.76611708141006,0.430609784178951,
2.37071555994688));
#104998=CARTESIAN_POINT('Ctrl Pts',(1.13525073787139,2.55891257909954,2.52968042613162));
#104999=CARTESIAN_POINT('Ctrl Pts',(-1.53707893828351,2.33970438741627,
2.68864529231638));
#105000=CARTESIAN_POINT('Ctrl Pts',(-2.79931358384604,-0.0259165258534752,
2.84761015850112));
#105001=CARTESIAN_POINT('Ctrl Pts',(-1.49349644210569,-2.36776191833878,
3.00657502468587));
#105002=CARTESIAN_POINT('Ctrl Pts',(1.18243377626383,-2.53745513396945,
3.16553989087062));
#105003=CARTESIAN_POINT('Ctrl Pts',(2.77361552270627,-0.379321906352915,
3.32450475705537));
#105004=CARTESIAN_POINT('Ctrl Pts',(1.82032054711271,2.12679601103407,3.48346962324011));
#105005=CARTESIAN_POINT('Ctrl Pts',(-0.802911451550624,2.68182053417896,
3.64243448942486));
#105006=CARTESIAN_POINT('Ctrl Pts',(-2.68956353241581,0.776579795495751,
3.8013993556096));
#105007=CARTESIAN_POINT('Ctrl Pts',(-2.10884703321116,-1.84108456165128,
3.96036422179436));
#105008=CARTESIAN_POINT('Ctrl Pts',(0.406496718972051,-2.76976327354607,
4.11932908797911));
#105009=CARTESIAN_POINT('Ctrl Pts',(2.54892597416715,-1.15749926640803,
4.27829395416385));
#105010=CARTESIAN_POINT('Ctrl Pts',(2.35300561059747,1.51663864183913,4.43725882034861));
#105011=CARTESIAN_POINT('Ctrl Pts',(-0.00152972572175765,2.79943312718021,
4.59622368653335));
#105012=CARTESIAN_POINT('Ctrl Pts',(-2.35466171272765,1.51406617825868,
4.7551885527181));
#105013=CARTESIAN_POINT('Ctrl Pts',(-2.54765944163499,-1.16028425093789,
4.91415341890285));
#105014=CARTESIAN_POINT('Ctrl Pts',(-0.403469451362134,-2.77020587238022,
5.0731182850876));
#105015=CARTESIAN_POINT('Ctrl Pts',(2.11085786236346,-1.83877874102286,
5.23208315127234));
#105016=CARTESIAN_POINT('Ctrl Pts',(2.68871321588955,0.77951870807597,5.39104801745709));
#105017=CARTESIAN_POINT('Ctrl Pts',(0.799980058451885,2.68269641957907,
5.55001288364184));
#105018=CARTESIAN_POINT('Ctrl Pts',(-1.82264379789626,2.12480534626852,
5.70897774982658));
#105019=CARTESIAN_POINT('Ctrl Pts',(-2.77319931132722,-0.382352917074548,
5.86794261601134));
#105020=CARTESIAN_POINT('Ctrl Pts',(-1.17965993226115,-2.53874587498616,
6.02690748219608));
#105021=CARTESIAN_POINT('Ctrl Pts',(1.49608323803294,-2.36612829711708,
6.18587234838083));
#105022=CARTESIAN_POINT('Ctrl Pts',(2.79934022996841,-0.0228571744051168,
6.34483721456558));
#105023=CARTESIAN_POINT('Ctrl Pts',(1.53452101031131,2.34138280562034,6.50380208075032));
#105024=CARTESIAN_POINT('Ctrl Pts',(-1.13804667113744,2.55767041423525,
6.66276694693508));
#105025=CARTESIAN_POINT('Ctrl Pts',(-2.76658599456728,0.42758637514024,
6.82173181311982));
#105026=CARTESIAN_POINT('Ctrl Pts',(-1.85709739130469,-2.09475952146081,
6.98069667930457));
#105027=CARTESIAN_POINT('Ctrl Pts',(0.756066807429931,-2.69540185431488,
7.13966154548932));
#105028=CARTESIAN_POINT('Ctrl Pts',(2.67562571955118,-0.823319611340344,
7.29862641167407));
#105029=CARTESIAN_POINT('Ctrl Pts',(2.14060240978145,1.80406471524147,7.4575912778588));
#105030=CARTESIAN_POINT('Ctrl Pts',(-0.358180098740468,2.77642489370911,
7.61655614404357));
#105031=CARTESIAN_POINT('Ctrl Pts',(-2.52837311278293,1.20173107478242,
7.7755210102283));
#105032=CARTESIAN_POINT('Ctrl Pts',(-2.37907142037402,-1.47541429785025,
7.93448587641306));
#105033=CARTESIAN_POINT('Ctrl Pts',(-0.0472423399272245,-2.79903489346946,
8.09345074259782));
#105034=CARTESIAN_POINT('Ctrl Pts',(2.32792621317397,-1.55485938899917,
8.25241560878254));
#105035=CARTESIAN_POINT('Ctrl Pts',(2.56748728762925,1.11572272604064,8.41138047496732));
#105036=CARTESIAN_POINT('Ctrl Pts',(0.451670849790703,2.76275616314411,
8.57034534115203));
#105037=CARTESIAN_POINT('Ctrl Pts',(-2.07850221122631,1.87527510820912,
8.72931020733681));
#105038=CARTESIAN_POINT('Ctrl Pts',(-2.70188594122545,-0.732557529583622,
8.88827507352154));
#105039=CARTESIAN_POINT('Ctrl Pts',(-0.846596683277061,-2.66835196880128,
9.04723993970629));
#105040=CARTESIAN_POINT('Ctrl Pts',(1.78534872381028,-2.1562370249883,9.20620480589104));
#105041=CARTESIAN_POINT('Ctrl Pts',(2.77943977581406,0.333980098455095,
9.36516967207578));
#105042=CARTESIAN_POINT('Ctrl Pts',(1.22371101906138,2.51780847471947,9.52413453826054));
#105043=CARTESIAN_POINT('Ctrl Pts',(-1.45463338986256,2.3918339981358,9.68309940444529));
#105044=CARTESIAN_POINT('Ctrl Pts',(-2.79851714084195,0.0716239202725503,
9.84206427063003));
#105045=CARTESIAN_POINT('Ctrl Pts',(-1.5750797708687,-2.31429295659422,
10.0010291368147));
#105046=CARTESIAN_POINT('Ctrl Pts',(1.0933141097943,-2.57710931682498,10.1599940029995));
#105047=CARTESIAN_POINT('Ctrl Pts',(2.75871666875113,-0.475721047564691,
10.3189588691842));
#105048=CARTESIAN_POINT('Ctrl Pts',(1.89331051224729,2.0620871654116,10.477923735369));
#105049=CARTESIAN_POINT('Ctrl Pts',(-0.70899265863458,2.70816498455018,
10.6368886015537));
#105050=CARTESIAN_POINT('Ctrl Pts',(-2.6608757193272,0.869809507786801,
10.7958534677385));
#105051=CARTESIAN_POINT('Ctrl Pts',(-2.17170800539298,-1.76649724394164,
10.9548183339232));
#105052=CARTESIAN_POINT('Ctrl Pts',(0.309754752733788,-2.78224372884552,
11.113783200108));
#105053=CARTESIAN_POINT('Ctrl Pts',(2.50705276253614,-1.24559809706071,
11.2727480662927));
#105054=CARTESIAN_POINT('Ctrl Pts',(2.40441506186246,1.43374209111343,11.4317129324775));
#105055=CARTESIAN_POINT('Ctrl Pts',(0.0960000651458504,2.79778701137764,
11.5906777986622));
#105056=CARTESIAN_POINT('Ctrl Pts',(-2.3004840704961,1.5951806214141,11.749642664847));
#105057=CARTESIAN_POINT('Ctrl Pts',(-2.58653577161565,-1.07082252296726,
11.9086075310317));
#105058=CARTESIAN_POINT('Ctrl Pts',(-0.499735143315288,-2.75446781794179,
12.0675723972165));
#105059=CARTESIAN_POINT('Ctrl Pts',(2.04551562973912,-1.91120223472933,
12.2265372634012));
#105060=CARTESIAN_POINT('Ctrl Pts',(2.71423850777836,0.685373982898722,
12.3855021295861));
#105061=CARTESIAN_POINT('Ctrl Pts',(0.892956323270132,2.6531975384945,12.5444669957707));
#105062=CARTESIAN_POINT('Ctrl Pts',(-1.7475117062567,2.18701417691729,12.7034318619554));
#105063=CARTESIAN_POINT('Ctrl Pts',(-2.78483654001413,-0.285505900015315,
12.8623967281402));
#105064=CARTESIAN_POINT('Ctrl Pts',(-1.2673906477906,-2.4961067924739,13.0213615943249));
#105065=CARTESIAN_POINT('Ctrl Pts',(1.41274198702393,-2.41681365678884,
13.1803264605097));
#105066=CARTESIAN_POINT('Ctrl Pts',(2.79684456048536,-0.120368924664381,
13.3392913266944));
#105067=CARTESIAN_POINT('Ctrl Pts',(1.61516041520069,2.28650060282304,13.4982561928792));
#105068=CARTESIAN_POINT('Ctrl Pts',(-1.04824967242495,2.59576593663651,
13.6572210590639));
#105069=CARTESIAN_POINT('Ctrl Pts',(-2.75000993315739,0.523711314635311,
13.8161859252487));
#105070=CARTESIAN_POINT('Ctrl Pts',(-1.92894891786922,-2.0287888618071,
13.9751507914334));
#105071=CARTESIAN_POINT('Ctrl Pts',(0.661703294775168,-2.72010604999605,
14.1341156576182));
#105072=CARTESIAN_POINT('Ctrl Pts',(2.6453180089931,-0.916035373136955,
14.2930805238029));
#105073=CARTESIAN_POINT('Ctrl Pts',(2.20215437799027,1.72839355155001,14.4520453899877));
#105074=CARTESIAN_POINT('Ctrl Pts',(-0.26123538052229,2.78721801255387,
14.6110102561724));
#105075=CARTESIAN_POINT('Ctrl Pts',(-2.48497139521209,1.28908701743486,
14.7699751223572));
#105076=CARTESIAN_POINT('Ctrl Pts',(-2.42902884199723,-1.3916346712722,
14.9289399885419));
#105077=CARTESIAN_POINT('Ctrl Pts',(-0.144728649498314,-2.79568985968684,
15.0879048547267));
#105078=CARTESIAN_POINT('Ctrl Pts',(2.27234361476724,-1.63501763598071,
15.2468697209114));
#105079=CARTESIAN_POINT('Ctrl Pts',(2.60479911141896,1.02559727119973,15.4058345870963));
#105080=CARTESIAN_POINT('Ctrl Pts',(0.547647741995679,2.74534335270262,
15.5647994532809));
#105081=CARTESIAN_POINT('Ctrl Pts',(-2.0119081309943,1.94654921488784,15.7237643194657));
#105082=CARTESIAN_POINT('Ctrl Pts',(-2.72576716592093,-0.63798239061021,
15.8827291856504));
#105083=CARTESIAN_POINT('Ctrl Pts',(-0.93904490593987,-2.63723772879309,
16.0416940518351));
#105084=CARTESIAN_POINT('Ctrl Pts',(1.70914423068041,-2.21712745963629,
16.2006589180199));
#105085=CARTESIAN_POINT('Ctrl Pts',(2.78938796573705,0.236945036121653,
16.3596237842046));
#105086=CARTESIAN_POINT('Ctrl Pts',(1.31068555947639,2.47364741580554,16.5185886503894));
#105087=CARTESIAN_POINT('Ctrl Pts',(-1.37042174567262,2.44105969048874,
16.6775535165741));
#105088=CARTESIAN_POINT('Ctrl Pts',(-2.79432299661122,0.169077391010992,
16.8365183827589));
#105089=CARTESIAN_POINT('Ctrl Pts',(-1.65475077680833,-2.25801418068922,
16.9954832489436));
#105090=CARTESIAN_POINT('Ctrl Pts',(1.00286703836107,-2.61363461044391,
17.1544481151284));
#105091=CARTESIAN_POINT('Ctrl Pts',(2.74046843071987,-0.571542608883376,
17.3134129813131));
#105092=CARTESIAN_POINT('Ctrl Pts',(1.96400179011519,1.99487471836346,17.4723778474979));
#105093=CARTESIAN_POINT('Ctrl Pts',(-0.614213070560955,2.73122142593629,
17.6313427136826));
#105094=CARTESIAN_POINT('Ctrl Pts',(-2.62895731109937,0.961983175507027,
17.7903075798675));
#105095=CARTESIAN_POINT('Ctrl Pts',(-2.2319322855622,-1.68976520446079,
17.9492724460521));
#105096=CARTESIAN_POINT('Ctrl Pts',(0.21263671018481,-2.79134623488795,
18.1082373122369));
#105097=CARTESIAN_POINT('Ctrl Pts',(2.4621357136205,-1.33218463482211,18.2672021784216));
#105098=CARTESIAN_POINT('Ctrl Pts',(2.45290528925346,1.34910482005423,18.4261670446065));
#105099=CARTESIAN_POINT('Ctrl Pts',(0.193413301399417,2.79274407498839,
18.5851319107911));
#105100=CARTESIAN_POINT('Ctrl Pts',(-2.24351338803655,1.67435834015417,
18.7440967769758));
#105101=CARTESIAN_POINT('Ctrl Pts',(-2.62227176319312,-0.980060698885337,
18.9030616431606));
#105102=CARTESIAN_POINT('Ctrl Pts',(-0.595394101940265,-2.7353855371618,
19.0620265093455));
#105103=CARTESIAN_POINT('Ctrl Pts',(1.977689916566,-1.98130531909285,19.2209913755301));
#105104=CARTESIAN_POINT('Ctrl Pts',(2.73646841612022,0.590397138460929,
19.379956241715));
#105105=CARTESIAN_POINT('Ctrl Pts',(0.984848441080798,2.620477384301,19.5389211078996));
#105106=CARTESIAN_POINT('Ctrl Pts',(-1.67025794355887,2.24656773225142,
19.6978859740844));
#105107=CARTESIAN_POINT('Ctrl Pts',(-2.79309267137315,-0.188312247462501,
19.8568508402691));
#105108=CARTESIAN_POINT('Ctrl Pts',(-1.35358261196975,-2.4504371622411,
20.0158157064539));
#105109=CARTESIAN_POINT('Ctrl Pts',(1.32768551221931,-2.46456473939368,
20.1747805726386));
#105110=CARTESIAN_POINT('Ctrl Pts',(2.79095321448688,-0.217734533731887,
20.3337454388233));
#105111=CARTESIAN_POINT('Ctrl Pts',(1.69383883831331,2.2288423370653,20.4927103050081));
#105112=CARTESIAN_POINT('Ctrl Pts',(-0.957179984086533,2.63070991457424,
20.6516751711928));
#105113=CARTESIAN_POINT('Ctrl Pts',(-2.73009505669085,0.619200410386925,
20.8106400373776));
#105114=CARTESIAN_POINT('Ctrl Pts',(-1.99845849072177,-1.96035502838096,
20.9696049035625));
#105115=CARTESIAN_POINT('Ctrl Pts',(0.566536405591253,-2.74150774087858,
21.1285697697471));
#105116=CARTESIAN_POINT('Ctrl Pts',(2.61179858446281,-1.00763896248394,
21.2875346359319));
#105117=CARTESIAN_POINT('Ctrl Pts',(2.26103270329154,1.65062391890566,21.4464995021166));
#105118=CARTESIAN_POINT('Ctrl Pts',(-0.163973521133312,2.79462716070978,
21.6054643683013));
#105119=CARTESIAN_POINT('Ctrl Pts',(-2.43855259750074,1.37487783258505,
21.7644292344861));
#105120=CARTESIAN_POINT('Ctrl Pts',(-2.47603725527275,-1.30616538187191,
21.9233941006708));
#105121=CARTESIAN_POINT('Ctrl Pts',(-0.242039052944788,-2.78895067659981,
22.0823589668556));
#105122=CARTESIAN_POINT('Ctrl Pts',(2.21400177968597,-1.71319055318707,
22.2413238330403));
#105123=CARTESIAN_POINT('Ctrl Pts',(2.63894911424742,0.934226172697978,
22.4002886992251));
#105124=CARTESIAN_POINT('Ctrl Pts',(0.642958410343447,2.72459826446569,
22.5592535654098));
#105125=CARTESIAN_POINT('Ctrl Pts',(-1.94286885474847,2.01545833544657,
22.7182184315946));
#105126=CARTESIAN_POINT('Ctrl Pts',(-2.74634381808181,-0.542629498889809,
22.8771832977793));
#105127=CARTESIAN_POINT('Ctrl Pts',(-1.03034384648533,-2.6029276480822,
23.036148163964));
#105128=CARTESIAN_POINT('Ctrl Pts',(1.63084712721742,-2.27531449840608,
23.1951130301488));
#105129=CARTESIAN_POINT('Ctrl Pts',(2.79598298084694,0.1396002291639,23.3540778963335));
#105130=CARTESIAN_POINT('Ctrl Pts',(1.39600493091336,2.42652520388118,23.5130427625183));
#105131=CARTESIAN_POINT('Ctrl Pts',(-1.284424361538,2.48724124595668,23.672007628703));
#105132=CARTESIAN_POINT('Ctrl Pts',(-2.78696897019498,0.26647914057034,
23.8309724948878));
#105133=CARTESIAN_POINT('Ctrl Pts',(-1.73196816232114,-2.19928735220062,
23.9899373610725));
#105134=CARTESIAN_POINT('Ctrl Pts',(0.910351149945236,-2.64642399680759,
24.1489022272573));
#105135=CARTESIAN_POINT('Ctrl Pts',(2.7205403994727,-0.667766635797716,
24.3078670934421));
#105136=CARTESIAN_POINT('Ctrl Pts',(2.0288526792701,1.92795307285542,24.4668579886134));
#105137=CARTESIAN_POINT('Ctrl Pts',(0.335086850842407,2.47282047565727,
24.5728605950565));
#105138=CARTESIAN_POINT('Ctrl Pts',(-0.439799363723413,2.32629260682496,
24.6258749127712));
#105139=CARTESIAN_POINT('Ctrl Pts',(-1.12118154143677,2.30173662773389,
-0.220420412161518));
#105140=CARTESIAN_POINT('Ctrl Pts',(-1.88768856351612,1.92838558415202,
-0.167420479265639));
#105141=CARTESIAN_POINT('Ctrl Pts',(-3.004812428816,0.362230841230852,-0.0614322576415114));
#105142=CARTESIAN_POINT('Ctrl Pts',(-1.92889724583594,-2.33593798304895,
0.0975442527108654));
#105143=CARTESIAN_POINT('Ctrl Pts',(0.919061342212502,-2.88358970516562,
0.256509118895613));
#105144=CARTESIAN_POINT('Ctrl Pts',(2.9225621587036,-0.789555855045466,
0.415473985080361));
#105145=CARTESIAN_POINT('Ctrl Pts',(2.24563494364476,2.03071326009328,0.574438851265108));
#105146=CARTESIAN_POINT('Ctrl Pts',(-0.491768124086146,2.98703698313542,
0.733403717449859));
#105147=CARTESIAN_POINT('Ctrl Pts',(-2.77784068156911,1.20361607841659,
0.892368583634605));
#105148=CARTESIAN_POINT('Ctrl Pts',(-2.51565952305497,-1.68425907284144,
1.05133344981935));
#105149=CARTESIAN_POINT('Ctrl Pts',(0.0544049846261753,-3.0268749008653,
1.2102983160041));
#105150=CARTESIAN_POINT('Ctrl Pts',(2.57453191286305,-1.5927523663815,1.36926318218884));
#105151=CARTESIAN_POINT('Ctrl Pts',(2.73283293240736,1.30257857610461,1.52822804837359));
#105152=CARTESIAN_POINT('Ctrl Pts',(0.384063157534352,3.00292126710289,
1.68719291455834));
#105153=CARTESIAN_POINT('Ctrl Pts',(-2.31703696465619,1.94843608866463,
1.84615778074309));
#105154=CARTESIAN_POINT('Ctrl Pts',(-2.89252130275355,-0.893523198904568,
2.00512264692783));
#105155=CARTESIAN_POINT('Ctrl Pts',(-0.814445322427711,-2.91577363816391,
2.16408751311259));
#105156=CARTESIAN_POINT('Ctrl Pts',(2.01079102902708,-2.26313500937155,
2.32305237929733));
#105157=CARTESIAN_POINT('Ctrl Pts',(2.99135565075408,0.465673351222398,
2.48201724548208));
#105158=CARTESIAN_POINT('Ctrl Pts',(1.22769160155114,2.76727896108183,2.64098211166683));
#105159=CARTESIAN_POINT('Ctrl Pts',(-1.66223975065641,2.53022114914384,
2.79994697785158));
#105160=CARTESIAN_POINT('Ctrl Pts',(-3.02725526824118,-0.0280268491094517,
2.95891184403632));
#105161=CARTESIAN_POINT('Ctrl Pts',(-1.61510843177923,-2.5605633404543,
3.11787671022108));
#105162=CARTESIAN_POINT('Ctrl Pts',(1.27871664653699,-2.74407428541136,
3.27684157640582));
#105163=CARTESIAN_POINT('Ctrl Pts',(2.99946467292601,-0.410209219143078,
3.43580644259057));
#105164=CARTESIAN_POINT('Ctrl Pts',(1.96854507402614,2.29997613201714,3.59477130877531));
#105165=CARTESIAN_POINT('Ctrl Pts',(-0.868290689426212,2.9001950290315,
3.75373617496007));
#105166=CARTESIAN_POINT('Ctrl Pts',(-2.9085685218548,0.83981490701523,3.91270104114481));
#105167=CARTESIAN_POINT('Ctrl Pts',(-2.28056561009935,-1.99099985464254,
4.07166590732956));
#105168=CARTESIAN_POINT('Ctrl Pts',(0.439596814423422,-2.99529874395252,
4.23063077351431));
#105169=CARTESIAN_POINT('Ctrl Pts',(2.7564791698159,-1.25175177673545,4.38959563969905));
#105170=CARTESIAN_POINT('Ctrl Pts',(2.5446054604199,1.64013504775611,4.54856050588381));
#105171=CARTESIAN_POINT('Ctrl Pts',(-0.00165428777859027,3.02738454571485,
4.70752537206855));
#105172=CARTESIAN_POINT('Ctrl Pts',(-2.54639641514797,1.63735311436671,
4.8664902382533));
#105173=CARTESIAN_POINT('Ctrl Pts',(-2.75510950644466,-1.25476353616774,
5.02545510443804));
#105174=CARTESIAN_POINT('Ctrl Pts',(-0.436323043355592,-2.99577738259457,
5.1844199706228));
#105175=CARTESIAN_POINT('Ctrl Pts',(2.28274017645734,-1.98850627632914,
5.34338483680754));
#105176=CARTESIAN_POINT('Ctrl Pts',(2.90764896600416,0.842993128505951,
5.50234970299229));
#105177=CARTESIAN_POINT('Ctrl Pts',(0.865120599711097,2.90114223577074,
5.66131456917704));
#105178=CARTESIAN_POINT('Ctrl Pts',(-1.97105750179221,2.29782337198566,
5.82027943536179));
#105179=CARTESIAN_POINT('Ctrl Pts',(-2.99901457040901,-0.413487038115629,
5.97924430154654));
#105180=CARTESIAN_POINT('Ctrl Pts',(-1.27571693477946,-2.74547012850852,
6.13820916773129));
#105181=CARTESIAN_POINT('Ctrl Pts',(1.61790586456557,-2.55879669720352,
6.29717403391604));
#105182=CARTESIAN_POINT('Ctrl Pts',(3.02728408409617,-0.0247183816898012,
6.45613890010078));
#105183=CARTESIAN_POINT('Ctrl Pts',(1.65947353647649,2.53203623709253,6.61510376628553));
#105184=CARTESIAN_POINT('Ctrl Pts',(-1.23071520125009,2.76593564958176,
6.77406863247027));
#105185=CARTESIAN_POINT('Ctrl Pts',(-2.99186274643416,0.462403752920377,
6.93303349865502));
#105186=CARTESIAN_POINT('Ctrl Pts',(-2.00831657228625,-2.26533098457947,
7.09199836483977));
#105187=CARTESIAN_POINT('Ctrl Pts',(0.817631593381527,-2.91488224491483,
7.25096323102452));
#105188=CARTESIAN_POINT('Ctrl Pts',(2.89349578485752,-0.890360638857735,
7.40992809720926));
#105189=CARTESIAN_POINT('Ctrl Pts',(2.31490675414699,1.95096556705137,7.56889296339402));
#105190=CARTESIAN_POINT('Ctrl Pts',(-0.387345882629388,3.00250280456578,
7.72785782957877));
#105191=CARTESIAN_POINT('Ctrl Pts',(-2.7342527360709,1.29958527981204,7.88682269576352));
#105192=CARTESIAN_POINT('Ctrl Pts',(-2.57279374929985,-1.59555389999179,
8.04578756194826));
#105193=CARTESIAN_POINT('Ctrl Pts',(-0.0510891753085383,-3.02695388474646,
8.204752428133));
#105194=CARTESIAN_POINT('Ctrl Pts',(2.51748390518839,-1.68146802269111,
8.36371729431776));
#105195=CARTESIAN_POINT('Ctrl Pts',(2.77655188845945,1.2065734685081,8.52268216050249));
#105196=CARTESIAN_POINT('Ctrl Pts',(0.488449371099479,2.98772106062261,
8.68164702668726));
#105197=CARTESIAN_POINT('Ctrl Pts',(-2.24774987886168,2.0279744589843,8.84061189287199));
#105198=CARTESIAN_POINT('Ctrl Pts',(-2.9218943161501,-0.792208008963017,
8.99957675905675));
#105199=CARTESIAN_POINT('Ctrl Pts',(-0.915533109372039,-2.88562974926773,
9.1585416252415));
#105200=CARTESIAN_POINT('Ctrl Pts',(1.93072557536648,-2.33181446020929,
9.31750649142625));
#105201=CARTESIAN_POINT('Ctrl Pts',(3.00576318160537,0.361175331827897,
9.476471357611));
#105202=CARTESIAN_POINT('Ctrl Pts',(1.32335500053861,2.72282784376186,9.63543622379573));
#105203=CARTESIAN_POINT('Ctrl Pts',(-1.57308085033148,2.58659555449547,
9.79440108998049));
#105204=CARTESIAN_POINT('Ctrl Pts',(-3.02639397271004,0.0774560918177764,
9.95336595616523));
#105205=CARTESIAN_POINT('Ctrl Pts',(-1.70333490387714,-2.50274052379573,
10.11233082235));
#105206=CARTESIAN_POINT('Ctrl Pts',(1.18234017003909,-2.78695741742269,
10.2712956885347));
#105207=CARTESIAN_POINT('Ctrl Pts',(2.98335263946653,-0.51445792131468,
10.4302605547195));
#105208=CARTESIAN_POINT('Ctrl Pts',(2.04747844460581,2.2299981935172,10.5892254209042));
#105209=CARTESIAN_POINT('Ctrl Pts',(-0.766724304622935,2.92868464757063,
10.748190287089));
#105210=CARTESIAN_POINT('Ctrl Pts',(-2.87754472594713,0.940636100938752,
10.9071551532737));
#105211=CARTESIAN_POINT('Ctrl Pts',(-2.34854520706281,-1.91033906273146,
11.0661200194585));
#105212=CARTESIAN_POINT('Ctrl Pts',(0.334977371769763,-3.0087954541008,
11.2250848856432));
#105213=CARTESIAN_POINT('Ctrl Pts',(2.71119631860565,-1.34702429309741,
11.384049751828));
#105214=CARTESIAN_POINT('Ctrl Pts',(2.60020106538442,1.55048842104322,11.5430146180127));
#105215=CARTESIAN_POINT('Ctrl Pts',(0.103817130256965,3.02560439047814,
11.7019794841975));
#105216=CARTESIAN_POINT('Ctrl Pts',(-2.48780721177585,1.72507252057746,
11.8609443503822));
#105217=CARTESIAN_POINT('Ctrl Pts',(-2.79715144680568,-1.15801714488529,
12.019909216567));
#105218=CARTESIAN_POINT('Ctrl Pts',(-0.540427429801531,-2.97875781448132,
12.1788740827517));
#105219=CARTESIAN_POINT('Ctrl Pts',(2.21207727570474,-2.06682704901162,
12.3378389489365));
#105220=CARTESIAN_POINT('Ctrl Pts',(2.93525272386455,0.741182414295655,
12.4968038151212));
#105221=CARTESIAN_POINT('Ctrl Pts',(0.965667708515435,2.86924132846054,
12.655768681306));
#105222=CARTESIAN_POINT('Ctrl Pts',(-1.88980757625962,2.36509772502683,
12.8147335474907));
#105223=CARTESIAN_POINT('Ctrl Pts',(-3.01159939193577,-0.308753990593601,
12.9736984136755));
#105224=CARTESIAN_POINT('Ctrl Pts',(-1.37059136124803,-2.69935904330781,
13.1326632798602));
#105225=CARTESIAN_POINT('Ctrl Pts',(1.5277783266453,-2.61360924945721,13.2916281460449));
#105226=CARTESIAN_POINT('Ctrl Pts',(3.02458519797139,-0.130170290111654,
13.4505930122297));
#105227=CARTESIAN_POINT('Ctrl Pts',(1.74667922314479,2.47268510240381,13.6095578784144));
#105228=CARTESIAN_POINT('Ctrl Pts',(-1.13360623889827,2.80713320299311,
13.7685227445992));
#105229=CARTESIAN_POINT('Ctrl Pts',(-2.97393693436389,0.566355925758412,
13.9274876107839));
#105230=CARTESIAN_POINT('Ctrl Pts',(-2.08601880385432,-2.19398848542593,
14.0864524769687));
#105231=CARTESIAN_POINT('Ctrl Pts',(0.715584276331253,-2.94159804658673,
14.2454173431534));
#105232=CARTESIAN_POINT('Ctrl Pts',(2.86072018694497,-0.990626032476896,
14.4043822093382));
#105233=CARTESIAN_POINT('Ctrl Pts',(2.38147075794636,1.86913267406616,14.5633470755229));
#105234=CARTESIAN_POINT('Ctrl Pts',(-0.282507178367135,3.0141747823221,
14.7223119417077));
#105235=CARTESIAN_POINT('Ctrl Pts',(-2.68731691618803,1.39405441650785,
14.8812768078924));
#105236=CARTESIAN_POINT('Ctrl Pts',(-2.62681908917938,-1.5049522905854,
15.0402416740772));
#105237=CARTESIAN_POINT('Ctrl Pts',(-0.156513571465329,-3.02333647253536,
15.1992065402619));
#105238=CARTESIAN_POINT('Ctrl Pts',(2.45737534328226,-1.76815337186677,
15.3581714064467));
#105239=CARTESIAN_POINT('Ctrl Pts',(2.81690192847887,1.1091093045987,15.5171362726314));
#105240=CARTESIAN_POINT('Ctrl Pts',(0.592241441496159,2.96889036496633,
15.6761011388162));
#105241=CARTESIAN_POINT('Ctrl Pts',(-2.17573319542207,2.10505225268967,
15.8350660050009));
#105242=CARTESIAN_POINT('Ctrl Pts',(-2.94772013419658,-0.689931833348374,
15.9940308711857));
#105243=CARTESIAN_POINT('Ctrl Pts',(-1.01550917875938,-2.85198194806187,
16.1529957373704));
#105244=CARTESIAN_POINT('Ctrl Pts',(1.84831592514999,-2.39766306328732,
16.3119606035552));
#105245=CARTESIAN_POINT('Ctrl Pts',(3.0165214298158,0.256238926936299,16.4709254697399));
#105246=CARTESIAN_POINT('Ctrl Pts',(1.41741167828759,2.67507085111204,16.6298903359247));
#105247=CARTESIAN_POINT('Ctrl Pts',(-1.48201204510996,2.63982958206858,
16.7888552021094));
#105248=CARTESIAN_POINT('Ctrl Pts',(-3.02185830893466,0.182844975151096,
16.9478200682941));
#105249=CARTESIAN_POINT('Ctrl Pts',(-1.7894933370904,-2.44187909625444,
17.1067849344789));
#105250=CARTESIAN_POINT('Ctrl Pts',(1.08452820103594,-2.82645688192358,
17.2657498006636));
#105251=CARTESIAN_POINT('Ctrl Pts',(2.96361848926806,-0.618082012587279,
17.4247146668484));
#105252=CARTESIAN_POINT('Ctrl Pts',(2.12392595108712,2.15731279106996,17.5836795330331));
#105253=CARTESIAN_POINT('Ctrl Pts',(-0.664227032086787,2.95361852209465,
17.7426443992179));
#105254=CARTESIAN_POINT('Ctrl Pts',(-2.84302727494801,1.04031525900428,
17.9016092654026));
#105255=CARTESIAN_POINT('Ctrl Pts',(-2.41367341223081,-1.82735890927465,
18.0605741315874));
#105256=CARTESIAN_POINT('Ctrl Pts',(0.229951229774008,-3.01863915633199,
18.2195389977721));
#105257=CARTESIAN_POINT('Ctrl Pts',(2.66262177742226,-1.44066137402666,
18.3785038639569));
#105258=CARTESIAN_POINT('Ctrl Pts',(2.65263974077067,1.45895933113273,18.5374687301416));
#105259=CARTESIAN_POINT('Ctrl Pts',(0.209162502903596,3.02015081934562,
18.6964335963264));
#105260=CARTESIAN_POINT('Ctrl Pts',(-2.42619753731628,1.81069749934597,
18.8553984625111));
#105261=CARTESIAN_POINT('Ctrl Pts',(-2.83579733821026,-1.0598647936472,
19.0143633286959));
#105262=CARTESIAN_POINT('Ctrl Pts',(-0.643875678016031,-2.95812170734611,
19.1733281948806));
#105263=CARTESIAN_POINT('Ctrl Pts',(2.13872867027862,-2.14263846674061,
19.3322930610654));
#105264=CARTESIAN_POINT('Ctrl Pts',(2.95929276265433,0.63847182326205,19.4912579272501));
#105265=CARTESIAN_POINT('Ctrl Pts',(1.06504239070805,2.8338568471607,19.6502227934348));
#105266=CARTESIAN_POINT('Ctrl Pts',(-1.80626321686095,2.42950058977487,
19.8091876596196));
#105267=CARTESIAN_POINT('Ctrl Pts',(-3.02052780113442,-0.203646081844827,
19.9681525258043));
#105268=CARTESIAN_POINT('Ctrl Pts',(-1.46380173937327,-2.6499706398368,
20.1271173919891));
#105269=CARTESIAN_POINT('Ctrl Pts',(1.43579589818991,-2.66524859319272,
20.2860822581738));
#105270=CARTESIAN_POINT('Ctrl Pts',(3.01821413318115,-0.235464157399701,
20.4450471243586));
#105271=CARTESIAN_POINT('Ctrl Pts',(1.83176424978813,2.41033185631518,20.6040119905434));
#105272=CARTESIAN_POINT('Ctrl Pts',(-1.03512095472343,2.8449225889039,20.7629768567281));
#105273=CARTESIAN_POINT('Ctrl Pts',(-2.95240043518508,0.669620479555379,
20.9219417229129));
#105274=CARTESIAN_POINT('Ctrl Pts',(-2.16118838179135,-2.11998224190941,
21.0809065890976));
#105275=CARTESIAN_POINT('Ctrl Pts',(0.612668165643748,-2.96474242806914,
21.2398714552823));
#105276=CARTESIAN_POINT('Ctrl Pts',(2.82447135255811,-1.08968869199482,
21.3988363214671));
#105277=CARTESIAN_POINT('Ctrl Pts',(2.44514341022872,1.78503043861445,21.5578011876518));
#105278=CARTESIAN_POINT('Ctrl Pts',(-0.177325508855966,3.0221872404181,
21.7167660538366));
#105279=CARTESIAN_POINT('Ctrl Pts',(-2.63711834224907,1.4868309809588,21.8757309200213));
#105280=CARTESIAN_POINT('Ctrl Pts',(-2.67765528972552,-1.41252343298867,
22.0346957862061));
#105281=CARTESIAN_POINT('Ctrl Pts',(-0.261747737865253,-3.01604853322711,
22.1936606523908));
#105282=CARTESIAN_POINT('Ctrl Pts',(2.39428286638798,-1.85269173041736,
22.3526255185756));
#105283=CARTESIAN_POINT('Ctrl Pts',(2.85383268770837,1.01029806712227,22.5115903847603));
#105284=CARTESIAN_POINT('Ctrl Pts',(0.695313038955047,2.94645605177694,
22.6705552509451));
#105285=CARTESIAN_POINT('Ctrl Pts',(-2.10107220926576,2.17957248487984,
22.8295201171298));
#105286=CARTESIAN_POINT('Ctrl Pts',(-2.96997229594661,-0.586814574364468,
22.9884849833146));
#105287=CARTESIAN_POINT('Ctrl Pts',(-1.11424238262265,-2.81487807617514,
23.1474498494993));
#105288=CARTESIAN_POINT('Ctrl Pts',(1.76364326814073,-2.46058813916154,
23.3064147156841));
#105289=CARTESIAN_POINT('Ctrl Pts',(3.02365346187921,0.150967555626084,
23.4653795818688));
#105290=CARTESIAN_POINT('Ctrl Pts',(1.50967841044511,2.62411158555409,23.6243444480536));
#105291=CARTESIAN_POINT('Ctrl Pts',(-1.38901209123598,2.68977159567244,
23.7833093142383));
#105292=CARTESIAN_POINT('Ctrl Pts',(-3.01390546101515,0.288177925768345,
23.942274180423));
#105293=CARTESIAN_POINT('Ctrl Pts',(-1.87299835719334,-2.37837027682274,
24.1012390466078));
#105294=CARTESIAN_POINT('Ctrl Pts',(0.984478956028511,-2.8619162328104,
24.2602039127925));
#105295=CARTESIAN_POINT('Ctrl Pts',(2.94206776414501,-0.722141341305858,
24.4191687789773));
#105296=CARTESIAN_POINT('Ctrl Pts',(2.19405749939855,2.08494186946522,24.5781596741486));
#105297=CARTESIAN_POINT('Ctrl Pts',(0.362372204523541,2.67417657512423,
24.6841622805916));
#105298=CARTESIAN_POINT('Ctrl Pts',(-0.475611217151184,2.51571727802135,
24.7371765983065));
#105299=CARTESIAN_POINT('Ctrl Pts',(-1.2056025718497,2.47504930785831,-0.109118726626311));
#105300=CARTESIAN_POINT('Ctrl Pts',(-2.02982487930536,2.07358624259213,
-0.0561187937304326));
#105301=CARTESIAN_POINT('Ctrl Pts',(-3.23106424626307,0.389505550752776,
0.0498694278936948));
#105302=CARTESIAN_POINT('Ctrl Pts',(-2.07413643060294,-2.51182590505037,
0.208845938246073));
#105303=CARTESIAN_POINT('Ctrl Pts',(0.988263431842728,-3.10071387747958,
0.36781080443082));
#105304=CARTESIAN_POINT('Ctrl Pts',(3.14262081982585,-0.849006636554098,
0.526775670615569));
#105305=CARTESIAN_POINT('Ctrl Pts',(2.41472336408983,2.18361883296827,0.685740536800315));
#105306=CARTESIAN_POINT('Ctrl Pts',(-0.528796535833263,3.21195037198289,
0.844705402985064));
#105307=CARTESIAN_POINT('Ctrl Pts',(-2.98700232399185,1.29424413980195,
1.00367026916981));
#105308=CARTESIAN_POINT('Ctrl Pts',(-2.70507984550533,-1.81107786280241,
1.16263513535456));
#105309=CARTESIAN_POINT('Ctrl Pts',(0.0585014887978986,-3.25478794493359,
1.32160000153931));
#105310=CARTESIAN_POINT('Ctrl Pts',(2.76838511939756,-1.71268102288631,
1.48056486772406));
#105311=CARTESIAN_POINT('Ctrl Pts',(2.93860564946843,1.4006581658271,1.6395297339088));
#105312=CARTESIAN_POINT('Ctrl Pts',(0.412981763758567,3.22903068671821,
1.79849460009355));
#105313=CARTESIAN_POINT('Ctrl Pts',(-2.49150170638785,2.09514647964018,
1.9574594662783));
#105314=CARTESIAN_POINT('Ctrl Pts',(-3.11031799298164,-0.960802356080768,
2.11642433246304));
#105315=CARTESIAN_POINT('Ctrl Pts',(-0.875770193372517,-3.13532114754331,
2.2753891986478));
#105316=CARTESIAN_POINT('Ctrl Pts',(2.16219652790641,-2.43354112327336,
2.43435406483254));
#105317=CARTESIAN_POINT('Ctrl Pts',(3.2165942200981,0.500736918265847,2.59331893101729));
#105318=CARTESIAN_POINT('Ctrl Pts',(1.3201324652309,2.97564534306413,2.75228379720204));
#105319=CARTESIAN_POINT('Ctrl Pts',(-1.7874005630293,2.7207379108714,2.91124866338679));
#105320=CARTESIAN_POINT('Ctrl Pts',(-3.25519695263632,-0.0301371723654253,
3.07021352957154));
#105321=CARTESIAN_POINT('Ctrl Pts',(-1.73672042145277,-2.75336476256983,
3.22917839575628));
#105322=CARTESIAN_POINT('Ctrl Pts',(1.37499951681013,-2.95069343685326,
3.38814326194103));
#105323=CARTESIAN_POINT('Ctrl Pts',(3.22531382314573,-0.441096531933247,
3.54710812812578));
#105324=CARTESIAN_POINT('Ctrl Pts',(2.11676960093958,2.4731562530002,3.70607299431053));
#105325=CARTESIAN_POINT('Ctrl Pts',(-0.933669927301801,3.11856952388404,
3.86503786049528));
#105326=CARTESIAN_POINT('Ctrl Pts',(-3.12757351129378,0.903050018534707,
4.02400272668002));
#105327=CARTESIAN_POINT('Ctrl Pts',(-2.45228418698753,-2.1409151476338,
4.18296759286477));
#105328=CARTESIAN_POINT('Ctrl Pts',(0.472696909874794,-3.22083421435897,
4.34193245904952));
#105329=CARTESIAN_POINT('Ctrl Pts',(2.96403236546465,-1.34600428706288,
4.50089732523426));
#105330=CARTESIAN_POINT('Ctrl Pts',(2.73620531024232,1.7636314536731,4.65986219141902));
#105331=CARTESIAN_POINT('Ctrl Pts',(-0.00177884983542148,3.2553359642495,
4.81882705760376));
#105332=CARTESIAN_POINT('Ctrl Pts',(-2.73813111756831,1.76064005047473,
4.97779192378851));
#105333=CARTESIAN_POINT('Ctrl Pts',(-2.96255957125432,-1.34924282139759,
5.13675678997326));
#105334=CARTESIAN_POINT('Ctrl Pts',(-0.469176635349051,-3.2213488928089,
5.29572165615801));
#105335=CARTESIAN_POINT('Ctrl Pts',(2.45462249055121,-2.13823381163544,
5.45468652234275));
#105336=CARTESIAN_POINT('Ctrl Pts',(3.12658471611875,0.906467548935932,
5.6136513885275));
#105337=CARTESIAN_POINT('Ctrl Pts',(0.930261140970313,3.1195880519624,5.77261625471225));
#105338=CARTESIAN_POINT('Ctrl Pts',(-2.11947120568816,2.4708413977028,5.931581120897));
#105339=CARTESIAN_POINT('Ctrl Pts',(-3.22482982949079,-0.444621159156713,
6.09054598708174));
#105340=CARTESIAN_POINT('Ctrl Pts',(-1.37177393729776,-2.95219438203088,
6.2495108532665));
#105341=CARTESIAN_POINT('Ctrl Pts',(1.7397284910982,-2.75146509728996,6.40847571945124));
#105342=CARTESIAN_POINT('Ctrl Pts',(3.25522793822394,-0.0265795889744855,
6.56744058563598));
#105343=CARTESIAN_POINT('Ctrl Pts',(1.78442606264166,2.7226896685647,6.72640545182074));
#105344=CARTESIAN_POINT('Ctrl Pts',(-1.32338373136274,2.97420088492828,
6.88537031800549));
#105345=CARTESIAN_POINT('Ctrl Pts',(-3.21713949830104,0.497221130700515,
7.04433518419023));
#105346=CARTESIAN_POINT('Ctrl Pts',(-2.15953575326782,-2.43590244769814,
7.20330005037498));
#105347=CARTESIAN_POINT('Ctrl Pts',(0.87919637933312,-3.13436263551479,
7.36226491655974));
#105348=CARTESIAN_POINT('Ctrl Pts',(3.11136585016387,-0.957401666375127,
7.52122978274447));
#105349=CARTESIAN_POINT('Ctrl Pts',(2.48921109851253,2.09786641886127,7.68019464892923));
#105350=CARTESIAN_POINT('Ctrl Pts',(-0.416511666518302,3.22858071542247,
7.83915951511398));
#105351=CARTESIAN_POINT('Ctrl Pts',(-2.94013235935888,1.39743948484165,
7.99812438129872));
#105352=CARTESIAN_POINT('Ctrl Pts',(-2.76651607822568,-1.71569350213334,
8.15708924748347));
#105353=CARTESIAN_POINT('Ctrl Pts',(-0.0549360106898553,-3.25487287602346,
8.31605411366822));
#105354=CARTESIAN_POINT('Ctrl Pts',(2.70704159720282,-1.80807665638305,
8.47501897985296));
#105355=CARTESIAN_POINT('Ctrl Pts',(2.98561648928963,1.29742421097557,8.63398384603771));
#105356=CARTESIAN_POINT('Ctrl Pts',(0.525227892408259,3.21268595810113,
8.79294871222246));
#105357=CARTESIAN_POINT('Ctrl Pts',(-2.41699754649706,2.18067380975948,
8.9519135784072));
#105358=CARTESIAN_POINT('Ctrl Pts',(-3.14190269107475,-0.851858488342414,
9.11087844459197));
#105359=CARTESIAN_POINT('Ctrl Pts',(-0.984469535467015,-3.10290752973419,
9.26984331077669));
#105360=CARTESIAN_POINT('Ctrl Pts',(2.07610242692268,-2.50739189543028,
9.42880817696146));
#105361=CARTESIAN_POINT('Ctrl Pts',(3.23208658739667,0.388370565200701,
9.58777304314619));
#105362=CARTESIAN_POINT('Ctrl Pts',(1.42299898201583,2.92784721280426,9.74673790933095));
#105363=CARTESIAN_POINT('Ctrl Pts',(-1.6915283108004,2.78135711085513,9.90570277551569));
#105364=CARTESIAN_POINT('Ctrl Pts',(-3.25427080457815,0.0832882633629985,
10.0646676417004));
#105365=CARTESIAN_POINT('Ctrl Pts',(-1.83159003688557,-2.69118809099722,
10.2236325078851));
#105366=CARTESIAN_POINT('Ctrl Pts',(1.27136623028387,-2.9968055180204,10.3825973740699));
#105367=CARTESIAN_POINT('Ctrl Pts',(3.20798861018195,-0.553194795064668,
10.5415622402546));
#105368=CARTESIAN_POINT('Ctrl Pts',(2.20164637696432,2.39790922162279,10.7005271064394));
#105369=CARTESIAN_POINT('Ctrl Pts',(-0.82445595061129,3.14920431059108,
10.8594919726241));
#105370=CARTESIAN_POINT('Ctrl Pts',(-3.09421373256705,1.0114626940907,11.0184568388089));
#105371=CARTESIAN_POINT('Ctrl Pts',(-2.52538240873262,-2.05418088152127,
11.1774217049936));
#105372=CARTESIAN_POINT('Ctrl Pts',(0.360199990805737,-3.23534717935607,
11.3363865711784));
#105373=CARTESIAN_POINT('Ctrl Pts',(2.91533987467515,-1.44845048913411,
11.4953514373631));
#105374=CARTESIAN_POINT('Ctrl Pts',(2.79598706890637,1.66723475097302,11.6543163035479));
#105375=CARTESIAN_POINT('Ctrl Pts',(0.111634195368079,3.25342176957865,
11.8132811697326));
#105376=CARTESIAN_POINT('Ctrl Pts',(-2.67513035305559,1.85496441974084,
11.9722460359174));
#105377=CARTESIAN_POINT('Ctrl Pts',(-3.0077671219957,-1.24521176680332,
12.1312109021021));
#105378=CARTESIAN_POINT('Ctrl Pts',(-0.581119716287773,-3.20304781102084,
12.2901757682869));
#105379=CARTESIAN_POINT('Ctrl Pts',(2.37863892167038,-2.22245186329391,
12.4491406344716));
#105380=CARTESIAN_POINT('Ctrl Pts',(3.15626693995073,0.79699084569259,12.6081055006564));
#105381=CARTESIAN_POINT('Ctrl Pts',(1.03837909376074,3.08528511842656,12.7670703668411));
#105382=CARTESIAN_POINT('Ctrl Pts',(-2.03210344626256,2.54318127313638,
12.9260352330259));
#105383=CARTESIAN_POINT('Ctrl Pts',(-3.23836224385742,-0.332002081171888,
13.0850000992106));
#105384=CARTESIAN_POINT('Ctrl Pts',(-1.47379207470547,-2.90261129414173,
13.2439649653954));
#105385=CARTESIAN_POINT('Ctrl Pts',(1.64281466626666,-2.81040484212558,
13.4029298315801));
#105386=CARTESIAN_POINT('Ctrl Pts',(3.25232583545743,-0.139971655558927,
13.5618946977649));
#105387=CARTESIAN_POINT('Ctrl Pts',(1.87819803108888,2.65886960198457,13.7208595639496));
#105388=CARTESIAN_POINT('Ctrl Pts',(-1.21896280537159,3.01850046934971,
13.8798244301343));
#105389=CARTESIAN_POINT('Ctrl Pts',(-3.1978639355704,0.609000536881513,
14.0387892963191));
#105390=CARTESIAN_POINT('Ctrl Pts',(-2.24308868983942,-2.35918810904475,
14.1977541625039));
#105391=CARTESIAN_POINT('Ctrl Pts',(0.769465257887335,-3.16309004317742,
14.3567190286886));
#105392=CARTESIAN_POINT('Ctrl Pts',(3.07612236489684,-1.06521669181684,
14.5156838948734));
#105393=CARTESIAN_POINT('Ctrl Pts',(2.56078713790247,2.00987179658232,14.6746487610581));
#105394=CARTESIAN_POINT('Ctrl Pts',(-0.303778976211977,3.24113155209031,
14.8336136272429));
#105395=CARTESIAN_POINT('Ctrl Pts',(-2.88966243716399,1.49902181558082,
14.9925784934276));
#105396=CARTESIAN_POINT('Ctrl Pts',(-2.8246093363615,-1.61826990989858,
15.1515433596124));
#105397=CARTESIAN_POINT('Ctrl Pts',(-0.168298493432347,-3.2509830853839,
15.3105082257971));
#105398=CARTESIAN_POINT('Ctrl Pts',(2.64240707179728,-1.90128910775282,
15.4694730919818));
#105399=CARTESIAN_POINT('Ctrl Pts',(3.02900474553876,1.19262133799767,15.6284379581666));
#105400=CARTESIAN_POINT('Ctrl Pts',(0.636835140996644,3.19243737723006,
15.7874028243514));
#105401=CARTESIAN_POINT('Ctrl Pts',(-2.33955825984986,2.2635552904915,15.9463676905361));
#105402=CARTESIAN_POINT('Ctrl Pts',(-3.16967310247223,-0.741881276086534,
16.1053325567208));
#105403=CARTESIAN_POINT('Ctrl Pts',(-1.0919734515789,-3.06672616733066,
16.2642974229056));
#105404=CARTESIAN_POINT('Ctrl Pts',(1.98748761961958,-2.57819866693835,
16.4232622890903));
#105405=CARTESIAN_POINT('Ctrl Pts',(3.24365489389454,0.275532817750943,
16.5822271552751));
#105406=CARTESIAN_POINT('Ctrl Pts',(1.52413779709881,2.87649428641854,16.7411920214598));
#105407=CARTESIAN_POINT('Ctrl Pts',(-1.5936023445473,2.83859947364843,16.9001568876446));
#105408=CARTESIAN_POINT('Ctrl Pts',(-3.24939362125808,0.196612559291201,
17.0591217538293));
#105409=CARTESIAN_POINT('Ctrl Pts',(-1.92423589737249,-2.62574401181966,
17.2180866200141));
#105410=CARTESIAN_POINT('Ctrl Pts',(1.16618936371082,-3.03927915340325,
17.3770514861988));
#105411=CARTESIAN_POINT('Ctrl Pts',(3.18676854781625,-0.664621416291182,
17.5360163523836));
#105412=CARTESIAN_POINT('Ctrl Pts',(2.28385011205904,2.31975086377646,17.6949812185683));
#105413=CARTESIAN_POINT('Ctrl Pts',(-0.714240993612621,3.176015618253,17.8539460847531));
#105414=CARTESIAN_POINT('Ctrl Pts',(-3.05709723879664,1.11864734250153,
18.0129109509378));
#105415=CARTESIAN_POINT('Ctrl Pts',(-2.59541453889942,-1.9649526140885,
18.1718758171225));
#105416=CARTESIAN_POINT('Ctrl Pts',(0.247265749363208,-3.24593207777605,
18.3308406833073));
#105417=CARTESIAN_POINT('Ctrl Pts',(2.86310784122402,-1.54913811323122,
18.4898055494921));
#105418=CARTESIAN_POINT('Ctrl Pts',(2.85237419228788,1.56881384221122,18.6487704156768));
#105419=CARTESIAN_POINT('Ctrl Pts',(0.224911704407769,3.24755756370285,
18.8077352818615));
#105420=CARTESIAN_POINT('Ctrl Pts',(-2.60888168659601,1.94703665853776,
18.9667001480463));
#105421=CARTESIAN_POINT('Ctrl Pts',(-3.04932291322741,-1.13966888840907,
19.125665014231));
#105422=CARTESIAN_POINT('Ctrl Pts',(-0.692357254091794,-3.18085787753041,
19.2846298804158));
#105423=CARTESIAN_POINT('Ctrl Pts',(2.29976742399123,-2.30397161438838,
19.4435947466005));
#105424=CARTESIAN_POINT('Ctrl Pts',(3.18211710918843,0.686546508063173,
19.6025596127853));
#105425=CARTESIAN_POINT('Ctrl Pts',(1.1452363403353,3.04723631002041,19.76152447897));
#105426=CARTESIAN_POINT('Ctrl Pts',(-1.94226849016302,2.61243344729831,
19.9204893451548));
#105427=CARTESIAN_POINT('Ctrl Pts',(-3.24796293089569,-0.218979916227147,
20.0794542113395));
#105428=CARTESIAN_POINT('Ctrl Pts',(-1.57402086677678,-2.84950411743251,
20.2384190775243));
#105429=CARTESIAN_POINT('Ctrl Pts',(1.54390628416051,-2.86593244699177,
20.397383943709));
#105430=CARTESIAN_POINT('Ctrl Pts',(3.2454750518754,-0.253193781067517,
20.5563488098938));
#105431=CARTESIAN_POINT('Ctrl Pts',(1.96968966126294,2.59182137556506,20.7153136760785));
#105432=CARTESIAN_POINT('Ctrl Pts',(-1.11306192536034,3.05913526323357,
20.8742785422633));
#105433=CARTESIAN_POINT('Ctrl Pts',(-3.17470581367933,0.720040548723835,
21.033243408448));
#105434=CARTESIAN_POINT('Ctrl Pts',(-2.32391827286092,-2.27960945543785,
21.1922082746328));
#105435=CARTESIAN_POINT('Ctrl Pts',(0.658799925696245,-3.18797711525971,
21.3511731408175));
#105436=CARTESIAN_POINT('Ctrl Pts',(3.03714412065341,-1.17173842150571,
21.5101380070023));
#105437=CARTESIAN_POINT('Ctrl Pts',(2.6292541171659,1.91943695832324,21.669102873187));
#105438=CARTESIAN_POINT('Ctrl Pts',(-0.190677496578619,3.24974732012642,
21.8280677393718));
#105439=CARTESIAN_POINT('Ctrl Pts',(-2.83568408699738,1.59878412933253,
21.9870326055565));
#105440=CARTESIAN_POINT('Ctrl Pts',(-2.87927332417827,-1.51888148410543,
22.1459974717412));
#105441=CARTESIAN_POINT('Ctrl Pts',(-0.281456422785714,-3.24314638985442,
22.304962337926));
#105442=CARTESIAN_POINT('Ctrl Pts',(2.57456395308999,-1.99219290764765,
22.4639272041107));
#105443=CARTESIAN_POINT('Ctrl Pts',(3.06871626116932,1.08636996154657,22.6228920702955));
#105444=CARTESIAN_POINT('Ctrl Pts',(0.747667667566643,3.16831383908819,
22.7818569364802));
#105445=CARTESIAN_POINT('Ctrl Pts',(-2.25927556378304,2.3436866343131,22.940821802665));
#105446=CARTESIAN_POINT('Ctrl Pts',(-3.1936007738114,-0.630999649839126,
23.0997866688497));
#105447=CARTESIAN_POINT('Ctrl Pts',(-1.19814091875997,-3.02682850426808,
23.2587515350345));
#105448=CARTESIAN_POINT('Ctrl Pts',(1.89643940906404,-2.64586177991698,
23.4177164012192));
#105449=CARTESIAN_POINT('Ctrl Pts',(3.25132394291147,0.16233488208827,23.576681267404));
#105450=CARTESIAN_POINT('Ctrl Pts',(1.62335188997686,2.82169796722699,23.7356461335887));
#105451=CARTESIAN_POINT('Ctrl Pts',(-1.49359982093395,2.8923019453882,23.8946109997735));
#105452=CARTESIAN_POINT('Ctrl Pts',(-3.24084195183531,0.309876710966349,
24.0535758659582));
#105453=CARTESIAN_POINT('Ctrl Pts',(-2.01402855206554,-2.55745320144486,
24.212540732143));
#105454=CARTESIAN_POINT('Ctrl Pts',(1.05860676211178,-3.0774084688132,24.3715055983277));
#105455=CARTESIAN_POINT('Ctrl Pts',(3.16359512881733,-0.776516046813999,
24.5304704645125));
#105456=CARTESIAN_POINT('Ctrl Pts',(2.35926231952699,2.24193066607503,24.6894613596838));
#105457=CARTESIAN_POINT('Ctrl Pts',(0.389657558204677,2.87553267459119,
24.7954639661269));
#105458=CARTESIAN_POINT('Ctrl Pts',(-0.511423070578954,2.70514194921774,
24.8484782838417));
#105459=CARTESIAN_POINT('Ctrl Pts',(-1.29002360226262,2.64836198798272,
0.00218295890889542));
#105460=CARTESIAN_POINT('Ctrl Pts',(-2.17196119509458,2.21878690103223,
0.0551828918047738));
#105461=CARTESIAN_POINT('Ctrl Pts',(-3.45731606371014,0.416780260274697,
0.161171113428902));
#105462=CARTESIAN_POINT('Ctrl Pts',(-2.21937561536994,-2.68771382705179,
0.320147623781279));
#105463=CARTESIAN_POINT('Ctrl Pts',(1.05746552147296,-3.31783804979352,
0.479112489966027));
#105464=CARTESIAN_POINT('Ctrl Pts',(3.36267948094808,-0.908457418062733,
0.638077356150774));
#105465=CARTESIAN_POINT('Ctrl Pts',(2.58381178453491,2.33652440584326,0.797042222335523));
#105466=CARTESIAN_POINT('Ctrl Pts',(-0.565824947580382,3.43686376083034,
0.956007088520271));
#105467=CARTESIAN_POINT('Ctrl Pts',(-3.1961639664146,1.3848722011873,1.11497195470501));
#105468=CARTESIAN_POINT('Ctrl Pts',(-2.89450016795568,-1.93789665276337,
1.27393682088976));
#105469=CARTESIAN_POINT('Ctrl Pts',(0.0625979929696191,-3.48270098900187,
1.43290168707451));
#105470=CARTESIAN_POINT('Ctrl Pts',(2.96223832593208,-1.83260967939114,
1.59186655325927));
#105471=CARTESIAN_POINT('Ctrl Pts',(3.14437836652949,1.49873775554959,1.75083141944401));
#105472=CARTESIAN_POINT('Ctrl Pts',(0.441900369982786,3.45514010633353,
1.90979628562875));
#105473=CARTESIAN_POINT('Ctrl Pts',(-2.66596644811953,2.24185687061573,
2.0687611518135));
#105474=CARTESIAN_POINT('Ctrl Pts',(-3.32811468320972,-1.02808151325697,
2.22772601799825));
#105475=CARTESIAN_POINT('Ctrl Pts',(-0.937095064317323,-3.35486865692271,
2.38669088418301));
#105476=CARTESIAN_POINT('Ctrl Pts',(2.31360202678571,-2.60394723717516,
2.54565575036775));
#105477=CARTESIAN_POINT('Ctrl Pts',(3.44183278944212,0.535800485309293,
2.70462061655249));
#105478=CARTESIAN_POINT('Ctrl Pts',(1.41257332891064,3.18401172504641,2.86358548273725));
#105479=CARTESIAN_POINT('Ctrl Pts',(-1.91256137540221,2.91125467259897,
3.022550348922));
#105480=CARTESIAN_POINT('Ctrl Pts',(-3.48313863703146,-0.0322474956213979,
3.18151521510675));
#105481=CARTESIAN_POINT('Ctrl Pts',(-1.85833241112631,-2.94616618468535,
3.34048008129148));
#105482=CARTESIAN_POINT('Ctrl Pts',(1.47128238708329,-3.15731258829517,
3.49944494747623));
#105483=CARTESIAN_POINT('Ctrl Pts',(3.45116297336547,-0.471983844723412,
3.65840981366099));
#105484=CARTESIAN_POINT('Ctrl Pts',(2.26499412785301,2.64633637398326,3.81737467984574));
#105485=CARTESIAN_POINT('Ctrl Pts',(-0.999049165177388,3.33694401873657,
3.97633954603049));
#105486=CARTESIAN_POINT('Ctrl Pts',(-3.34657850073276,0.966285130054183,
4.13530441221522));
#105487=CARTESIAN_POINT('Ctrl Pts',(-2.62400276387572,-2.29083044062507,
4.29426927839998));
#105488=CARTESIAN_POINT('Ctrl Pts',(0.505797005326167,-3.44636968476542,
4.45323414458472));
#105489=CARTESIAN_POINT('Ctrl Pts',(3.17158556111339,-1.4402567973903,4.61219901076946));
#105490=CARTESIAN_POINT('Ctrl Pts',(2.92780516006474,1.8871278595901,4.77116387695423));
#105491=CARTESIAN_POINT('Ctrl Pts',(-0.00190341189225514,3.48328738278414,
4.93012874313896));
#105492=CARTESIAN_POINT('Ctrl Pts',(-2.92986581998863,1.88392698658276,
5.08909360932372));
#105493=CARTESIAN_POINT('Ctrl Pts',(-3.17000963606399,-1.44372210662744,
5.24805847550846));
#105494=CARTESIAN_POINT('Ctrl Pts',(-0.502030227342508,-3.44692040302324,
5.4070233416932));
#105495=CARTESIAN_POINT('Ctrl Pts',(2.62650480464509,-2.28796134694173,
5.56598820787796));
#105496=CARTESIAN_POINT('Ctrl Pts',(3.34552046623336,0.969941969365909,
5.72495307406269));
#105497=CARTESIAN_POINT('Ctrl Pts',(0.995401682229525,3.33803386815407,
5.88391794024746));
#105498=CARTESIAN_POINT('Ctrl Pts',(-2.26788490958412,2.64385942341994,
6.0428828064322));
#105499=CARTESIAN_POINT('Ctrl Pts',(-3.45064508857258,-0.475755280197791,
6.20184767261695));
#105500=CARTESIAN_POINT('Ctrl Pts',(-1.46783093981607,-3.15891863555324,
6.36081253880171));
#105501=CARTESIAN_POINT('Ctrl Pts',(1.86155111763083,-2.94413349737639,
6.51977740498645));
#105502=CARTESIAN_POINT('Ctrl Pts',(3.48317179235171,-0.028440796259172,
6.6787422711712));
#105503=CARTESIAN_POINT('Ctrl Pts',(1.90937858880683,2.91334310003689,6.83770713735594));
#105504=CARTESIAN_POINT('Ctrl Pts',(-1.41605226147539,3.18246612027479,
6.99667200354068));
#105505=CARTESIAN_POINT('Ctrl Pts',(-3.44241625016792,0.53203850848065,
7.15563686972543));
#105506=CARTESIAN_POINT('Ctrl Pts',(-2.31075493424938,-2.60647391081679,
7.31460173591018));
#105507=CARTESIAN_POINT('Ctrl Pts',(0.940761165284715,-3.35384302611475,
7.47356660209493));
#105508=CARTESIAN_POINT('Ctrl Pts',(3.3292359154702,-1.02444269389252,7.63253146827967));
#105509=CARTESIAN_POINT('Ctrl Pts',(2.66351544287808,2.24476727067117,7.79149633446445));
#105510=CARTESIAN_POINT('Ctrl Pts',(-0.44567745040722,3.45465862627915,
7.95046120064917));
#105511=CARTESIAN_POINT('Ctrl Pts',(-3.14601198264685,1.49529368987125,
8.10942606683394));
#105512=CARTESIAN_POINT('Ctrl Pts',(-2.96023840715151,-1.83583310427489,
8.26839093301866));
#105513=CARTESIAN_POINT('Ctrl Pts',(-0.0587828460711719,-3.48279186730046,
8.42735579920343));
#105514=CARTESIAN_POINT('Ctrl Pts',(2.89659928921725,-1.93468529007499,
8.58632066538816));
#105515=CARTESIAN_POINT('Ctrl Pts',(3.19468109011983,1.38827495344303,8.74528553157291));
#105516=CARTESIAN_POINT('Ctrl Pts',(0.56200641371704,3.43765085557963,8.90425039775766));
#105517=CARTESIAN_POINT('Ctrl Pts',(-2.58624521413244,2.33337316053465,
9.06321526394242));
#105518=CARTESIAN_POINT('Ctrl Pts',(-3.3619110659994,-0.911508967721811,
9.22218013012717));
#105519=CARTESIAN_POINT('Ctrl Pts',(-1.05340596156199,-3.32018531020063,
9.38114499631191));
#105520=CARTESIAN_POINT('Ctrl Pts',(2.22147927847889,-2.68296933065128,
9.54010986249667));
#105521=CARTESIAN_POINT('Ctrl Pts',(3.45840999318797,0.415565798573505,
9.6990747286814));
#105522=CARTESIAN_POINT('Ctrl Pts',(1.52264296349306,3.13286658184666,9.85803959486615));
#105523=CARTESIAN_POINT('Ctrl Pts',(-1.80997577126933,2.9761186672148,10.0170044610509));
#105524=CARTESIAN_POINT('Ctrl Pts',(-3.48214763644626,0.0891204349082218,
10.1759693272357));
#105525=CARTESIAN_POINT('Ctrl Pts',(-1.959845169894,-2.87963565819873,10.3349341934204));
#105526=CARTESIAN_POINT('Ctrl Pts',(1.36039229052865,-3.20665361861812,
10.4938990596052));
#105527=CARTESIAN_POINT('Ctrl Pts',(3.43262458089735,-0.591931668814657,
10.6528639257899));
#105528=CARTESIAN_POINT('Ctrl Pts',(2.35581430932283,2.56582024972839,10.8118287919747));
#105529=CARTESIAN_POINT('Ctrl Pts',(-0.882187596599642,3.36972397361152,
10.9707936581594));
#105530=CARTESIAN_POINT('Ctrl Pts',(-3.31088273918698,1.08228928724265,
11.1297585243441));
#105531=CARTESIAN_POINT('Ctrl Pts',(-2.70221961040245,-2.1980227003111,
11.2887233905289));
#105532=CARTESIAN_POINT('Ctrl Pts',(0.38542260984171,-3.46189890461135,
11.4476882567136));
#105533=CARTESIAN_POINT('Ctrl Pts',(3.11948343074465,-1.54987668517082,
11.6066531228984));
#105534=CARTESIAN_POINT('Ctrl Pts',(2.99177307242833,1.78398108090281,11.7656179890831));
#105535=CARTESIAN_POINT('Ctrl Pts',(0.119451260479191,3.48123914867916,
11.9245828552679));
#105536=CARTESIAN_POINT('Ctrl Pts',(-2.86245349433533,1.9848563189042,12.0835477214526));
#105537=CARTESIAN_POINT('Ctrl Pts',(-3.21838279718572,-1.33240638872134,
12.2425125876374));
#105538=CARTESIAN_POINT('Ctrl Pts',(-0.621812002774014,-3.42733780756036,
12.4014774538221));
#105539=CARTESIAN_POINT('Ctrl Pts',(2.54520056763601,-2.37807667757619,
12.5604423200069));
#105540=CARTESIAN_POINT('Ctrl Pts',(3.37728115603691,0.852799277089526,
12.7194071861916));
#105541=CARTESIAN_POINT('Ctrl Pts',(1.11109047900605,3.30132890839259,12.8783720523764));
#105542=CARTESIAN_POINT('Ctrl Pts',(-2.1743993162655,2.72126482124593,13.0373369185611));
#105543=CARTESIAN_POINT('Ctrl Pts',(-3.46512509577907,-0.355250171750174,
13.1963017847459));
#105544=CARTESIAN_POINT('Ctrl Pts',(-1.57699278816291,-3.10586354497564,
13.3552666509306));
#105545=CARTESIAN_POINT('Ctrl Pts',(1.75785100588802,-3.00720043479395,
13.5142315171154));
#105546=CARTESIAN_POINT('Ctrl Pts',(3.48006647294345,-0.149773021006202,
13.6731963833001));
#105547=CARTESIAN_POINT('Ctrl Pts',(2.00971683903299,2.84505410156533,13.8321612494849));
#105548=CARTESIAN_POINT('Ctrl Pts',(-1.30431937184491,3.22986773570631,
13.9911261156696));
#105549=CARTESIAN_POINT('Ctrl Pts',(-3.42179093677689,0.651645148004609,
14.1500909818544));
#105550=CARTESIAN_POINT('Ctrl Pts',(-2.40015857582453,-2.52438773266358,
14.3090558480391));
#105551=CARTESIAN_POINT('Ctrl Pts',(0.823346239443419,-3.38458203976812,
14.4680207142239));
#105552=CARTESIAN_POINT('Ctrl Pts',(3.29152454284872,-1.13980735115677,
14.6269855804086));
#105553=CARTESIAN_POINT('Ctrl Pts',(2.74010351785857,2.15061091909846,14.7859504465933));
#105554=CARTESIAN_POINT('Ctrl Pts',(-0.325050774056821,3.46808832185853,
14.9449153127781));
#105555=CARTESIAN_POINT('Ctrl Pts',(-3.09200795813995,1.60398921465379,
15.1038801789628));
#105556=CARTESIAN_POINT('Ctrl Pts',(-3.02239958354363,-1.73158752921176,
15.2628450451476));
#105557=CARTESIAN_POINT('Ctrl Pts',(-0.180083415399364,-3.47862969823242,
15.4218099113323));
#105558=CARTESIAN_POINT('Ctrl Pts',(2.82743880031229,-2.03442484363887,
15.5807747775171));
#105559=CARTESIAN_POINT('Ctrl Pts',(3.24110756259866,1.27613337139665,15.7397396437018));
#105560=CARTESIAN_POINT('Ctrl Pts',(0.681428840497123,3.41598438949379,
15.8987045098866));
#105561=CARTESIAN_POINT('Ctrl Pts',(-2.50338332427764,2.42205832829334,
16.0576693760713));
#105562=CARTESIAN_POINT('Ctrl Pts',(-3.39162607074788,-0.793830718824695,
16.2166342422561));
#105563=CARTESIAN_POINT('Ctrl Pts',(-1.16843772439841,-3.28147038659945,
16.3755991084409));
#105564=CARTESIAN_POINT('Ctrl Pts',(2.12665931408915,-2.75873427058938,
16.5345639746256));
#105565=CARTESIAN_POINT('Ctrl Pts',(3.47078835797328,0.294826708565589,
16.6935288408103));
#105566=CARTESIAN_POINT('Ctrl Pts',(1.63086391591002,3.07791772172504,16.8524937069951));
#105567=CARTESIAN_POINT('Ctrl Pts',(-1.70519264398462,3.03736936522827,
17.0114585731798));
#105568=CARTESIAN_POINT('Ctrl Pts',(-3.47692893358152,0.210380143431305,
17.1704234393646));
#105569=CARTESIAN_POINT('Ctrl Pts',(-2.05897845765457,-2.80960892738488,
17.3293883055493));
#105570=CARTESIAN_POINT('Ctrl Pts',(1.24785052638568,-3.25210142488291,
17.4883531717341));
#105571=CARTESIAN_POINT('Ctrl Pts',(3.40991860636443,-0.711160819995082,
17.6473180379188));
#105572=CARTESIAN_POINT('Ctrl Pts',(2.44377427303097,2.48218893648296,17.8062829041036));
#105573=CARTESIAN_POINT('Ctrl Pts',(-0.764254955138454,3.39841271441135,
17.9652477702883));
#105574=CARTESIAN_POINT('Ctrl Pts',(-3.27116720264528,1.19697942599879,
18.1242126364731));
#105575=CARTESIAN_POINT('Ctrl Pts',(-2.77715566556803,-2.10254631890235,
18.2831775026578));
#105576=CARTESIAN_POINT('Ctrl Pts',(0.264580268952404,-3.4732249992201,
18.4421423688426));
#105577=CARTESIAN_POINT('Ctrl Pts',(3.06359390502579,-1.65761485243577,
18.6011072350273));
#105578=CARTESIAN_POINT('Ctrl Pts',(3.05210864380509,1.67866835328972,18.7600721012121));
#105579=CARTESIAN_POINT('Ctrl Pts',(0.240660905911945,3.47496430806008,
18.9190369673968));
#105580=CARTESIAN_POINT('Ctrl Pts',(-2.79156583587576,2.08337581772957,
19.0780018335815));
#105581=CARTESIAN_POINT('Ctrl Pts',(-3.26284848824455,-1.21947298317094,
19.2369666997663));
#105582=CARTESIAN_POINT('Ctrl Pts',(-0.74083883016756,-3.40359404771472,
19.395931565951));
#105583=CARTESIAN_POINT('Ctrl Pts',(2.46080617770385,-2.46530476203616,
19.5548964321358));
#105584=CARTESIAN_POINT('Ctrl Pts',(3.40494145572254,0.734621192864293,
19.7138612983205));
#105585=CARTESIAN_POINT('Ctrl Pts',(1.22543028996257,3.26061577288012,19.8728261645053));
#105586=CARTESIAN_POINT('Ctrl Pts',(-2.07827376346511,2.79536630482174,
20.03179103069));
#105587=CARTESIAN_POINT('Ctrl Pts',(-3.47539806065695,-0.234313750609469,
20.1907558968748));
#105588=CARTESIAN_POINT('Ctrl Pts',(-1.6842399941803,-3.04903759502821,
20.3497207630595));
#105589=CARTESIAN_POINT('Ctrl Pts',(1.6520166701311,-3.06661630079082,20.5086856292443));
#105590=CARTESIAN_POINT('Ctrl Pts',(3.47273597056966,-0.27092340473533,
20.667650495429));
#105591=CARTESIAN_POINT('Ctrl Pts',(2.10761507273776,2.77331089481495,20.8266153616138));
#105592=CARTESIAN_POINT('Ctrl Pts',(-1.19100289599724,3.27334793756324,
20.9855802277985));
#105593=CARTESIAN_POINT('Ctrl Pts',(-3.39701119217357,0.77046061789229,
21.1445450939833));
#105594=CARTESIAN_POINT('Ctrl Pts',(-2.4866481639305,-2.4392366689663,21.303509960168));
#105595=CARTESIAN_POINT('Ctrl Pts',(0.70493168574874,-3.41121180245027,
21.4624748263528));
#105596=CARTESIAN_POINT('Ctrl Pts',(3.2498168887487,-1.2537881510166,21.6214396925375));
#105597=CARTESIAN_POINT('Ctrl Pts',(2.81336482410308,2.05384347803204,21.7804045587223));
#105598=CARTESIAN_POINT('Ctrl Pts',(-0.20402948430127,3.47730739983474,
21.939369424907));
#105599=CARTESIAN_POINT('Ctrl Pts',(-3.03424983174571,1.71073727770627,
22.0983342910918));
#105600=CARTESIAN_POINT('Ctrl Pts',(-3.08089135863104,-1.62523953522219,
22.2572991572765));
#105601=CARTESIAN_POINT('Ctrl Pts',(-0.301165107706183,-3.47024424648171,
22.4162640234613));
#105602=CARTESIAN_POINT('Ctrl Pts',(2.75484503979201,-2.13169408487794,
22.575228889646));
#105603=CARTESIAN_POINT('Ctrl Pts',(3.28359983463026,1.16244185597087,22.7341937558308));
#105604=CARTESIAN_POINT('Ctrl Pts',(0.800022296178244,3.39017162639943,
22.8931586220155));
#105605=CARTESIAN_POINT('Ctrl Pts',(-2.41747891830033,2.50780078374637,
23.0521234882003));
#105606=CARTESIAN_POINT('Ctrl Pts',(-3.4172292516762,-0.675184725313785,
23.211088354385));
#105607=CARTESIAN_POINT('Ctrl Pts',(-1.28203945489728,-3.23877893236102,
23.3700532205698));
#105608=CARTESIAN_POINT('Ctrl Pts',(2.02923554998735,-2.83113542067243,
23.5290180867545));
#105609=CARTESIAN_POINT('Ctrl Pts',(3.47899442394374,0.173702208550458,
23.6879829529393));
#105610=CARTESIAN_POINT('Ctrl Pts',(1.73702536950861,3.0192843488999,23.846947819124));
#105611=CARTESIAN_POINT('Ctrl Pts',(-1.59818755063192,3.09483229510396,
24.0059126853087));
#105612=CARTESIAN_POINT('Ctrl Pts',(-3.46777844265547,0.331575496164351,
24.1648775514935));
#105613=CARTESIAN_POINT('Ctrl Pts',(-2.15505874693774,-2.73653612606696,
24.3238424176782));
#105614=CARTESIAN_POINT('Ctrl Pts',(1.13273456819505,-3.29290070481601,
24.482807283863));
#105615=CARTESIAN_POINT('Ctrl Pts',(3.38512249348965,-0.830890752322139,
24.6417721500477));
#105616=CARTESIAN_POINT('Ctrl Pts',(2.52446713965543,2.39891946268483,24.800763045219));
#105617=CARTESIAN_POINT('Ctrl Pts',(0.41694291188581,3.07688877405814,24.9067656516621));
#105618=CARTESIAN_POINT('Ctrl Pts',(-0.547234924006723,2.89456662041414,
24.9597799693768));
#105619=CARTESIAN_POINT('',(-1.37840024430538,-1.93245649864576,-0.0011160887762519));
#105620=CARTESIAN_POINT('Ctrl Pts',(-1.38000853228519,-1.93376988380877,
2.94035629178069E-16));
#105621=CARTESIAN_POINT('Ctrl Pts',(-1.4297549820204,-1.90670748712375,
-1.0940687484236E-15));
#105622=CARTESIAN_POINT('Ctrl Pts',(-1.47837306283675,-1.87779458035135,
1.7193541140338E-15));
#105623=CARTESIAN_POINT('Ctrl Pts',(-1.52574686801137,-1.84705383051901,
1.33053290607421E-15));
#105624=CARTESIAN_POINT('Ctrl Pts',(-1.59465901921528,-1.80233689902576,
5.8070168986626E-16));
#105625=CARTESIAN_POINT('Ctrl Pts',(-1.66093964424413,-1.75375486097636,
-7.47438015865648E-16));
#105626=CARTESIAN_POINT('Ctrl Pts',(-1.72450125496549,-1.7016761593034,
3.92047505570758E-16));
#105627=CARTESIAN_POINT('Ctrl Pts',(-1.77965763233737,-1.65648421891812,
1.3808502233884E-15));
#105628=CARTESIAN_POINT('Ctrl Pts',(-1.83276652858523,-1.60865813869483,
4.61594664290787E-15));
#105629=CARTESIAN_POINT('Ctrl Pts',(-1.88375802489245,-1.55840962235702,
2.91433543964104E-16));
#105630=CARTESIAN_POINT('Ctrl Pts',(-1.89644826437001,-1.54590428809742,
-8.1504500272814E-16));
#105631=CARTESIAN_POINT('Ctrl Pts',(-1.90900111730879,-1.53325481819968,
-1.74004399250644E-16));
#105632=CARTESIAN_POINT('Ctrl Pts',(-1.92141126720496,-1.52046950431021,
9.71445146547012E-17));
#105633=CARTESIAN_POINT('Ctrl Pts',(-1.98035838488981,-1.45974039073902,
1.67517006871711E-15));
#105634=CARTESIAN_POINT('Ctrl Pts',(-2.03612011880858,-1.39591828314059,
2.73356635213392E-15));
#105635=CARTESIAN_POINT('Ctrl Pts',(-2.08860296990658,-1.32938115129062,
1.77635683940025E-15));
#105636=CARTESIAN_POINT('Ctrl Pts',(-2.1424363494038,-1.26113183566471,
7.94515687876094E-16));
#105637=CARTESIAN_POINT('Ctrl Pts',(-2.19282057211837,-1.19002542991145,
-4.18623297150609E-16));
#105638=CARTESIAN_POINT('Ctrl Pts',(-2.23962715136483,-1.11642291402605,
5.27355936696949E-16));
#105639=CARTESIAN_POINT('Ctrl Pts',(-2.25367989982903,-1.09432521625106,
8.11367467546422E-16));
#105640=CARTESIAN_POINT('Ctrl Pts',(-2.26740994442307,-1.0720022413678,
1.01236449027613E-15));
#105641=CARTESIAN_POINT('Ctrl Pts',(-2.28081320143484,-1.0494630813435,
9.43689570931383E-16));
#105642=CARTESIAN_POINT('Ctrl Pts',(-2.28854016506294,-1.03646927919803,
1.06112055969545E-15));
#105643=CARTESIAN_POINT('Ctrl Pts',(-2.29615841050338,-1.02340363584216,
2.42274131692933E-15));
#105644=CARTESIAN_POINT('Ctrl Pts',(-2.30366012931239,-1.01028056907449,
2.42861286636753E-15));
#105645=CARTESIAN_POINT('Ctrl Pts',(-2.34788758313654,-0.932911656126013,
2.51960496077167E-15));
#105646=CARTESIAN_POINT('Ctrl Pts',(-2.38813169620358,-0.853443126245271,
2.56936708869013E-15));
#105647=CARTESIAN_POINT('Ctrl Pts',(-2.42429183936437,-0.772277775263675,
8.04911692853238E-16));
#105648=CARTESIAN_POINT('Ctrl Pts',(-2.46091595491175,-0.69007098809537,
-9.82183507738202E-16));
#105649=CARTESIAN_POINT('Ctrl Pts',(-2.49335125604467,-0.60612280514716,
-7.94941899479276E-16));
#105650=CARTESIAN_POINT('Ctrl Pts',(-2.52145944991457,-0.520809805332038,
-6.10622663543836E-16));
#105651=CARTESIAN_POINT('Ctrl Pts',(-2.5494808416252,-0.435760264372774,
-4.2687263201004E-16));
#105652=CARTESIAN_POINT('Ctrl Pts',(-2.57320236910088,-0.349353441725185,
5.04520330946943E-16));
#105653=CARTESIAN_POINT('Ctrl Pts',(-2.59244489102332,-0.261933481969527,
-2.77555756156289E-17));
#105654=CARTESIAN_POINT('Ctrl Pts',(-2.60035763856488,-0.225985383563911,
-2.4663358381342E-16));
#105655=CARTESIAN_POINT('Ctrl Pts',(-2.60751246699365,-0.189865704000582,
-9.27455087219583E-16));
#105656=CARTESIAN_POINT('Ctrl Pts',(-2.61389449998738,-0.153597483987339,
-7.7715611723761E-16));
#105657=CARTESIAN_POINT('Ctrl Pts',(-2.61683838977986,-0.136867761218229,
-7.7185221570313E-16));
#105658=CARTESIAN_POINT('Ctrl Pts',(-2.61961782537805,-0.120106427110366,
1.42601103290378E-15));
#105659=CARTESIAN_POINT('Ctrl Pts',(-2.62223123581086,-0.103315720290366,
1.11022302462516E-16));
#105660=CARTESIAN_POINT('Ctrl Pts',(-2.62432314157133,-0.0898755901530302,
-5.34901838098858E-16));
#105661=CARTESIAN_POINT('Ctrl Pts',(-2.62630726224861,-0.0764256097890602,
-1.48813852544152E-15));
#105662=CARTESIAN_POINT('Ctrl Pts',(-2.62818292774977,-0.0629691027470899,
-1.33226762955019E-15));
#105663=CARTESIAN_POINT('Ctrl Pts',(-2.64096297258636,0.0287182280877715,
-5.01642716975331E-16));
#105664=CARTESIAN_POINT('Ctrl Pts',(-2.64871616260283,0.120736677540811,
1.05235300008268E-15));
#105665=CARTESIAN_POINT('Ctrl Pts',(-2.65130675431473,0.212692240506512,
-7.49400541621981E-16));
#105666=CARTESIAN_POINT('Ctrl Pts',(-2.65228201510577,0.247310067262954,
-1.71122277691643E-15));
#105667=CARTESIAN_POINT('Ctrl Pts',(-2.65252517805866,0.28191928532423,
-1.61897482542291E-15));
#105668=CARTESIAN_POINT('Ctrl Pts',(-2.65202733419216,0.316499817063281,
-5.82867087928207E-16));
#105669=CARTESIAN_POINT('Ctrl Pts',(-2.65073859129207,0.406016667142018,
2.28695183531716E-15));
#105670=CARTESIAN_POINT('Ctrl Pts',(-2.64448830078811,0.495340674919477,
9.61036850291248E-16));
#105671=CARTESIAN_POINT('Ctrl Pts',(-2.63352875838965,0.584202228253877,
2.22044604925031E-16));
#105672=CARTESIAN_POINT('Ctrl Pts',(-2.62256921599118,0.673063781588278,
-5.16947640441185E-16));
#105673=CARTESIAN_POINT('Ctrl Pts',(-2.60690015250225,0.761463607059672,
4.96773921778048E-16));
#105674=CARTESIAN_POINT('Ctrl Pts',(-2.58672150741346,0.849135624308466,
-2.27595720048157E-15));
#105675=CARTESIAN_POINT('Ctrl Pts',(-2.58222377673817,0.86867732889812,
-2.64044297795768E-15));
#105676=CARTESIAN_POINT('Ctrl Pts',(-2.57750180222384,0.888182863298944,
1.57927706612469E-15));
#105677=CARTESIAN_POINT('Ctrl Pts',(-2.57255746459196,0.907649247569788,
-4.71844785465692E-16));
#105678=CARTESIAN_POINT('Ctrl Pts',(-2.56909036256595,0.921299597802606,
-1.81456717867258E-15));
#105679=CARTESIAN_POINT('Ctrl Pts',(-2.56551386203416,0.934930611625315,
-6.29501938009571E-17));
#105680=CARTESIAN_POINT('Ctrl Pts',(-2.56183256521565,0.948527398973697,
-2.22044604925031E-16));
#105681=CARTESIAN_POINT('Ctrl Pts',(-2.53769258385253,1.03768787947022,
-1.55526631325667E-15));
#105682=CARTESIAN_POINT('Ctrl Pts',(-2.5090134703751,1.12552579298916,2.14318453916703E-15));
#105683=CARTESIAN_POINT('Ctrl Pts',(-2.4760839832643,1.21175983132397,2.99760216648792E-15));
#105684=CARTESIAN_POINT('Ctrl Pts',(-2.44257162390528,1.29952026536694,
3.86714351321826E-15));
#105685=CARTESIAN_POINT('Ctrl Pts',(-2.40465691530913,1.38562031404822,
-6.57769690187563E-16));
#105686=CARTESIAN_POINT('Ctrl Pts',(-2.3625894351197,1.46976681490133,-1.63757896132211E-15));
#105687=CARTESIAN_POINT('Ctrl Pts',(-2.31999722978461,1.55496290999486,
-2.62960980028503E-15));
#105688=CARTESIAN_POINT('Ctrl Pts',(-2.27314775465957,1.63815729286034,
1.03894163369803E-15));
#105689=CARTESIAN_POINT('Ctrl Pts',(-2.22224770950079,1.71903655485284,
8.32667268468867E-16));
#105690=CARTESIAN_POINT('Ctrl Pts',(-2.19258578684687,1.76616881978589,
7.12461200913758E-16));
#105691=CARTESIAN_POINT('Ctrl Pts',(-2.16154735127789,1.8125146430568,-3.53624849731269E-16));
#105692=CARTESIAN_POINT('Ctrl Pts',(-2.12916581821013,1.85800875267655,
-4.44089209850063E-16));
#105693=CARTESIAN_POINT('Ctrl Pts',(-2.12064615841252,1.8699783631315,-5.70106170484684E-16));
#105694=CARTESIAN_POINT('Ctrl Pts',(-2.11203197224998,1.88189106910177,
4.99191063271152E-16));
#105695=CARTESIAN_POINT('Ctrl Pts',(-2.10332881249318,1.89373885098382,
4.44089209850063E-16));
#105696=CARTESIAN_POINT('Ctrl Pts',(-2.04513073725928,1.97296503096835,
6.63206793642155E-16));
#105697=CARTESIAN_POINT('Ctrl Pts',(-1.98310309941755,2.04909488477598,
2.85493467669587E-17));
#105698=CARTESIAN_POINT('Ctrl Pts',(-1.91752051055856,2.12182013150207,
1.27675647831893E-15));
#105699=CARTESIAN_POINT('Ctrl Pts',(-1.85172508404381,2.19478139622161,
2.51589036252178E-15));
#105700=CARTESIAN_POINT('Ctrl Pts',(-1.78235120221478,2.26431682197845,
2.36153937213606E-15));
#105701=CARTESIAN_POINT('Ctrl Pts',(-1.70962567801232,2.33010034792287,
1.66533453693773E-16));
#105702=CARTESIAN_POINT('Ctrl Pts',(-1.63825968478638,2.39465411660879,
-1.03982216055884E-15));
#105703=CARTESIAN_POINT('Ctrl Pts',(-1.56366566082645,2.45559572732805,
8.15654749631012E-16));
#105704=CARTESIAN_POINT('Ctrl Pts',(-1.48601649839977,2.51259054837298,
0.));
#105705=CARTESIAN_POINT('Ctrl Pts',(-1.42234737003875,2.55932396395166,
-4.16838681284198E-16));
#105706=CARTESIAN_POINT('Ctrl Pts',(-1.35662332229989,2.60340355803474,
-4.62859095806204E-17));
#105707=CARTESIAN_POINT('Ctrl Pts',(-1.28892185405323,2.64462557919717,
2.77555756156289E-16));
#105708=CARTESIAN_POINT('Ctrl Pts',(-1.37727721526601,-1.93088206134116,
-0.0011160887762518));
#105709=CARTESIAN_POINT('Ctrl Pts',(-1.36872530799275,-1.93698204397104,
-0.000744059184169721));
#105710=CARTESIAN_POINT('Ctrl Pts',(-1.36013287474801,-1.94302521096248,
-0.00037202959208763));
#105711=CARTESIAN_POINT('Ctrl Pts',(-1.35150067398999,-1.94901102888224,
-5.55111512312578E-15));
#105712=CARTESIAN_POINT('Origin',(-1.44337567297407,-2.5,-6.));
#105713=CARTESIAN_POINT('',(-1.44337567297407,-2.5,-6.));
#105714=CARTESIAN_POINT('',(1.44337567297406,-2.5,-6.));
#105715=CARTESIAN_POINT('',(-0.721687836487033,-2.5,-6.));
#105716=CARTESIAN_POINT('',(-1.44337567297407,-2.5,-3.));
#105717=CARTESIAN_POINT('',(-1.44337567297407,-2.5,-6.));
#105718=CARTESIAN_POINT('',(1.44337567297406,-2.5,-3.));
#105719=CARTESIAN_POINT('',(-1.44337567297407,-2.5,-3.));
#105720=CARTESIAN_POINT('',(1.44337567297406,-2.5,-6.));
#105721=CARTESIAN_POINT('Origin',(-2.88675134594813,3.53525079574969E-16,
-6.));
#105722=CARTESIAN_POINT('',(-2.88675134594813,3.53525079574969E-16,-6.));
#105723=CARTESIAN_POINT('',(-2.52590742770461,-0.625,-6.));
#105724=CARTESIAN_POINT('',(-2.88675134594813,5.55111512312578E-16,-3.));
#105725=CARTESIAN_POINT('',(-2.88675134594813,3.53525079574969E-16,-6.));
#105726=CARTESIAN_POINT('',(-2.88675134594813,3.53525079574969E-16,-3.));
#105727=CARTESIAN_POINT('Origin',(-1.44337567297406,2.5,-6.));
#105728=CARTESIAN_POINT('',(-1.44337567297406,2.5,-6.));
#105729=CARTESIAN_POINT('',(-1.80421959121758,1.875,-6.));
#105730=CARTESIAN_POINT('',(-1.44337567297406,2.5,-3.));
#105731=CARTESIAN_POINT('',(-1.44337567297406,2.5,-6.));
#105732=CARTESIAN_POINT('',(-1.44337567297406,2.5,-3.));
#105733=CARTESIAN_POINT('Origin',(1.44337567297406,2.5,-6.));
#105734=CARTESIAN_POINT('',(1.44337567297406,2.5,-6.));
#105735=CARTESIAN_POINT('',(0.721687836487033,2.5,-6.));
#105736=CARTESIAN_POINT('',(1.44337567297406,2.5,-3.));
#105737=CARTESIAN_POINT('',(1.44337567297406,2.5,-6.));
#105738=CARTESIAN_POINT('',(1.44337567297406,2.5,-3.));
#105739=CARTESIAN_POINT('Origin',(2.88675134594813,0.,-6.));
#105740=CARTESIAN_POINT('',(2.88675134594813,0.,-6.));
#105741=CARTESIAN_POINT('',(2.52590742770461,0.625,-6.));
#105742=CARTESIAN_POINT('',(2.88675134594813,0.,-3.));
#105743=CARTESIAN_POINT('',(2.88675134594813,0.,-6.));
#105744=CARTESIAN_POINT('',(2.88675134594813,0.,-3.));
#105745=CARTESIAN_POINT('Origin',(1.44337567297406,-2.5,-6.));
#105746=CARTESIAN_POINT('',(1.80421959121758,-1.875,-6.));
#105747=CARTESIAN_POINT('',(1.44337567297406,-2.5,-3.));
#105748=CARTESIAN_POINT('Origin',(0.,0.,-3.));
#105749=CARTESIAN_POINT('Origin',(0.,0.,0.));
#105750=CARTESIAN_POINT('',(-5.,-6.12323399573677E-16,0.));
#105751=CARTESIAN_POINT('Origin',(0.,0.,0.));
#105752=CARTESIAN_POINT('Origin',(0.,0.,-6.));
#105753=CARTESIAN_POINT('',(-5.,-6.12323399573677E-16,-6.));
#105754=CARTESIAN_POINT('',(-5.,-6.12323399573677E-16,-6.));
#105755=CARTESIAN_POINT('Origin',(0.,0.,-6.));
#105756=CARTESIAN_POINT('Origin',(0.,0.,-6.));
#105757=CARTESIAN_POINT('Origin',(0.,0.,25.));
#105758=CARTESIAN_POINT('',(0.,0.,0.));
#105759=CARTESIAN_POINT('',(0.,0.,52.));
#105760=CARTESIAN_POINT('',(87.5044647016809,-2.26829488139857E-46,52.));
#105761=CARTESIAN_POINT('',(20.,0.,52.));
#105762=CARTESIAN_POINT('',(0.,-35.,52.));
#105763=CARTESIAN_POINT('',(201.,-35.,52.));
#105764=CARTESIAN_POINT('',(87.5044647016809,-35.,52.));
#105765=CARTESIAN_POINT('',(87.5044647016809,-2.26829488139857E-46,52.));
#105766=CARTESIAN_POINT('',(267.504464701681,2.98372437868011E-15,52.));
#105767=CARTESIAN_POINT('',(85.5044647016809,-2.26829488139857E-46,52.));
#105768=CARTESIAN_POINT('',(84.5044647016817,1.52378110129803E-13,52.0000000000001));
#105769=CARTESIAN_POINT('',(0.,-15.,52.));
#105770=CARTESIAN_POINT('',(180.,0.,52.));
#105771=CARTESIAN_POINT('',(81.5044647016809,-2.26829488139857E-46,52.));
#105772=CARTESIAN_POINT('',(0.,35.,52.));
#105773=CARTESIAN_POINT('',(201.,35.,52.));
#105774=CARTESIAN_POINT('',(87.5044647016809,35.,52.));
#105775=CARTESIAN_POINT('',(107.504464701681,-2.26829488139856E-46,52.));
#105776=CARTESIAN_POINT('',(0.,15.,52.));
#105777=CARTESIAN_POINT('',(107.504464701681,-15.,52.));
#105778=CARTESIAN_POINT('',(107.504464701681,15.,52.));
#105779=UNCERTAINTY_MEASURE_WITH_UNIT(LENGTH_MEASURE(0.01),#105807,
'DISTANCE_ACCURACY_VALUE',
'Maximum model space distance between geometric entities at asserted c
onnectivities');
#105780=UNCERTAINTY_MEASURE_WITH_UNIT(LENGTH_MEASURE(0.01),#105807,
'DISTANCE_ACCURACY_VALUE',
'Maximum model space distance between geometric entities at asserted c
onnectivities');
#105781=UNCERTAINTY_MEASURE_WITH_UNIT(LENGTH_MEASURE(0.01),#105807,
'DISTANCE_ACCURACY_VALUE',
'Maximum model space distance between geometric entities at asserted c
onnectivities');
#105782=UNCERTAINTY_MEASURE_WITH_UNIT(LENGTH_MEASURE(0.01),#105807,
'DISTANCE_ACCURACY_VALUE',
'Maximum model space distance between geometric entities at asserted c
onnectivities');
#105783=UNCERTAINTY_MEASURE_WITH_UNIT(LENGTH_MEASURE(0.01),#105807,
'DISTANCE_ACCURACY_VALUE',
'Maximum model space distance between geometric entities at asserted c
onnectivities');
#105784=UNCERTAINTY_MEASURE_WITH_UNIT(LENGTH_MEASURE(0.01),#105807,
'DISTANCE_ACCURACY_VALUE',
'Maximum model space distance between geometric entities at asserted c
onnectivities');
#105785=UNCERTAINTY_MEASURE_WITH_UNIT(LENGTH_MEASURE(0.01),#105807,
'DISTANCE_ACCURACY_VALUE',
'Maximum model space distance between geometric entities at asserted c
onnectivities');
#105786=UNCERTAINTY_MEASURE_WITH_UNIT(LENGTH_MEASURE(0.01),#105807,
'DISTANCE_ACCURACY_VALUE',
'Maximum model space distance between geometric entities at asserted c
onnectivities');
#105787=UNCERTAINTY_MEASURE_WITH_UNIT(LENGTH_MEASURE(0.01),#105807,
'DISTANCE_ACCURACY_VALUE',
'Maximum model space distance between geometric entities at asserted c
onnectivities');
#105788=UNCERTAINTY_MEASURE_WITH_UNIT(LENGTH_MEASURE(0.01),#105807,
'DISTANCE_ACCURACY_VALUE',
'Maximum model space distance between geometric entities at asserted c
onnectivities');
#105789=UNCERTAINTY_MEASURE_WITH_UNIT(LENGTH_MEASURE(0.01),#105807,
'DISTANCE_ACCURACY_VALUE',
'Maximum model space distance between geometric entities at asserted c
onnectivities');
#105790=UNCERTAINTY_MEASURE_WITH_UNIT(LENGTH_MEASURE(0.01),#105807,
'DISTANCE_ACCURACY_VALUE',
'Maximum model space distance between geometric entities at asserted c
onnectivities');
#105791=UNCERTAINTY_MEASURE_WITH_UNIT(LENGTH_MEASURE(0.01),#105807,
'DISTANCE_ACCURACY_VALUE',
'Maximum model space distance between geometric entities at asserted c
onnectivities');
#105792=UNCERTAINTY_MEASURE_WITH_UNIT(LENGTH_MEASURE(0.01),#105807,
'DISTANCE_ACCURACY_VALUE',
'Maximum model space distance between geometric entities at asserted c
onnectivities');
#105793=(
GEOMETRIC_REPRESENTATION_CONTEXT(3)
GLOBAL_UNCERTAINTY_ASSIGNED_CONTEXT((#105779))
GLOBAL_UNIT_ASSIGNED_CONTEXT((#105807,#105809,#105810))
REPRESENTATION_CONTEXT('','3D')
);
#105794=(
GEOMETRIC_REPRESENTATION_CONTEXT(3)
GLOBAL_UNCERTAINTY_ASSIGNED_CONTEXT((#105780))
GLOBAL_UNIT_ASSIGNED_CONTEXT((#105807,#105809,#105810))
REPRESENTATION_CONTEXT('','3D')
);
#105795=(
GEOMETRIC_REPRESENTATION_CONTEXT(3)
GLOBAL_UNCERTAINTY_ASSIGNED_CONTEXT((#105781))
GLOBAL_UNIT_ASSIGNED_CONTEXT((#105807,#105809,#105810))
REPRESENTATION_CONTEXT('','3D')
);
#105796=(
GEOMETRIC_REPRESENTATION_CONTEXT(3)
GLOBAL_UNCERTAINTY_ASSIGNED_CONTEXT((#105782))
GLOBAL_UNIT_ASSIGNED_CONTEXT((#105807,#105809,#105810))
REPRESENTATION_CONTEXT('','3D')
);
#105797=(
GEOMETRIC_REPRESENTATION_CONTEXT(3)
GLOBAL_UNCERTAINTY_ASSIGNED_CONTEXT((#105783))
GLOBAL_UNIT_ASSIGNED_CONTEXT((#105807,#105809,#105810))
REPRESENTATION_CONTEXT('','3D')
);
#105798=(
GEOMETRIC_REPRESENTATION_CONTEXT(3)
GLOBAL_UNCERTAINTY_ASSIGNED_CONTEXT((#105784))
GLOBAL_UNIT_ASSIGNED_CONTEXT((#105807,#105809,#105810))
REPRESENTATION_CONTEXT('','3D')
);
#105799=(
GEOMETRIC_REPRESENTATION_CONTEXT(3)
GLOBAL_UNCERTAINTY_ASSIGNED_CONTEXT((#105785))
GLOBAL_UNIT_ASSIGNED_CONTEXT((#105807,#105809,#105810))
REPRESENTATION_CONTEXT('','3D')
);
#105800=(
GEOMETRIC_REPRESENTATION_CONTEXT(3)
GLOBAL_UNCERTAINTY_ASSIGNED_CONTEXT((#105786))
GLOBAL_UNIT_ASSIGNED_CONTEXT((#105807,#105809,#105810))
REPRESENTATION_CONTEXT('','3D')
);
#105801=(
GEOMETRIC_REPRESENTATION_CONTEXT(3)
GLOBAL_UNCERTAINTY_ASSIGNED_CONTEXT((#105787))
GLOBAL_UNIT_ASSIGNED_CONTEXT((#105807,#105809,#105810))
REPRESENTATION_CONTEXT('','3D')
);
#105802=(
GEOMETRIC_REPRESENTATION_CONTEXT(3)
GLOBAL_UNCERTAINTY_ASSIGNED_CONTEXT((#105788))
GLOBAL_UNIT_ASSIGNED_CONTEXT((#105807,#105809,#105810))
REPRESENTATION_CONTEXT('','3D')
);
#105803=(
GEOMETRIC_REPRESENTATION_CONTEXT(3)
GLOBAL_UNCERTAINTY_ASSIGNED_CONTEXT((#105789))
GLOBAL_UNIT_ASSIGNED_CONTEXT((#105807,#105809,#105810))
REPRESENTATION_CONTEXT('','3D')
);
#105804=(
GEOMETRIC_REPRESENTATION_CONTEXT(3)
GLOBAL_UNCERTAINTY_ASSIGNED_CONTEXT((#105790))
GLOBAL_UNIT_ASSIGNED_CONTEXT((#105807,#105809,#105810))
REPRESENTATION_CONTEXT('','3D')
);
#105805=(
GEOMETRIC_REPRESENTATION_CONTEXT(3)
GLOBAL_UNCERTAINTY_ASSIGNED_CONTEXT((#105791))
GLOBAL_UNIT_ASSIGNED_CONTEXT((#105807,#105809,#105810))
REPRESENTATION_CONTEXT('','3D')
);
#105806=(
GEOMETRIC_REPRESENTATION_CONTEXT(3)
GLOBAL_UNCERTAINTY_ASSIGNED_CONTEXT((#105792))
GLOBAL_UNIT_ASSIGNED_CONTEXT((#105807,#105809,#105810))
REPRESENTATION_CONTEXT('','3D')
);
#105807=(
LENGTH_UNIT()
NAMED_UNIT(*)
SI_UNIT(.MILLI.,.METRE.)
);
#105808=(
LENGTH_UNIT()
NAMED_UNIT(*)
SI_UNIT($,.METRE.)
);
#105809=(
NAMED_UNIT(*)
PLANE_ANGLE_UNIT()
SI_UNIT($,.RADIAN.)
);
#105810=(
NAMED_UNIT(*)
SI_UNIT($,.STERADIAN.)
SOLID_ANGLE_UNIT()
);
#105811=SHAPE_DEFINITION_REPRESENTATION(#105824,#105858);
#105812=SHAPE_DEFINITION_REPRESENTATION(#105825,#105859);
#105813=SHAPE_DEFINITION_REPRESENTATION(#105826,#105860);
#105814=SHAPE_DEFINITION_REPRESENTATION(#105827,#105861);
#105815=SHAPE_DEFINITION_REPRESENTATION(#105828,#105862);
#105816=SHAPE_DEFINITION_REPRESENTATION(#105829,#105863);
#105817=SHAPE_DEFINITION_REPRESENTATION(#105830,#105864);
#105818=SHAPE_DEFINITION_REPRESENTATION(#105831,#105865);
#105819=SHAPE_DEFINITION_REPRESENTATION(#105832,#105866);
#105820=SHAPE_DEFINITION_REPRESENTATION(#105833,#105867);
#105821=SHAPE_DEFINITION_REPRESENTATION(#105834,#105868);
#105822=SHAPE_DEFINITION_REPRESENTATION(#105835,#105869);
#105823=SHAPE_DEFINITION_REPRESENTATION(#105836,#105870);
#105824=PRODUCT_DEFINITION_SHAPE('',$,#105872);
#105825=PRODUCT_DEFINITION_SHAPE('',$,#105873);
#105826=PRODUCT_DEFINITION_SHAPE('',$,#105874);
#105827=PRODUCT_DEFINITION_SHAPE('',$,#105875);
#105828=PRODUCT_DEFINITION_SHAPE('',$,#105876);
#105829=PRODUCT_DEFINITION_SHAPE('',$,#105877);
#105830=PRODUCT_DEFINITION_SHAPE('',$,#105878);
#105831=PRODUCT_DEFINITION_SHAPE('',$,#105879);
#105832=PRODUCT_DEFINITION_SHAPE('',$,#105880);
#105833=PRODUCT_DEFINITION_SHAPE('',$,#105881);
#105834=PRODUCT_DEFINITION_SHAPE('',$,#105882);
#105835=PRODUCT_DEFINITION_SHAPE('',$,#105883);
#105836=PRODUCT_DEFINITION_SHAPE('',$,#105884);
#105837=PRODUCT_DEFINITION_SHAPE($,$,#74);
#105838=PRODUCT_DEFINITION_SHAPE($,$,#75);
#105839=PRODUCT_DEFINITION_SHAPE($,$,#76);
#105840=PRODUCT_DEFINITION_SHAPE($,$,#77);
#105841=PRODUCT_DEFINITION_SHAPE($,$,#78);
#105842=PRODUCT_DEFINITION_SHAPE($,$,#79);
#105843=PRODUCT_DEFINITION_SHAPE($,$,#80);
#105844=PRODUCT_DEFINITION_SHAPE($,$,#81);
#105845=PRODUCT_DEFINITION_SHAPE($,$,#82);
#105846=PRODUCT_DEFINITION_SHAPE($,$,#83);
#105847=PRODUCT_DEFINITION_SHAPE($,$,#84);
#105848=PRODUCT_DEFINITION_SHAPE($,$,#85);
#105849=PRODUCT_DEFINITION_SHAPE($,$,#86);
#105850=PRODUCT_DEFINITION_SHAPE($,$,#87);
#105851=PRODUCT_DEFINITION_SHAPE($,$,#88);
#105852=PRODUCT_DEFINITION_SHAPE($,$,#89);
#105853=PRODUCT_DEFINITION_SHAPE($,$,#90);
#105854=PRODUCT_DEFINITION_SHAPE($,$,#91);
#105855=PRODUCT_DEFINITION_SHAPE($,$,#92);
#105856=PRODUCT_DEFINITION_SHAPE($,$,#93);
#105857=PRODUCT_DEFINITION_SHAPE($,$,#94);
#105858=SHAPE_REPRESENTATION('',(#7347,#7722,#7723,#7724,#7725,#7726,#7727,
#7728,#7729,#7730,#7731,#7732,#7733,#7734,#7735,#7736,#7737,#7738,#7739,
#7740,#7741,#7742),#105793);
#105859=SHAPE_REPRESENTATION('',(#7348),#105794);
#105860=SHAPE_REPRESENTATION('',(#7367),#105795);
#105861=SHAPE_REPRESENTATION('',(#7389),#105796);
#105862=SHAPE_REPRESENTATION('',(#7398),#105797);
#105863=SHAPE_REPRESENTATION('',(#7527),#105798);
#105864=SHAPE_REPRESENTATION('',(#7538),#105799);
#105865=SHAPE_REPRESENTATION('',(#7583),#105800);
#105866=SHAPE_REPRESENTATION('',(#7629),#105801);
#105867=SHAPE_REPRESENTATION('',(#7647),#105802);
#105868=SHAPE_REPRESENTATION('',(#7658),#105803);
#105869=SHAPE_REPRESENTATION('',(#7667),#105804);
#105870=SHAPE_REPRESENTATION('',(#7676),#105805);
#105871=PRODUCT_DEFINITION_CONTEXT('part definition',#105912,'design');
#105872=PRODUCT_DEFINITION('MAS-636','TAS-013',#105885,#105871);
#105873=PRODUCT_DEFINITION('Base plate','Base plate',#105886,#105871);
#105874=PRODUCT_DEFINITION('Moving jaw','Moving jaw',#105887,#105871);
#105875=PRODUCT_DEFINITION('Spindle journal bushing',
'Spindle journal bushing',#105888,#105871);
#105876=PRODUCT_DEFINITION('Clamping spindle','Clamping spindle',#105889,
#105871);
#105877=PRODUCT_DEFINITION('Pivot retaining ring',
'Pivot retaining ring',#105890,#105871);
#105878=PRODUCT_DEFINITION('End support','End support',#105891,#105871);
#105879=PRODUCT_DEFINITION('Jaw pad','Jaw pad',#105892,#105871);
#105880=PRODUCT_DEFINITION('Guide rod','Guide rod',#105893,#105871);
#105881=PRODUCT_DEFINITION('Guide retaining ring',
'Guide retaining ring',#105894,#105871);
#105882=PRODUCT_DEFINITION('Guide bushing','Guide bushing',#105895,#105871);
#105883=PRODUCT_DEFINITION('Pivot washer','Pivot washer',#105896,#105871);
#105884=PRODUCT_DEFINITION('Socket head cap screw M6x25',
'Socket head cap screw M6x25',#105897,#105871);
#105885=PRODUCT_DEFINITION_FORMATION('',$,#105914);
#105886=PRODUCT_DEFINITION_FORMATION('',$,#105915);
#105887=PRODUCT_DEFINITION_FORMATION('',$,#105916);
#105888=PRODUCT_DEFINITION_FORMATION('',$,#105917);
#105889=PRODUCT_DEFINITION_FORMATION('',$,#105918);
#105890=PRODUCT_DEFINITION_FORMATION('',$,#105919);
#105891=PRODUCT_DEFINITION_FORMATION('',$,#105920);
#105892=PRODUCT_DEFINITION_FORMATION('',$,#105921);
#105893=PRODUCT_DEFINITION_FORMATION('',$,#105922);
#105894=PRODUCT_DEFINITION_FORMATION('',$,#105923);
#105895=PRODUCT_DEFINITION_FORMATION('',$,#105924);
#105896=PRODUCT_DEFINITION_FORMATION('',$,#105925);
#105897=PRODUCT_DEFINITION_FORMATION('',$,#105926);
#105898=PRODUCT_RELATED_PRODUCT_CATEGORY('TAS-013','TAS-013',(#105914));
#105899=PRODUCT_RELATED_PRODUCT_CATEGORY('Base plate','Base plate',(#105915));
#105900=PRODUCT_RELATED_PRODUCT_CATEGORY('Moving jaw','Moving jaw',(#105916));
#105901=PRODUCT_RELATED_PRODUCT_CATEGORY('Spindle journal bushing',
'Spindle journal bushing',(#105917));
#105902=PRODUCT_RELATED_PRODUCT_CATEGORY('Clamping spindle',
'Clamping spindle',(#105918));
#105903=PRODUCT_RELATED_PRODUCT_CATEGORY('Pivot retaining ring',
'Pivot retaining ring',(#105919));
#105904=PRODUCT_RELATED_PRODUCT_CATEGORY('End support','End support',(#105920));
#105905=PRODUCT_RELATED_PRODUCT_CATEGORY('Jaw pad','Jaw pad',(#105921));
#105906=PRODUCT_RELATED_PRODUCT_CATEGORY('Guide rod','Guide rod',(#105922));
#105907=PRODUCT_RELATED_PRODUCT_CATEGORY('Guide retaining ring',
'Guide retaining ring',(#105923));
#105908=PRODUCT_RELATED_PRODUCT_CATEGORY('Guide bushing',
'Guide bushing',(#105924));
#105909=PRODUCT_RELATED_PRODUCT_CATEGORY('Pivot washer','Pivot washer',
(#105925));
#105910=PRODUCT_RELATED_PRODUCT_CATEGORY('Socket head cap screw M6x25',
'Socket head cap screw M6x25',(#105926));
#105911=APPLICATION_PROTOCOL_DEFINITION('international standard',
'automotive_design',2009,#105912);
#105912=APPLICATION_CONTEXT(
'Core Data for Automotive Mechanical Design Process');
#105913=PRODUCT_CONTEXT('part definition',#105912,'mechanical');
#105914=PRODUCT('MAS-636','TAS-013',
'Independent guided parallel-jaw bracket clamp. Two12mm guide rods, re
placeable bronze sleeves, captured swiveling spindle, replaceable jaw 
pads and modeled M16x2 screw. Native slider/revolute joints linked2mm 
per revolution. Nominal opening0..122 with initial28mm. Base and two i
dentical supports welded. Standard fits, weld details and clamp load r
equire engineering selection.',(#105913));
#105915=PRODUCT('Base plate','Base plate','Base plate',(#105913));
#105916=PRODUCT('Moving jaw','Moving jaw','Moving jaw',(#105913));
#105917=PRODUCT('Spindle journal bushing','Spindle journal bushing',$,(#105913));
#105918=PRODUCT('Clamping spindle','Clamping spindle',$,(#105913));
#105919=PRODUCT('Pivot retaining ring','Pivot retaining ring',$,(#105913));
#105920=PRODUCT('End support','End support',$,(#105913));
#105921=PRODUCT('Jaw pad','Jaw pad',$,(#105913));
#105922=PRODUCT('Guide rod','Guide rod',$,(#105913));
#105923=PRODUCT('Guide retaining ring','Guide retaining ring',$,(#105913));
#105924=PRODUCT('Guide bushing','Guide bushing',$,(#105913));
#105925=PRODUCT('Pivot washer','Pivot washer',$,(#105913));
#105926=PRODUCT('Socket head cap screw M6x25',
'Socket head cap screw M6x25',$,(#105913));
#105927=PRESENTATION_STYLE_ASSIGNMENT((#105933));
#105928=PRESENTATION_STYLE_ASSIGNMENT((#105934));
#105929=PRESENTATION_STYLE_ASSIGNMENT((#105935));
#105930=PRESENTATION_STYLE_ASSIGNMENT((#105936));
#105931=PRESENTATION_STYLE_ASSIGNMENT((#105937));
#105932=PRESENTATION_STYLE_ASSIGNMENT((#105938));
#105933=SURFACE_STYLE_USAGE(.BOTH.,#105939);
#105934=SURFACE_STYLE_USAGE(.BOTH.,#105940);
#105935=SURFACE_STYLE_USAGE(.BOTH.,#105941);
#105936=SURFACE_STYLE_USAGE(.BOTH.,#105942);
#105937=SURFACE_STYLE_USAGE(.BOTH.,#105943);
#105938=SURFACE_STYLE_USAGE(.BOTH.,#105944);
#105939=SURFACE_SIDE_STYLE('',(#105945));
#105940=SURFACE_SIDE_STYLE('',(#105946));
#105941=SURFACE_SIDE_STYLE('',(#105947));
#105942=SURFACE_SIDE_STYLE('',(#105948));
#105943=SURFACE_SIDE_STYLE('',(#105949));
#105944=SURFACE_SIDE_STYLE('',(#105950));
#105945=SURFACE_STYLE_FILL_AREA(#105951);
#105946=SURFACE_STYLE_FILL_AREA(#105952);
#105947=SURFACE_STYLE_FILL_AREA(#105953);
#105948=SURFACE_STYLE_FILL_AREA(#105954);
#105949=SURFACE_STYLE_FILL_AREA(#105955);
#105950=SURFACE_STYLE_FILL_AREA(#105956);
#105951=FILL_AREA_STYLE('Steel - Satin',(#105957));
#105952=FILL_AREA_STYLE('Opaque(104,114,127)',(#105958));
#105953=FILL_AREA_STYLE('Opaque(81,175,227)',(#105959));
#105954=FILL_AREA_STYLE('Opaque(185,192,202)',(#105960));
#105955=FILL_AREA_STYLE('Opaque(23,69,131)',(#105961));
#105956=FILL_AREA_STYLE('Opaque(64,72,82)',(#105962));
#105957=FILL_AREA_STYLE_COLOUR('Steel - Satin',#105963);
#105958=FILL_AREA_STYLE_COLOUR('Opaque(104,114,127)',#105964);
#105959=FILL_AREA_STYLE_COLOUR('Opaque(81,175,227)',#105965);
#105960=FILL_AREA_STYLE_COLOUR('Opaque(185,192,202)',#105966);
#105961=FILL_AREA_STYLE_COLOUR('Opaque(23,69,131)',#105967);
#105962=FILL_AREA_STYLE_COLOUR('Opaque(64,72,82)',#105968);
#105963=COLOUR_RGB('Steel - Satin',0.627450980392157,0.627450980392157,
0.627450980392157);
#105964=COLOUR_RGB('Opaque(104,114,127)',0.407843137254902,0.447058823529412,
0.498039215686275);
#105965=COLOUR_RGB('Opaque(81,175,227)',0.317647058823529,0.686274509803922,
0.890196078431372);
#105966=COLOUR_RGB('Opaque(185,192,202)',0.725490196078431,0.752941176470588,
0.792156862745098);
#105967=COLOUR_RGB('Opaque(23,69,131)',0.0901960784313725,0.270588235294118,
0.513725490196078);
#105968=COLOUR_RGB('Opaque(64,72,82)',0.250980392156863,0.282352941176471,
0.32156862745098);
ENDSEC;
END-ISO-10303-21;
